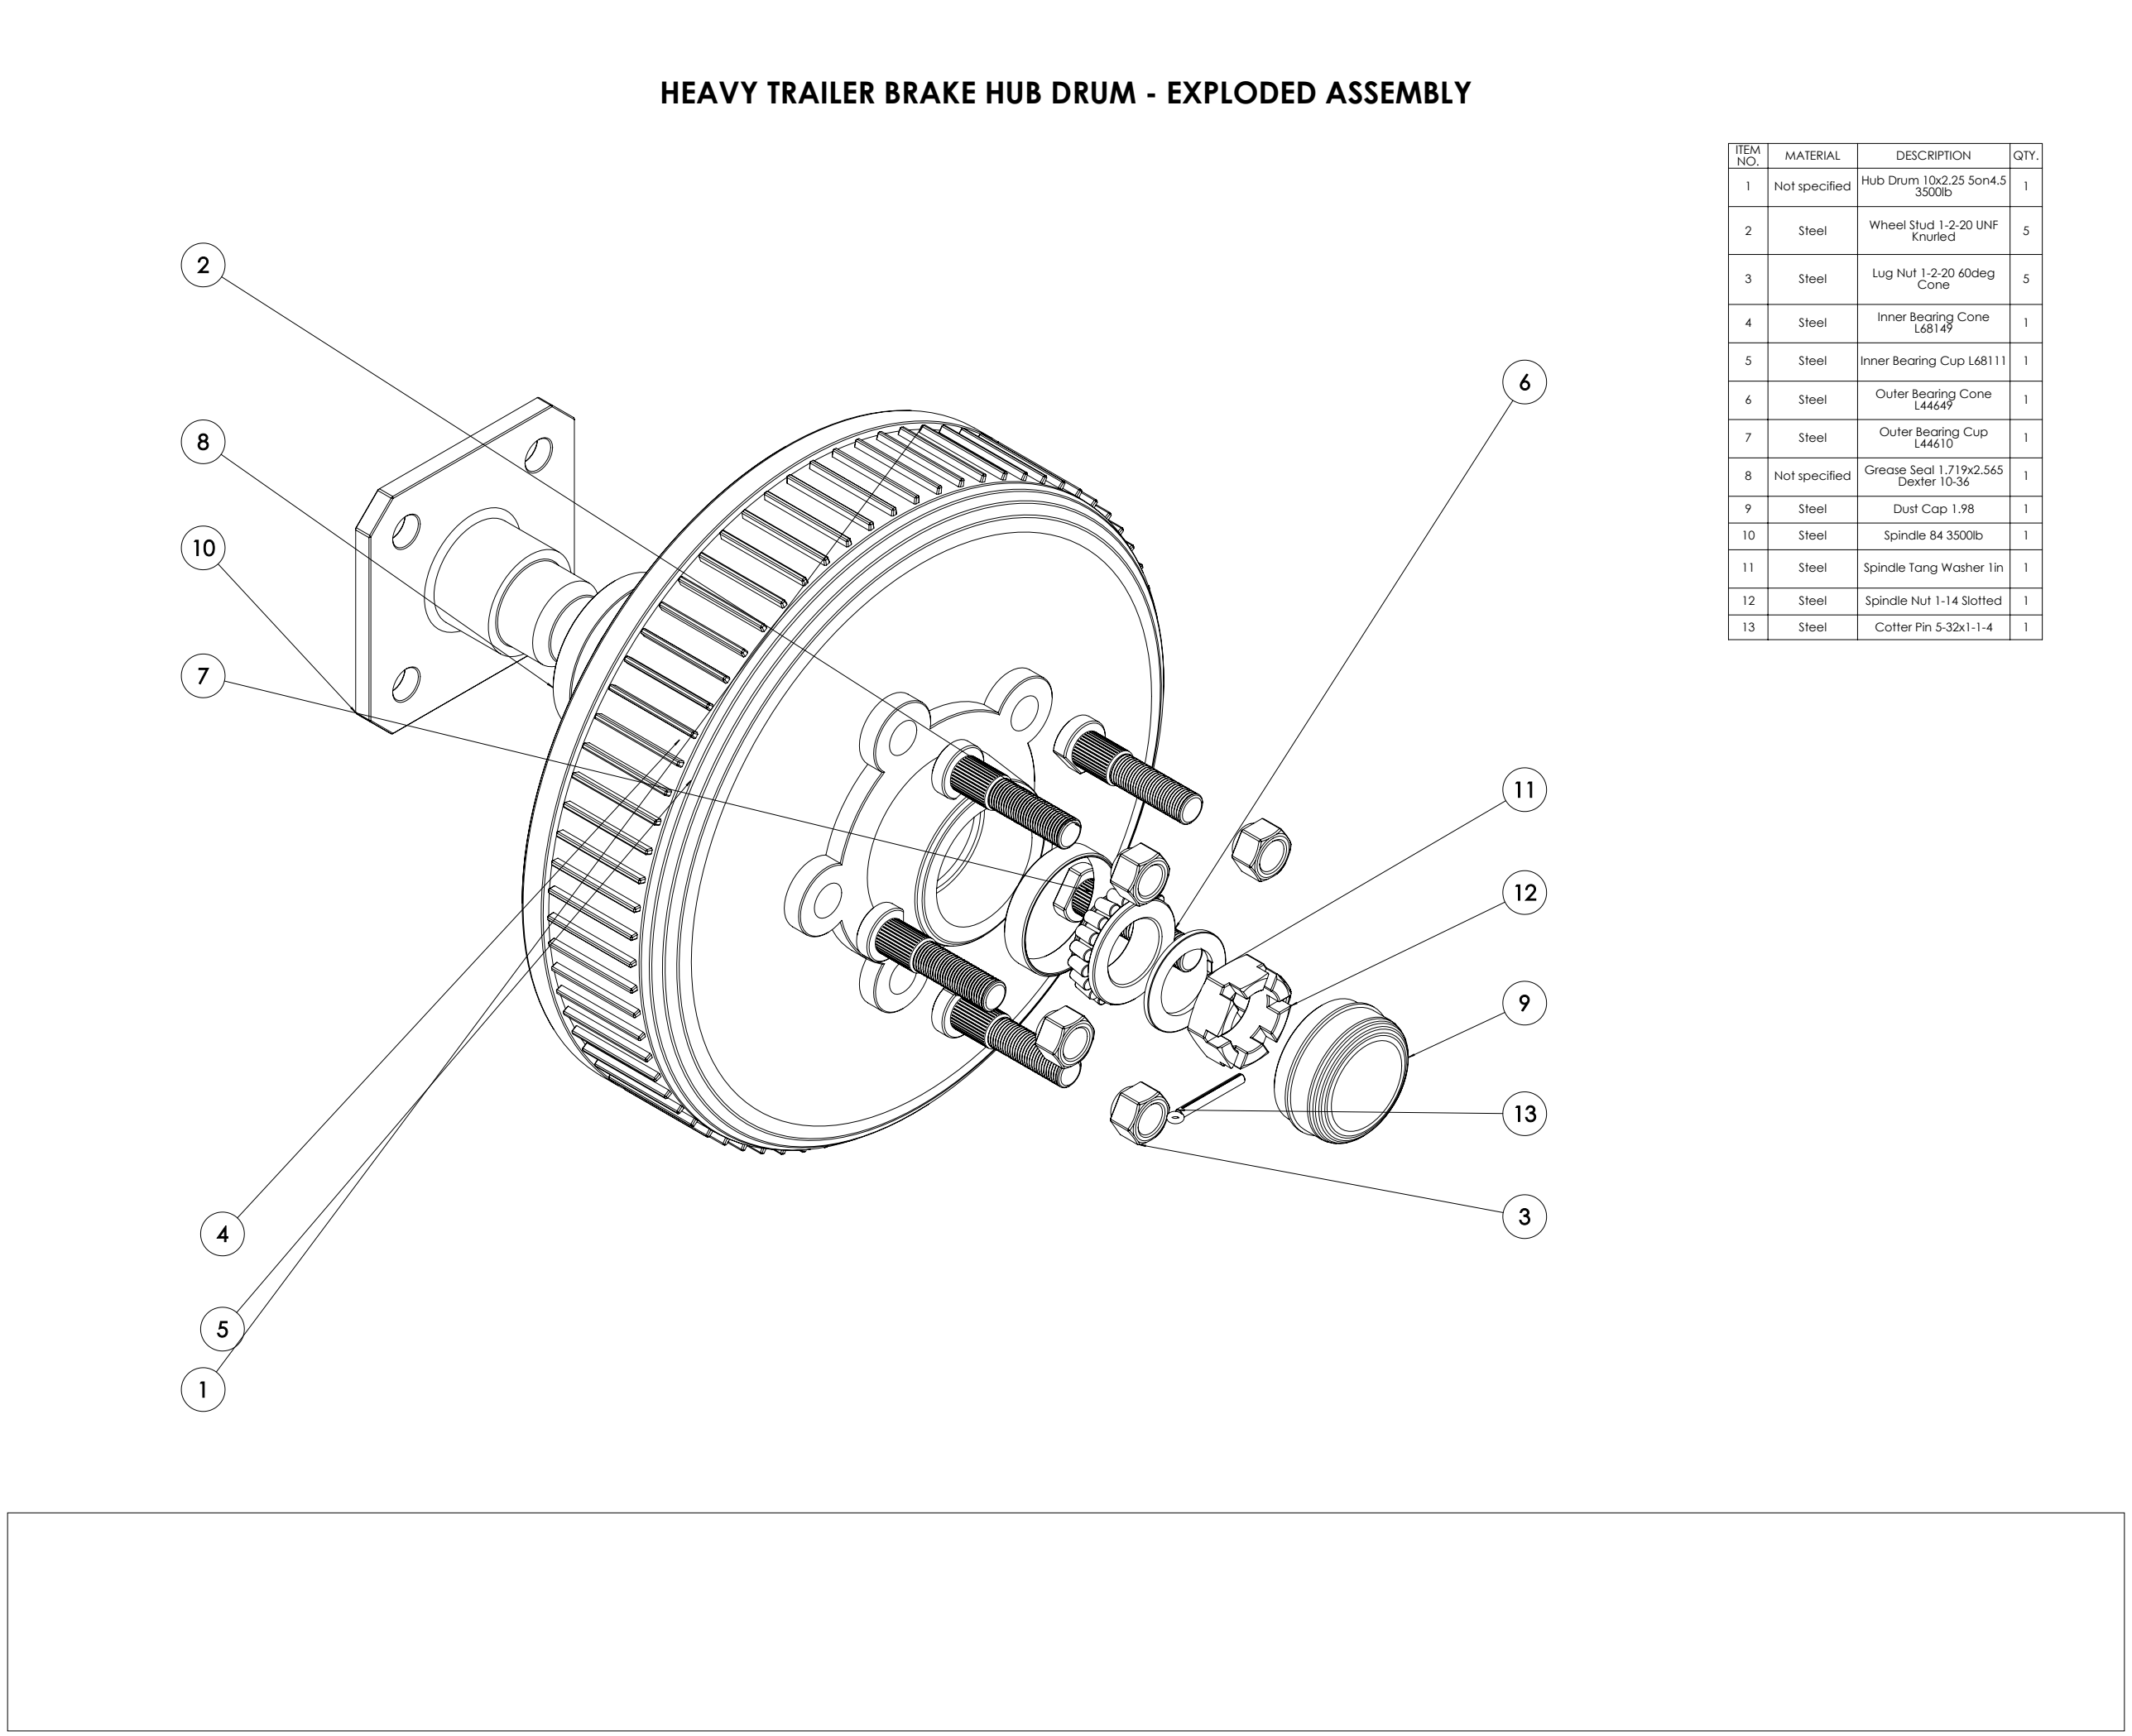
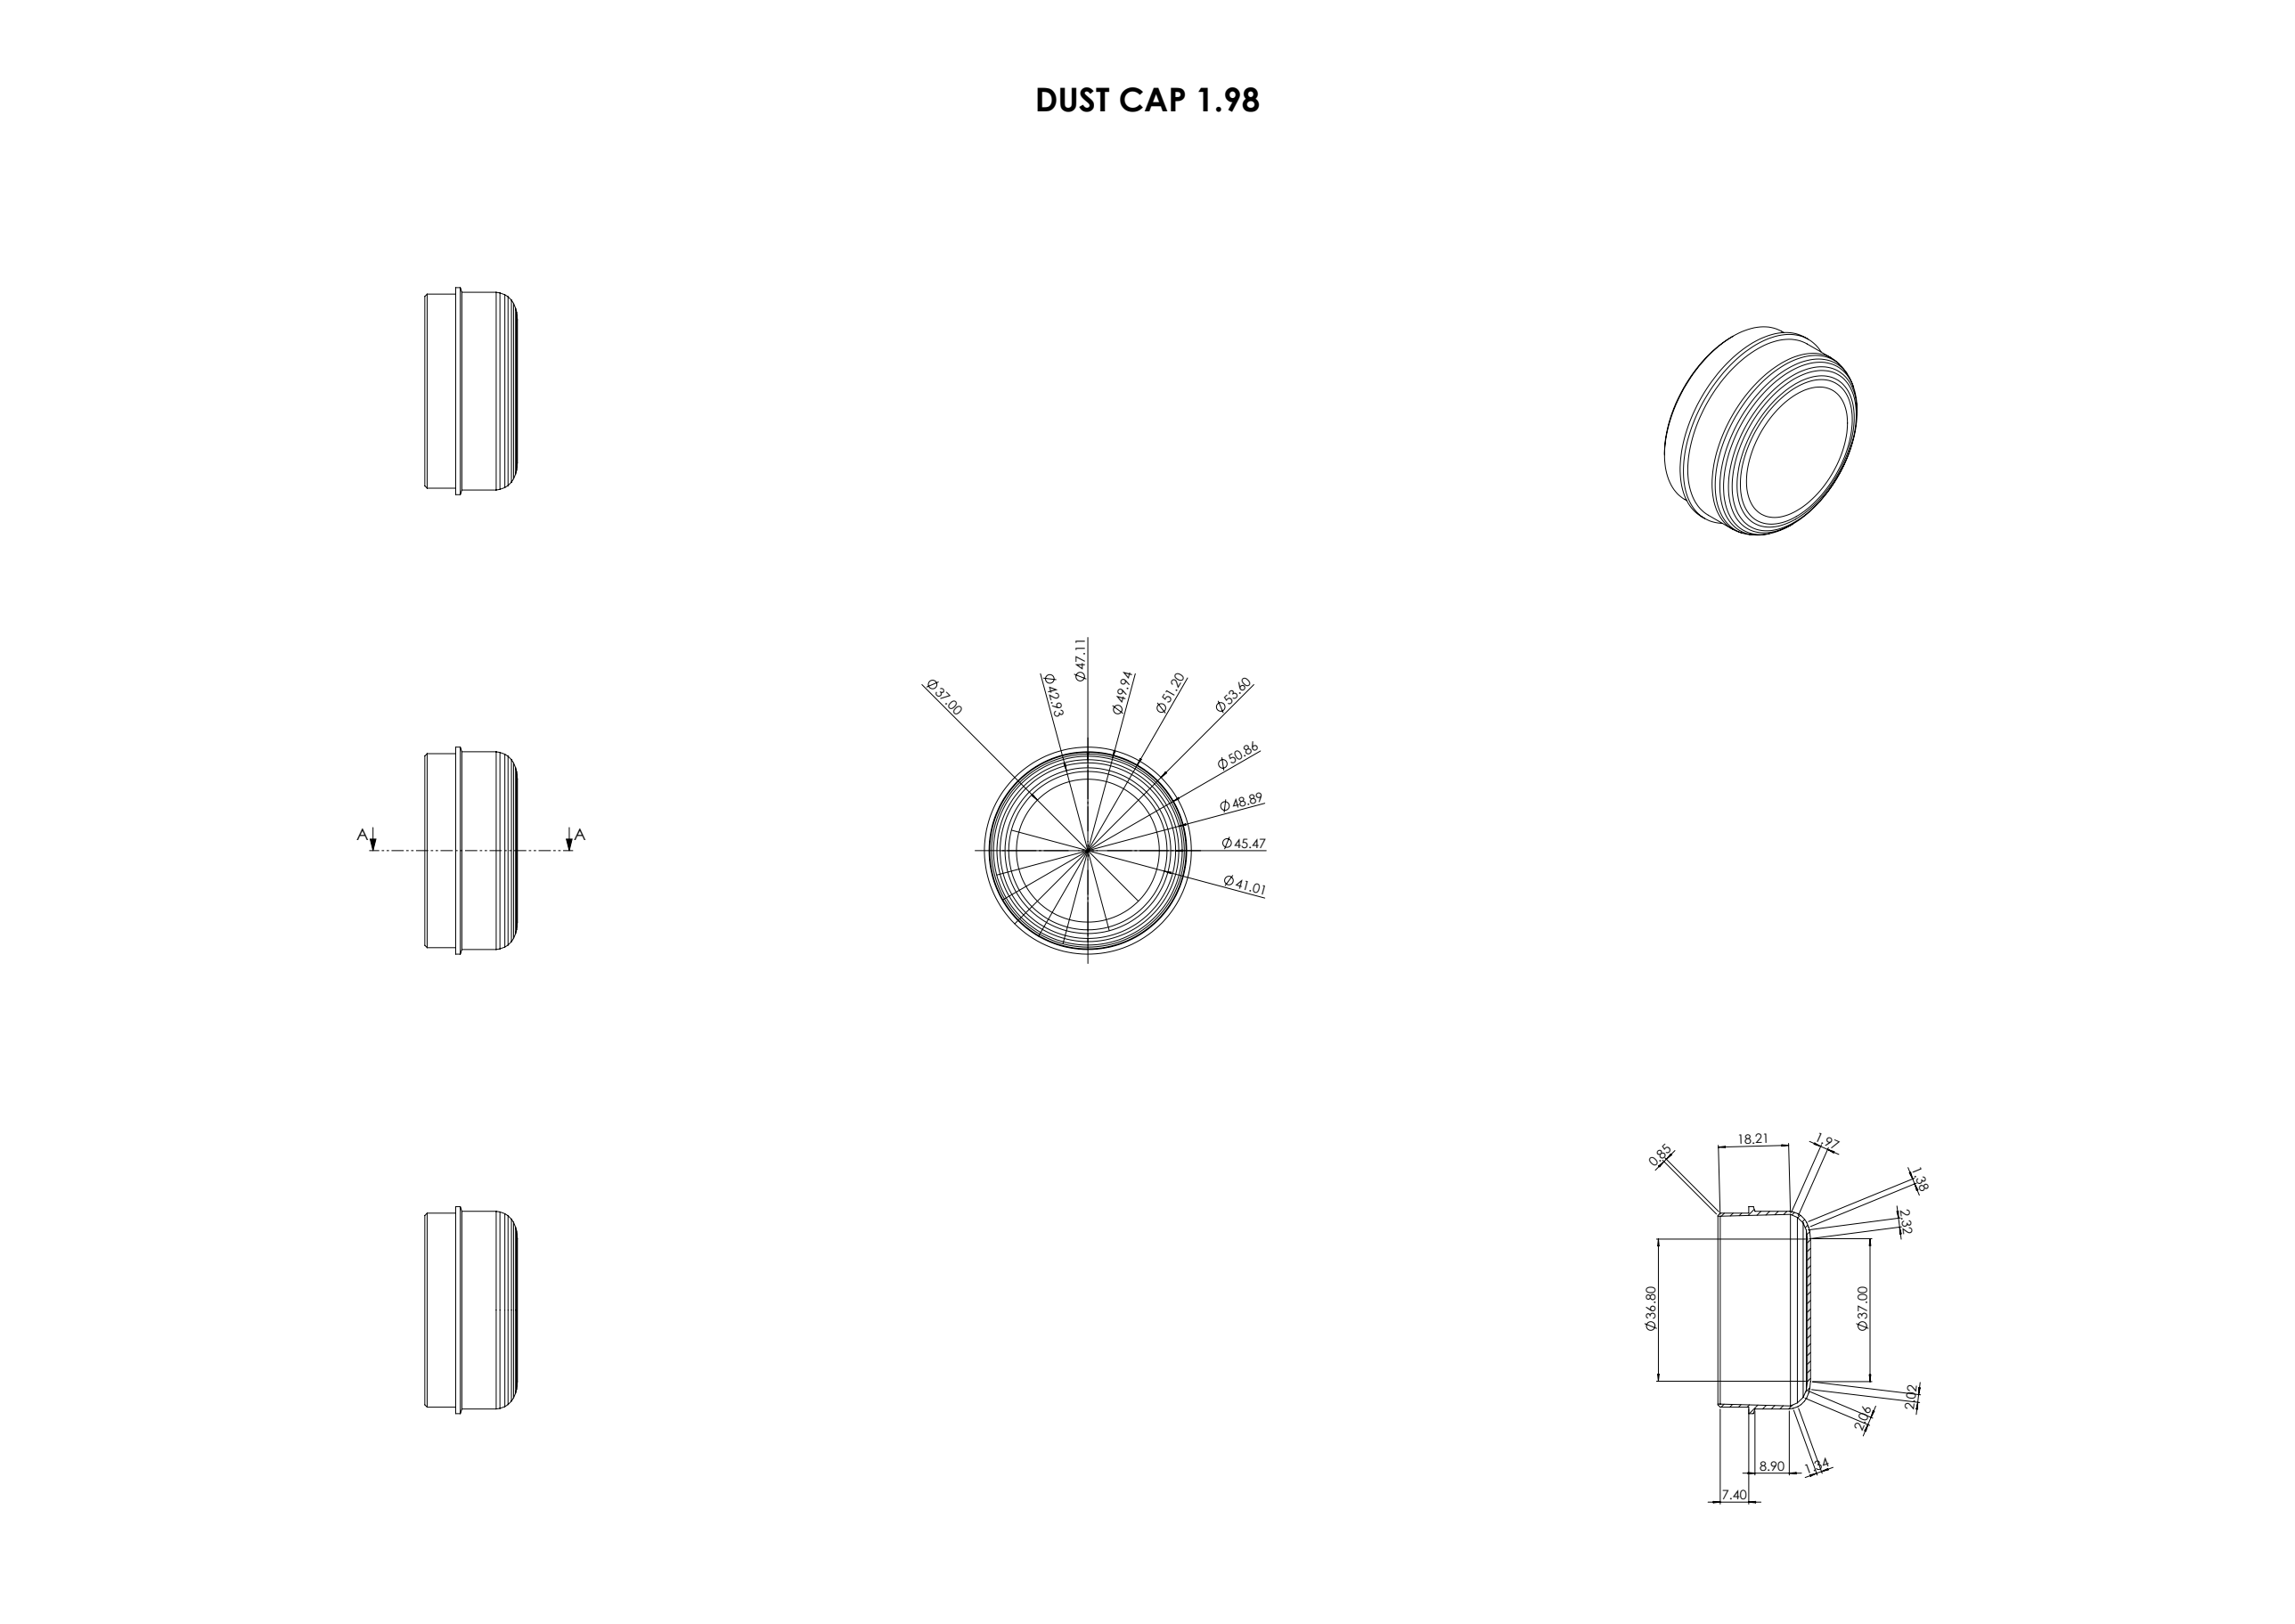
ISO-10303-21;
HEADER;
/* Generated by software containing ST-Developer
 * from STEP Tools, Inc. (www.steptools.com) 
 */

FILE_DESCRIPTION(
/* description */ (''),
/* implementation_level */ '2;1');

FILE_NAME(
/* name */ 'MAS-498',
/* time_stamp */ '2026-10-25T01:26:34-07:00',
/* author */ (''),
/* organization */ (''),
/* preprocessor_version */ 'ST-DEVELOPER v20.2',
/* originating_system */ 'Autodesk Translation Framework v15.15.0.0',
/* authorisation */ '');

FILE_SCHEMA (('AUTOMOTIVE_DESIGN { 1 0 10303 214 3 1 1 }'));
ENDSEC;

DATA;
#10=MECHANICAL_DESIGN_GEOMETRIC_PRESENTATION_REPRESENTATION('',(#321,#322,
#323,#324,#325,#326,#327,#328,#329,#330,#331,#332,#333),#71628);
#11=ITEM_DEFINED_TRANSFORMATION($,$,#34366,#37640);
#12=ITEM_DEFINED_TRANSFORMATION($,$,#36166,#37641);
#13=ITEM_DEFINED_TRANSFORMATION($,$,#36341,#37642);
#14=ITEM_DEFINED_TRANSFORMATION($,$,#36377,#37643);
#15=ITEM_DEFINED_TRANSFORMATION($,$,#36394,#37644);
#16=ITEM_DEFINED_TRANSFORMATION($,$,#36711,#37645);
#17=ITEM_DEFINED_TRANSFORMATION($,$,#36728,#37646);
#18=ITEM_DEFINED_TRANSFORMATION($,$,#37019,#37647);
#19=ITEM_DEFINED_TRANSFORMATION($,$,#37037,#37648);
#20=ITEM_DEFINED_TRANSFORMATION($,$,#37185,#37649);
#21=ITEM_DEFINED_TRANSFORMATION($,$,#37215,#37650);
#22=ITEM_DEFINED_TRANSFORMATION($,$,#37269,#37651);
#23=ITEM_DEFINED_TRANSFORMATION($,$,#37583,#37652);
#24=ITEM_DEFINED_TRANSFORMATION($,$,#37269,#37653);
#25=ITEM_DEFINED_TRANSFORMATION($,$,#37583,#37654);
#26=ITEM_DEFINED_TRANSFORMATION($,$,#37269,#37655);
#27=ITEM_DEFINED_TRANSFORMATION($,$,#37583,#37656);
#28=ITEM_DEFINED_TRANSFORMATION($,$,#37269,#37657);
#29=ITEM_DEFINED_TRANSFORMATION($,$,#37583,#37658);
#30=ITEM_DEFINED_TRANSFORMATION($,$,#37269,#37659);
#31=ITEM_DEFINED_TRANSFORMATION($,$,#37583,#37660);
#32=(
REPRESENTATION_RELATIONSHIP($,$,#71683,#71682)
REPRESENTATION_RELATIONSHIP_WITH_TRANSFORMATION(#11)
SHAPE_REPRESENTATION_RELATIONSHIP()
);
#33=(
REPRESENTATION_RELATIONSHIP($,$,#71684,#71682)
REPRESENTATION_RELATIONSHIP_WITH_TRANSFORMATION(#12)
SHAPE_REPRESENTATION_RELATIONSHIP()
);
#34=(
REPRESENTATION_RELATIONSHIP($,$,#71685,#71682)
REPRESENTATION_RELATIONSHIP_WITH_TRANSFORMATION(#13)
SHAPE_REPRESENTATION_RELATIONSHIP()
);
#35=(
REPRESENTATION_RELATIONSHIP($,$,#71686,#71682)
REPRESENTATION_RELATIONSHIP_WITH_TRANSFORMATION(#14)
SHAPE_REPRESENTATION_RELATIONSHIP()
);
#36=(
REPRESENTATION_RELATIONSHIP($,$,#71687,#71682)
REPRESENTATION_RELATIONSHIP_WITH_TRANSFORMATION(#15)
SHAPE_REPRESENTATION_RELATIONSHIP()
);
#37=(
REPRESENTATION_RELATIONSHIP($,$,#71688,#71682)
REPRESENTATION_RELATIONSHIP_WITH_TRANSFORMATION(#16)
SHAPE_REPRESENTATION_RELATIONSHIP()
);
#38=(
REPRESENTATION_RELATIONSHIP($,$,#71689,#71682)
REPRESENTATION_RELATIONSHIP_WITH_TRANSFORMATION(#17)
SHAPE_REPRESENTATION_RELATIONSHIP()
);
#39=(
REPRESENTATION_RELATIONSHIP($,$,#71690,#71682)
REPRESENTATION_RELATIONSHIP_WITH_TRANSFORMATION(#18)
SHAPE_REPRESENTATION_RELATIONSHIP()
);
#40=(
REPRESENTATION_RELATIONSHIP($,$,#71691,#71682)
REPRESENTATION_RELATIONSHIP_WITH_TRANSFORMATION(#19)
SHAPE_REPRESENTATION_RELATIONSHIP()
);
#41=(
REPRESENTATION_RELATIONSHIP($,$,#71692,#71682)
REPRESENTATION_RELATIONSHIP_WITH_TRANSFORMATION(#20)
SHAPE_REPRESENTATION_RELATIONSHIP()
);
#42=(
REPRESENTATION_RELATIONSHIP($,$,#71693,#71682)
REPRESENTATION_RELATIONSHIP_WITH_TRANSFORMATION(#21)
SHAPE_REPRESENTATION_RELATIONSHIP()
);
#43=(
REPRESENTATION_RELATIONSHIP($,$,#71694,#71682)
REPRESENTATION_RELATIONSHIP_WITH_TRANSFORMATION(#22)
SHAPE_REPRESENTATION_RELATIONSHIP()
);
#44=(
REPRESENTATION_RELATIONSHIP($,$,#71695,#71682)
REPRESENTATION_RELATIONSHIP_WITH_TRANSFORMATION(#23)
SHAPE_REPRESENTATION_RELATIONSHIP()
);
#45=(
REPRESENTATION_RELATIONSHIP($,$,#71694,#71682)
REPRESENTATION_RELATIONSHIP_WITH_TRANSFORMATION(#24)
SHAPE_REPRESENTATION_RELATIONSHIP()
);
#46=(
REPRESENTATION_RELATIONSHIP($,$,#71695,#71682)
REPRESENTATION_RELATIONSHIP_WITH_TRANSFORMATION(#25)
SHAPE_REPRESENTATION_RELATIONSHIP()
);
#47=(
REPRESENTATION_RELATIONSHIP($,$,#71694,#71682)
REPRESENTATION_RELATIONSHIP_WITH_TRANSFORMATION(#26)
SHAPE_REPRESENTATION_RELATIONSHIP()
);
#48=(
REPRESENTATION_RELATIONSHIP($,$,#71695,#71682)
REPRESENTATION_RELATIONSHIP_WITH_TRANSFORMATION(#27)
SHAPE_REPRESENTATION_RELATIONSHIP()
);
#49=(
REPRESENTATION_RELATIONSHIP($,$,#71694,#71682)
REPRESENTATION_RELATIONSHIP_WITH_TRANSFORMATION(#28)
SHAPE_REPRESENTATION_RELATIONSHIP()
);
#50=(
REPRESENTATION_RELATIONSHIP($,$,#71695,#71682)
REPRESENTATION_RELATIONSHIP_WITH_TRANSFORMATION(#29)
SHAPE_REPRESENTATION_RELATIONSHIP()
);
#51=(
REPRESENTATION_RELATIONSHIP($,$,#71694,#71682)
REPRESENTATION_RELATIONSHIP_WITH_TRANSFORMATION(#30)
SHAPE_REPRESENTATION_RELATIONSHIP()
);
#52=(
REPRESENTATION_RELATIONSHIP($,$,#71695,#71682)
REPRESENTATION_RELATIONSHIP_WITH_TRANSFORMATION(#31)
SHAPE_REPRESENTATION_RELATIONSHIP()
);
#53=CONTEXT_DEPENDENT_SHAPE_REPRESENTATION(#32,#71661);
#54=CONTEXT_DEPENDENT_SHAPE_REPRESENTATION(#33,#71662);
#55=CONTEXT_DEPENDENT_SHAPE_REPRESENTATION(#34,#71663);
#56=CONTEXT_DEPENDENT_SHAPE_REPRESENTATION(#35,#71664);
#57=CONTEXT_DEPENDENT_SHAPE_REPRESENTATION(#36,#71665);
#58=CONTEXT_DEPENDENT_SHAPE_REPRESENTATION(#37,#71666);
#59=CONTEXT_DEPENDENT_SHAPE_REPRESENTATION(#38,#71667);
#60=CONTEXT_DEPENDENT_SHAPE_REPRESENTATION(#39,#71668);
#61=CONTEXT_DEPENDENT_SHAPE_REPRESENTATION(#40,#71669);
#62=CONTEXT_DEPENDENT_SHAPE_REPRESENTATION(#41,#71670);
#63=CONTEXT_DEPENDENT_SHAPE_REPRESENTATION(#42,#71671);
#64=CONTEXT_DEPENDENT_SHAPE_REPRESENTATION(#43,#71672);
#65=CONTEXT_DEPENDENT_SHAPE_REPRESENTATION(#44,#71673);
#66=CONTEXT_DEPENDENT_SHAPE_REPRESENTATION(#45,#71674);
#67=CONTEXT_DEPENDENT_SHAPE_REPRESENTATION(#46,#71675);
#68=CONTEXT_DEPENDENT_SHAPE_REPRESENTATION(#47,#71676);
#69=CONTEXT_DEPENDENT_SHAPE_REPRESENTATION(#48,#71677);
#70=CONTEXT_DEPENDENT_SHAPE_REPRESENTATION(#49,#71678);
#71=CONTEXT_DEPENDENT_SHAPE_REPRESENTATION(#50,#71679);
#72=CONTEXT_DEPENDENT_SHAPE_REPRESENTATION(#51,#71680);
#73=CONTEXT_DEPENDENT_SHAPE_REPRESENTATION(#52,#71681);
#74=NEXT_ASSEMBLY_USAGE_OCCURRENCE(
'01_Hub_Drum_10x2.25_5on4.5_3500lb:2',
'01_Hub_Drum_10x2.25_5on4.5_3500lb:2',
'01_Hub_Drum_10x2.25_5on4.5_3500lb:2',#71697,#71698,
'01_Hub_Drum_10x2.25_5on4.5_3500lb:2');
#75=NEXT_ASSEMBLY_USAGE_OCCURRENCE('10_Spindle_84_3500lb:2',
'10_Spindle_84_3500lb:2','10_Spindle_84_3500lb:2',#71697,#71699,
'10_Spindle_84_3500lb:2');
#76=NEXT_ASSEMBLY_USAGE_OCCURRENCE(
'08_Grease_Seal_1.719x2.565_Dexter_10-36:2',
'08_Grease_Seal_1.719x2.565_Dexter_10-36:2',
'08_Grease_Seal_1.719x2.565_Dexter_10-36:2',#71697,#71700,
'08_Grease_Seal_1.719x2.565_Dexter_10-36:2');
#77=NEXT_ASSEMBLY_USAGE_OCCURRENCE('05_Inner_Bearing_Cup_L68111:2',
'05_Inner_Bearing_Cup_L68111:2','05_Inner_Bearing_Cup_L68111:2',#71697,
#71701,'05_Inner_Bearing_Cup_L68111:2');
#78=NEXT_ASSEMBLY_USAGE_OCCURRENCE('04_Inner_Bearing_Cone_L68149:2',
'04_Inner_Bearing_Cone_L68149:2','04_Inner_Bearing_Cone_L68149:2',#71697,
#71702,'04_Inner_Bearing_Cone_L68149:2');
#79=NEXT_ASSEMBLY_USAGE_OCCURRENCE('07_Outer_Bearing_Cup_L44610:2',
'07_Outer_Bearing_Cup_L44610:2','07_Outer_Bearing_Cup_L44610:2',#71697,
#71703,'07_Outer_Bearing_Cup_L44610:2');
#80=NEXT_ASSEMBLY_USAGE_OCCURRENCE('06_Outer_Bearing_Cone_L44649:2',
'06_Outer_Bearing_Cone_L44649:2','06_Outer_Bearing_Cone_L44649:2',#71697,
#71704,'06_Outer_Bearing_Cone_L44649:2');
#81=NEXT_ASSEMBLY_USAGE_OCCURRENCE('11_Spindle_Tang_Washer_1in:2',
'11_Spindle_Tang_Washer_1in:2','11_Spindle_Tang_Washer_1in:2',#71697,#71705,
'11_Spindle_Tang_Washer_1in:2');
#82=NEXT_ASSEMBLY_USAGE_OCCURRENCE('12_Spindle_Nut_1-14_Slotted:2',
'12_Spindle_Nut_1-14_Slotted:2','12_Spindle_Nut_1-14_Slotted:2',#71697,
#71706,'12_Spindle_Nut_1-14_Slotted:2');
#83=NEXT_ASSEMBLY_USAGE_OCCURRENCE('13_Cotter_Pin_5-32x1-1-4:2',
'13_Cotter_Pin_5-32x1-1-4:2','13_Cotter_Pin_5-32x1-1-4:2',#71697,#71707,
'13_Cotter_Pin_5-32x1-1-4:2');
#84=NEXT_ASSEMBLY_USAGE_OCCURRENCE('09_Dust_Cap_1.98:2',
'09_Dust_Cap_1.98:2','09_Dust_Cap_1.98:2',#71697,#71708,
'09_Dust_Cap_1.98:2');
#85=NEXT_ASSEMBLY_USAGE_OCCURRENCE('02_Wheel_Stud_1-2-20_UNF_Knurled:2',
'02_Wheel_Stud_1-2-20_UNF_Knurled:2',
'02_Wheel_Stud_1-2-20_UNF_Knurled:2',#71697,#71709,
'02_Wheel_Stud_1-2-20_UNF_Knurled:2');
#86=NEXT_ASSEMBLY_USAGE_OCCURRENCE('03_Lug_Nut_1-2-20_60deg_Cone:2',
'03_Lug_Nut_1-2-20_60deg_Cone:2','03_Lug_Nut_1-2-20_60deg_Cone:2',#71697,
#71710,'03_Lug_Nut_1-2-20_60deg_Cone:2');
#87=NEXT_ASSEMBLY_USAGE_OCCURRENCE('02_Wheel_Stud_1-2-20_UNF_Knurled:3',
'02_Wheel_Stud_1-2-20_UNF_Knurled:3',
'02_Wheel_Stud_1-2-20_UNF_Knurled:3',#71697,#71709,
'02_Wheel_Stud_1-2-20_UNF_Knurled:3');
#88=NEXT_ASSEMBLY_USAGE_OCCURRENCE('03_Lug_Nut_1-2-20_60deg_Cone:3',
'03_Lug_Nut_1-2-20_60deg_Cone:3','03_Lug_Nut_1-2-20_60deg_Cone:3',#71697,
#71710,'03_Lug_Nut_1-2-20_60deg_Cone:3');
#89=NEXT_ASSEMBLY_USAGE_OCCURRENCE('02_Wheel_Stud_1-2-20_UNF_Knurled:4',
'02_Wheel_Stud_1-2-20_UNF_Knurled:4',
'02_Wheel_Stud_1-2-20_UNF_Knurled:4',#71697,#71709,
'02_Wheel_Stud_1-2-20_UNF_Knurled:4');
#90=NEXT_ASSEMBLY_USAGE_OCCURRENCE('03_Lug_Nut_1-2-20_60deg_Cone:4',
'03_Lug_Nut_1-2-20_60deg_Cone:4','03_Lug_Nut_1-2-20_60deg_Cone:4',#71697,
#71710,'03_Lug_Nut_1-2-20_60deg_Cone:4');
#91=NEXT_ASSEMBLY_USAGE_OCCURRENCE('02_Wheel_Stud_1-2-20_UNF_Knurled:5',
'02_Wheel_Stud_1-2-20_UNF_Knurled:5',
'02_Wheel_Stud_1-2-20_UNF_Knurled:5',#71697,#71709,
'02_Wheel_Stud_1-2-20_UNF_Knurled:5');
#92=NEXT_ASSEMBLY_USAGE_OCCURRENCE('03_Lug_Nut_1-2-20_60deg_Cone:5',
'03_Lug_Nut_1-2-20_60deg_Cone:5','03_Lug_Nut_1-2-20_60deg_Cone:5',#71697,
#71710,'03_Lug_Nut_1-2-20_60deg_Cone:5');
#93=NEXT_ASSEMBLY_USAGE_OCCURRENCE('02_Wheel_Stud_1-2-20_UNF_Knurled:6',
'02_Wheel_Stud_1-2-20_UNF_Knurled:6',
'02_Wheel_Stud_1-2-20_UNF_Knurled:6',#71697,#71709,
'02_Wheel_Stud_1-2-20_UNF_Knurled:6');
#94=NEXT_ASSEMBLY_USAGE_OCCURRENCE('03_Lug_Nut_1-2-20_60deg_Cone:6',
'03_Lug_Nut_1-2-20_60deg_Cone:6','03_Lug_Nut_1-2-20_60deg_Cone:6',#71697,
#71710,'03_Lug_Nut_1-2-20_60deg_Cone:6');
#95=TOROIDAL_SURFACE('',#36358,25.4,0.8);
#96=TOROIDAL_SURFACE('',#36411,2.22978791005503,0.3);
#97=TOROIDAL_SURFACE('',#36419,2.56984636336567,0.3);
#98=TOROIDAL_SURFACE('',#36424,2.22978791005503,0.3);
#99=TOROIDAL_SURFACE('',#36432,2.56984636336567,0.3);
#100=TOROIDAL_SURFACE('',#36437,2.22978791005503,0.3);
#101=TOROIDAL_SURFACE('',#36445,2.56984636336567,0.3);
#102=TOROIDAL_SURFACE('',#36450,2.22978791005503,0.3);
#103=TOROIDAL_SURFACE('',#36458,2.56984636336567,0.3);
#104=TOROIDAL_SURFACE('',#36463,2.22978791005503,0.3);
#105=TOROIDAL_SURFACE('',#36471,2.56984636336567,0.3);
#106=TOROIDAL_SURFACE('',#36476,2.22978791005503,0.3);
#107=TOROIDAL_SURFACE('',#36484,2.56984636336567,0.3);
#108=TOROIDAL_SURFACE('',#36489,2.22978791005503,0.3);
#109=TOROIDAL_SURFACE('',#36497,2.56984636336567,0.3);
#110=TOROIDAL_SURFACE('',#36502,2.22978791005503,0.3);
#111=TOROIDAL_SURFACE('',#36510,2.56984636336567,0.3);
#112=TOROIDAL_SURFACE('',#36515,2.22978791005503,0.3);
#113=TOROIDAL_SURFACE('',#36523,2.56984636336567,0.3);
#114=TOROIDAL_SURFACE('',#36528,2.22978791005503,0.3);
#115=TOROIDAL_SURFACE('',#36536,2.56984636336567,0.3);
#116=TOROIDAL_SURFACE('',#36541,2.22978791005503,0.3);
#117=TOROIDAL_SURFACE('',#36549,2.56984636336567,0.3);
#118=TOROIDAL_SURFACE('',#36554,2.22978791005503,0.3);
#119=TOROIDAL_SURFACE('',#36562,2.56984636336567,0.3);
#120=TOROIDAL_SURFACE('',#36567,2.22978791005503,0.3);
#121=TOROIDAL_SURFACE('',#36575,2.56984636336567,0.3);
#122=TOROIDAL_SURFACE('',#36580,2.22978791005503,0.3);
#123=TOROIDAL_SURFACE('',#36588,2.56984636336567,0.3);
#124=TOROIDAL_SURFACE('',#36593,2.22978791005503,0.3);
#125=TOROIDAL_SURFACE('',#36601,2.56984636336567,0.3);
#126=TOROIDAL_SURFACE('',#36606,2.22978791005503,0.3);
#127=TOROIDAL_SURFACE('',#36614,2.56984636336567,0.3);
#128=TOROIDAL_SURFACE('',#36619,2.22978791005503,0.3);
#129=TOROIDAL_SURFACE('',#36627,2.56984636336567,0.3);
#130=TOROIDAL_SURFACE('',#36632,2.22978791005503,0.3);
#131=TOROIDAL_SURFACE('',#36640,2.56984636336567,0.3);
#132=TOROIDAL_SURFACE('',#36645,2.22978791005503,0.3);
#133=TOROIDAL_SURFACE('',#36653,2.56984636336567,0.3);
#134=TOROIDAL_SURFACE('',#36658,2.22978791005503,0.3);
#135=TOROIDAL_SURFACE('',#36666,2.56984636336567,0.3);
#136=TOROIDAL_SURFACE('',#36671,2.22978791005503,0.3);
#137=TOROIDAL_SURFACE('',#36679,2.56984636336567,0.3);
#138=TOROIDAL_SURFACE('',#36684,2.22978791005503,0.3);
#139=TOROIDAL_SURFACE('',#36692,2.56984636336567,0.3);
#140=TOROIDAL_SURFACE('',#36745,2.05196259868229,0.3);
#141=TOROIDAL_SURFACE('',#36753,2.34767167473842,0.3);
#142=TOROIDAL_SURFACE('',#36758,2.05196259868229,0.3);
#143=TOROIDAL_SURFACE('',#36766,2.34767167473842,0.3);
#144=TOROIDAL_SURFACE('',#36771,2.05196259868229,0.3);
#145=TOROIDAL_SURFACE('',#36779,2.34767167473842,0.3);
#146=TOROIDAL_SURFACE('',#36784,2.05196259868229,0.3);
#147=TOROIDAL_SURFACE('',#36792,2.34767167473842,0.3);
#148=TOROIDAL_SURFACE('',#36797,2.05196259868229,0.3);
#149=TOROIDAL_SURFACE('',#36805,2.34767167473842,0.3);
#150=TOROIDAL_SURFACE('',#36810,2.05196259868229,0.3);
#151=TOROIDAL_SURFACE('',#36818,2.34767167473842,0.3);
#152=TOROIDAL_SURFACE('',#36823,2.05196259868229,0.3);
#153=TOROIDAL_SURFACE('',#36831,2.34767167473842,0.3);
#154=TOROIDAL_SURFACE('',#36836,2.05196259868229,0.3);
#155=TOROIDAL_SURFACE('',#36844,2.34767167473842,0.3);
#156=TOROIDAL_SURFACE('',#36849,2.05196259868229,0.3);
#157=TOROIDAL_SURFACE('',#36857,2.34767167473842,0.3);
#158=TOROIDAL_SURFACE('',#36862,2.05196259868229,0.3);
#159=TOROIDAL_SURFACE('',#36870,2.34767167473842,0.3);
#160=TOROIDAL_SURFACE('',#36875,2.05196259868229,0.3);
#161=TOROIDAL_SURFACE('',#36883,2.34767167473842,0.3);
#162=TOROIDAL_SURFACE('',#36888,2.05196259868229,0.3);
#163=TOROIDAL_SURFACE('',#36896,2.34767167473842,0.3);
#164=TOROIDAL_SURFACE('',#36901,2.05196259868229,0.3);
#165=TOROIDAL_SURFACE('',#36909,2.34767167473842,0.3);
#166=TOROIDAL_SURFACE('',#36914,2.05196259868229,0.3);
#167=TOROIDAL_SURFACE('',#36922,2.34767167473842,0.3);
#168=TOROIDAL_SURFACE('',#36927,2.05196259868229,0.3);
#169=TOROIDAL_SURFACE('',#36935,2.34767167473842,0.3);
#170=TOROIDAL_SURFACE('',#36940,2.05196259868229,0.3);
#171=TOROIDAL_SURFACE('',#36948,2.34767167473842,0.3);
#172=TOROIDAL_SURFACE('',#36953,2.05196259868229,0.3);
#173=TOROIDAL_SURFACE('',#36961,2.34767167473842,0.3);
#174=TOROIDAL_SURFACE('',#36966,2.05196259868229,0.3);
#175=TOROIDAL_SURFACE('',#36974,2.34767167473842,0.3);
#176=TOROIDAL_SURFACE('',#36979,2.05196259868229,0.3);
#177=TOROIDAL_SURFACE('',#36987,2.34767167473842,0.3);
#178=TOROIDAL_SURFACE('',#36992,2.05196259868229,0.3);
#179=TOROIDAL_SURFACE('',#37000,2.34767167473842,0.3);
#180=TOROIDAL_SURFACE('',#37211,2.29999999999999,0.999999999999996);
#181=(
BOUNDED_CURVE()
B_SPLINE_CURVE(2,(#57816,#57817,#57818),.UNSPECIFIED.,.F.,.F.)
B_SPLINE_CURVE_WITH_KNOTS((3,3),(0.0552009552934231,0.395576151489963),
 .UNSPECIFIED.)
CURVE()
GEOMETRIC_REPRESENTATION_ITEM()
RATIONAL_B_SPLINE_CURVE((1.00343876873283,1.01256123126711,1.00343876873283))
REPRESENTATION_ITEM('')
);
#182=(
BOUNDED_CURVE()
B_SPLINE_CURVE(2,(#57942,#57943,#57944),.UNSPECIFIED.,.F.,.F.)
B_SPLINE_CURVE_WITH_KNOTS((3,3),(0.0550683626555145,0.394625977980432),
 .UNSPECIFIED.)
CURVE()
GEOMETRIC_REPRESENTATION_ITEM()
RATIONAL_B_SPLINE_CURVE((1.00343876873282,1.01256123126706,1.00343876873282))
REPRESENTATION_ITEM('')
);
#183=(
BOUNDED_CURVE()
B_SPLINE_CURVE(2,(#61982,#61983,#61984),.UNSPECIFIED.,.F.,.F.)
B_SPLINE_CURVE_WITH_KNOTS((3,3),(0.0551833308085786,0.208603356030854),
 .UNSPECIFIED.)
CURVE()
GEOMETRIC_REPRESENTATION_ITEM()
RATIONAL_B_SPLINE_CURVE((1.00066796366419,1.00140515246647,1.00107839993824))
REPRESENTATION_ITEM('')
);
#184=(
BOUNDED_CURVE()
B_SPLINE_CURVE(2,(#61988,#61989,#61990),.UNSPECIFIED.,.F.,.F.)
B_SPLINE_CURVE_WITH_KNOTS((3,3),(0.,0.0415381994417814),.UNSPECIFIED.)
CURVE()
GEOMETRIC_REPRESENTATION_ITEM()
RATIONAL_B_SPLINE_CURVE((1.,1.,1.))
REPRESENTATION_ITEM('')
);
#185=(
BOUNDED_CURVE()
B_SPLINE_CURVE(2,(#62002,#62003,#62004),.UNSPECIFIED.,.F.,.F.)
B_SPLINE_CURVE_WITH_KNOTS((3,3),(0.146737168363919,0.166814895713845),
 .UNSPECIFIED.)
CURVE()
GEOMETRIC_REPRESENTATION_ITEM()
RATIONAL_B_SPLINE_CURVE((1.00169850871231,1.00172953563108,1.00173725401054))
REPRESENTATION_ITEM('')
);
#186=(
BOUNDED_CURVE()
B_SPLINE_CURVE(2,(#62006,#62007,#62008),.UNSPECIFIED.,.F.,.F.)
B_SPLINE_CURVE_WITH_KNOTS((3,3),(0.0286170700108403,0.0762123799831723),
 .UNSPECIFIED.)
CURVE()
GEOMETRIC_REPRESENTATION_ITEM()
RATIONAL_B_SPLINE_CURVE((1.00112886559711,1.00201824869615,1.00274341056429))
REPRESENTATION_ITEM('')
);
#187=(
BOUNDED_CURVE()
B_SPLINE_CURVE(2,(#62010,#62011,#62012),.UNSPECIFIED.,.F.,.F.)
B_SPLINE_CURVE_WITH_KNOTS((3,3),(0.460004626021665,2.01415548066414),
 .UNSPECIFIED.)
CURVE()
GEOMETRIC_REPRESENTATION_ITEM()
RATIONAL_B_SPLINE_CURVE((1.06220108868579,1.14327836336947,1.06220108868485))
REPRESENTATION_ITEM('')
);
#188=(
BOUNDED_CURVE()
B_SPLINE_CURVE(2,(#62014,#62015,#62016),.UNSPECIFIED.,.F.,.F.)
B_SPLINE_CURVE_WITH_KNOTS((3,3),(0.517898922485183,0.565329042615563),
 .UNSPECIFIED.)
CURVE()
GEOMETRIC_REPRESENTATION_ITEM()
RATIONAL_B_SPLINE_CURVE((1.00287035745076,1.00210549051843,1.00117645345012))
REPRESENTATION_ITEM('')
);
#189=(
BOUNDED_CURVE()
B_SPLINE_CURVE(2,(#62018,#62019,#62020),.UNSPECIFIED.,.F.,.F.)
B_SPLINE_CURVE_WITH_KNOTS((3,3),(0.180111955302705,0.200189682652632),
 .UNSPECIFIED.)
CURVE()
GEOMETRIC_REPRESENTATION_ITEM()
RATIONAL_B_SPLINE_CURVE((1.00173725403577,1.00172953565623,1.00169850873703))
REPRESENTATION_ITEM('')
);
#190=(
BOUNDED_CURVE()
B_SPLINE_CURVE(2,(#62021,#62022,#62023),.UNSPECIFIED.,.F.,.F.)
B_SPLINE_CURVE_WITH_KNOTS((3,3),(0.135718481594952,0.289180967053373),
 .UNSPECIFIED.)
CURVE()
GEOMETRIC_REPRESENTATION_ITEM()
RATIONAL_B_SPLINE_CURVE((1.00140882606001,1.0017347183849,1.00099631962994))
REPRESENTATION_ITEM('')
);
#191=(
BOUNDED_CURVE()
B_SPLINE_CURVE(2,(#62028,#62029,#62030),.UNSPECIFIED.,.F.,.F.)
B_SPLINE_CURVE_WITH_KNOTS((3,3),(-2.1703979840528,-2.16974314947152),
 .UNSPECIFIED.)
CURVE()
GEOMETRIC_REPRESENTATION_ITEM()
RATIONAL_B_SPLINE_CURVE((1.2052492603669,1.20540347259793,1.20555757308983))
REPRESENTATION_ITEM('')
);
#192=(
BOUNDED_CURVE()
B_SPLINE_CURVE(2,(#62060,#62061,#62062),.UNSPECIFIED.,.F.,.F.)
B_SPLINE_CURVE_WITH_KNOTS((3,3),(-0.363565876377553,-0.362911041796276),
 .UNSPECIFIED.)
CURVE()
GEOMETRIC_REPRESENTATION_ITEM()
RATIONAL_B_SPLINE_CURVE((1.20555757308983,1.20540347259792,1.20524926036689))
REPRESENTATION_ITEM('')
);
#193=(
BOUNDED_CURVE()
B_SPLINE_CURVE(2,(#62082,#62083,#62084),.UNSPECIFIED.,.F.,.F.)
B_SPLINE_CURVE_WITH_KNOTS((3,3),(0.0400329798995012,0.0815711793412347),
 .UNSPECIFIED.)
CURVE()
GEOMETRIC_REPRESENTATION_ITEM()
RATIONAL_B_SPLINE_CURVE((1.,1.,1.))
REPRESENTATION_ITEM('')
);
#194=(
BOUNDED_CURVE()
B_SPLINE_CURVE(2,(#62105,#62106,#62107),.UNSPECIFIED.,.F.,.F.)
B_SPLINE_CURVE_WITH_KNOTS((3,3),(0.280206015619899,0.367357794870773),
 .UNSPECIFIED.)
CURVE()
GEOMETRIC_REPRESENTATION_ITEM()
RATIONAL_B_SPLINE_CURVE((1.0058941656769,1.00611162505668,1.0058941656769))
REPRESENTATION_ITEM('')
);
#195=(
BOUNDED_CURVE()
B_SPLINE_CURVE(2,(#62117,#62118,#62119),.UNSPECIFIED.,.F.,.F.)
B_SPLINE_CURVE_WITH_KNOTS((3,3),(0.460004626021663,2.01415548066414),
 .UNSPECIFIED.)
CURVE()
GEOMETRIC_REPRESENTATION_ITEM()
RATIONAL_B_SPLINE_CURVE((1.06220108868579,1.14327836336948,1.06220108868485))
REPRESENTATION_ITEM('')
);
#196=(
BOUNDED_CURVE()
B_SPLINE_CURVE(2,(#62126,#62127,#62128),.UNSPECIFIED.,.F.,.F.)
B_SPLINE_CURVE_WITH_KNOTS((3,3),(0.196145060700811,2.27801504598277),
 .UNSPECIFIED.)
CURVE()
GEOMETRIC_REPRESENTATION_ITEM()
RATIONAL_B_SPLINE_CURVE((1.02999692649796,1.17548252555731,1.02999692649702))
REPRESENTATION_ITEM('')
);
#197=(
BOUNDED_CURVE()
B_SPLINE_CURVE(2,(#62143,#62144,#62145),.UNSPECIFIED.,.F.,.F.)
B_SPLINE_CURVE_WITH_KNOTS((3,3),(0.0551833308085729,0.208603356030911),
 .UNSPECIFIED.)
CURVE()
GEOMETRIC_REPRESENTATION_ITEM()
RATIONAL_B_SPLINE_CURVE((1.00066796366438,1.00140515246685,1.00107839993854))
REPRESENTATION_ITEM('')
);
#198=(
BOUNDED_CURVE()
B_SPLINE_CURVE(2,(#62149,#62150,#62151),.UNSPECIFIED.,.F.,.F.)
B_SPLINE_CURVE_WITH_KNOTS((3,3),(0.,0.0415381994417707),.UNSPECIFIED.)
CURVE()
GEOMETRIC_REPRESENTATION_ITEM()
RATIONAL_B_SPLINE_CURVE((1.,1.,1.))
REPRESENTATION_ITEM('')
);
#199=(
BOUNDED_CURVE()
B_SPLINE_CURVE(2,(#62159,#62160,#62161),.UNSPECIFIED.,.F.,.F.)
B_SPLINE_CURVE_WITH_KNOTS((3,3),(0.0400329798994619,0.0815711793412169),
 .UNSPECIFIED.)
CURVE()
GEOMETRIC_REPRESENTATION_ITEM()
RATIONAL_B_SPLINE_CURVE((1.,1.,1.))
REPRESENTATION_ITEM('')
);
#200=(
BOUNDED_CURVE()
B_SPLINE_CURVE(2,(#62179,#62180,#62181),.UNSPECIFIED.,.F.,.F.)
B_SPLINE_CURVE_WITH_KNOTS((3,3),(0.146737168392566,0.16681489574343),
 .UNSPECIFIED.)
CURVE()
GEOMETRIC_REPRESENTATION_ITEM()
RATIONAL_B_SPLINE_CURVE((1.00169850874089,1.00172953566016,1.00173725403971))
REPRESENTATION_ITEM('')
);
#201=(
BOUNDED_CURVE()
B_SPLINE_CURVE(2,(#62183,#62184,#62185),.UNSPECIFIED.,.F.,.F.)
B_SPLINE_CURVE_WITH_KNOTS((3,3),(0.0286170700108407,0.0762123799831754),
 .UNSPECIFIED.)
CURVE()
GEOMETRIC_REPRESENTATION_ITEM()
RATIONAL_B_SPLINE_CURVE((1.0011288655971,1.00201824869615,1.00274341056429))
REPRESENTATION_ITEM('')
);
#202=(
BOUNDED_CURVE()
B_SPLINE_CURVE(2,(#62187,#62188,#62189),.UNSPECIFIED.,.F.,.F.)
B_SPLINE_CURVE_WITH_KNOTS((3,3),(0.460004626021664,2.01415548066414),
 .UNSPECIFIED.)
CURVE()
GEOMETRIC_REPRESENTATION_ITEM()
RATIONAL_B_SPLINE_CURVE((1.06220108868579,1.14327836336947,1.06220108868485))
REPRESENTATION_ITEM('')
);
#203=(
BOUNDED_CURVE()
B_SPLINE_CURVE(2,(#62191,#62192,#62193),.UNSPECIFIED.,.F.,.F.)
B_SPLINE_CURVE_WITH_KNOTS((3,3),(0.517898922485173,0.565329042615554),
 .UNSPECIFIED.)
CURVE()
GEOMETRIC_REPRESENTATION_ITEM()
RATIONAL_B_SPLINE_CURVE((1.00287035745075,1.00210549051842,1.00117645345012))
REPRESENTATION_ITEM('')
);
#204=(
BOUNDED_CURVE()
B_SPLINE_CURVE(2,(#62195,#62196,#62197),.UNSPECIFIED.,.F.,.F.)
B_SPLINE_CURVE_WITH_KNOTS((3,3),(0.180111955322094,0.200189682671483),
 .UNSPECIFIED.)
CURVE()
GEOMETRIC_REPRESENTATION_ITEM()
RATIONAL_B_SPLINE_CURVE((1.00173725402072,1.00172953564122,1.00169850872227))
REPRESENTATION_ITEM('')
);
#205=(
BOUNDED_CURVE()
B_SPLINE_CURVE(2,(#62198,#62199,#62200),.UNSPECIFIED.,.F.,.F.)
B_SPLINE_CURVE_WITH_KNOTS((3,3),(0.13571848159495,0.289180967053359),
 .UNSPECIFIED.)
CURVE()
GEOMETRIC_REPRESENTATION_ITEM()
RATIONAL_B_SPLINE_CURVE((1.00140882605995,1.00173471838483,1.0009963196299))
REPRESENTATION_ITEM('')
);
#206=(
BOUNDED_CURVE()
B_SPLINE_CURVE(2,(#62208,#62209,#62210),.UNSPECIFIED.,.F.,.F.)
B_SPLINE_CURVE_WITH_KNOTS((3,3),(0.280206015619895,0.367357794870771),
 .UNSPECIFIED.)
CURVE()
GEOMETRIC_REPRESENTATION_ITEM()
RATIONAL_B_SPLINE_CURVE((1.00589416567692,1.0061116250567,1.00589416567692))
REPRESENTATION_ITEM('')
);
#207=(
BOUNDED_CURVE()
B_SPLINE_CURVE(2,(#62214,#62215,#62216),.UNSPECIFIED.,.F.,.F.)
B_SPLINE_CURVE_WITH_KNOTS((3,3),(0.196145060700812,2.27801504598277),
 .UNSPECIFIED.)
CURVE()
GEOMETRIC_REPRESENTATION_ITEM()
RATIONAL_B_SPLINE_CURVE((1.02999692649796,1.1754825255573,1.02999692649702))
REPRESENTATION_ITEM('')
);
#208=(
BOUNDED_CURVE()
B_SPLINE_CURVE(2,(#62227,#62228,#62229),.UNSPECIFIED.,.F.,.F.)
B_SPLINE_CURVE_WITH_KNOTS((3,3),(0.196145060700811,1.23708005334447),
 .UNSPECIFIED.)
CURVE()
GEOMETRIC_REPRESENTATION_ITEM()
RATIONAL_B_SPLINE_CURVE((1.02999692649796,1.10273972602782,1.1027397260274))
REPRESENTATION_ITEM('')
);
#209=(
BOUNDED_CURVE()
B_SPLINE_CURVE(2,(#62231,#62232,#62233),.UNSPECIFIED.,.F.,.F.)
B_SPLINE_CURVE_WITH_KNOTS((3,3),(0.280206015619894,0.367357794870769),
 .UNSPECIFIED.)
CURVE()
GEOMETRIC_REPRESENTATION_ITEM()
RATIONAL_B_SPLINE_CURVE((1.00589416567691,1.00611162505669,1.00589416567691))
REPRESENTATION_ITEM('')
);
#210=(
BOUNDED_CURVE()
B_SPLINE_CURVE(2,(#62235,#62236,#62237),.UNSPECIFIED.,.F.,.F.)
B_SPLINE_CURVE_WITH_KNOTS((3,3),(0.196145060700811,2.27801504598277),
 .UNSPECIFIED.)
CURVE()
GEOMETRIC_REPRESENTATION_ITEM()
RATIONAL_B_SPLINE_CURVE((1.02999692649796,1.17548252555731,1.02999692649702))
REPRESENTATION_ITEM('')
);
#211=(
BOUNDED_CURVE()
B_SPLINE_CURVE(2,(#62239,#62240,#62241),.UNSPECIFIED.,.F.,.F.)
B_SPLINE_CURVE_WITH_KNOTS((3,3),(0.280206015619887,0.367357794870763),
 .UNSPECIFIED.)
CURVE()
GEOMETRIC_REPRESENTATION_ITEM()
RATIONAL_B_SPLINE_CURVE((1.00589416567691,1.00611162505669,1.00589416567691))
REPRESENTATION_ITEM('')
);
#212=(
BOUNDED_CURVE()
B_SPLINE_CURVE(2,(#62243,#62244,#62245),.UNSPECIFIED.,.F.,.F.)
B_SPLINE_CURVE_WITH_KNOTS((3,3),(0.196145060700811,2.27801504598277),
 .UNSPECIFIED.)
CURVE()
GEOMETRIC_REPRESENTATION_ITEM()
RATIONAL_B_SPLINE_CURVE((1.02999692649796,1.1754825255573,1.02999692649702))
REPRESENTATION_ITEM('')
);
#213=(
BOUNDED_CURVE()
B_SPLINE_CURVE(2,(#62247,#62248,#62249),.UNSPECIFIED.,.F.,.F.)
B_SPLINE_CURVE_WITH_KNOTS((3,3),(0.280206015619889,0.367357794870765),
 .UNSPECIFIED.)
CURVE()
GEOMETRIC_REPRESENTATION_ITEM()
RATIONAL_B_SPLINE_CURVE((1.00589416567691,1.00611162505669,1.00589416567691))
REPRESENTATION_ITEM('')
);
#214=(
BOUNDED_CURVE()
B_SPLINE_CURVE(2,(#62251,#62252,#62253),.UNSPECIFIED.,.F.,.F.)
B_SPLINE_CURVE_WITH_KNOTS((3,3),(0.196145060700811,2.27801504598277),
 .UNSPECIFIED.)
CURVE()
GEOMETRIC_REPRESENTATION_ITEM()
RATIONAL_B_SPLINE_CURVE((1.02999692649796,1.17548252555731,1.02999692649702))
REPRESENTATION_ITEM('')
);
#215=(
BOUNDED_CURVE()
B_SPLINE_CURVE(2,(#62254,#62255,#62256),.UNSPECIFIED.,.F.,.F.)
B_SPLINE_CURVE_WITH_KNOTS((3,3),(0.280206015619893,0.367357794870768),
 .UNSPECIFIED.)
CURVE()
GEOMETRIC_REPRESENTATION_ITEM()
RATIONAL_B_SPLINE_CURVE((1.00589416567691,1.00611162505669,1.00589416567691))
REPRESENTATION_ITEM('')
);
#216=(
BOUNDED_CURVE()
B_SPLINE_CURVE(2,(#62257,#62258,#62259),.UNSPECIFIED.,.F.,.F.)
B_SPLINE_CURVE_WITH_KNOTS((3,3),(1.23708005334447,2.27801504598277),
 .UNSPECIFIED.)
CURVE()
GEOMETRIC_REPRESENTATION_ITEM()
RATIONAL_B_SPLINE_CURVE((1.1027397260274,1.10273972602697,1.02999692649702))
REPRESENTATION_ITEM('')
);
#217=(
BOUNDED_CURVE()
B_SPLINE_CURVE(2,(#62263,#62264,#62265),.UNSPECIFIED.,.F.,.F.)
B_SPLINE_CURVE_WITH_KNOTS((3,3),(0.0551833308085754,0.208603356030846),
 .UNSPECIFIED.)
CURVE()
GEOMETRIC_REPRESENTATION_ITEM()
RATIONAL_B_SPLINE_CURVE((1.00066796366419,1.00140515246646,1.00107839993824))
REPRESENTATION_ITEM('')
);
#218=(
BOUNDED_CURVE()
B_SPLINE_CURVE(2,(#62269,#62270,#62271),.UNSPECIFIED.,.F.,.F.)
B_SPLINE_CURVE_WITH_KNOTS((3,3),(0.,0.0415381994417462),.UNSPECIFIED.)
CURVE()
GEOMETRIC_REPRESENTATION_ITEM()
RATIONAL_B_SPLINE_CURVE((1.,1.,1.))
REPRESENTATION_ITEM('')
);
#219=(
BOUNDED_CURVE()
B_SPLINE_CURVE(2,(#62283,#62284,#62285),.UNSPECIFIED.,.F.,.F.)
B_SPLINE_CURVE_WITH_KNOTS((3,3),(0.146737168364576,0.166814895714678),
 .UNSPECIFIED.)
CURVE()
GEOMETRIC_REPRESENTATION_ITEM()
RATIONAL_B_SPLINE_CURVE((1.00169850872058,1.00172953563951,1.001737254019))
REPRESENTATION_ITEM('')
);
#220=(
BOUNDED_CURVE()
B_SPLINE_CURVE(2,(#62287,#62288,#62289),.UNSPECIFIED.,.F.,.F.)
B_SPLINE_CURVE_WITH_KNOTS((3,3),(0.0286170700108412,0.076212379983174),
 .UNSPECIFIED.)
CURVE()
GEOMETRIC_REPRESENTATION_ITEM()
RATIONAL_B_SPLINE_CURVE((1.00112886559711,1.00201824869615,1.0027434105643))
REPRESENTATION_ITEM('')
);
#221=(
BOUNDED_CURVE()
B_SPLINE_CURVE(2,(#62291,#62292,#62293),.UNSPECIFIED.,.F.,.F.)
B_SPLINE_CURVE_WITH_KNOTS((3,3),(0.460004626021661,2.01415548066414),
 .UNSPECIFIED.)
CURVE()
GEOMETRIC_REPRESENTATION_ITEM()
RATIONAL_B_SPLINE_CURVE((1.06220108868579,1.14327836336948,1.06220108868485))
REPRESENTATION_ITEM('')
);
#222=(
BOUNDED_CURVE()
B_SPLINE_CURVE(2,(#62295,#62296,#62297),.UNSPECIFIED.,.F.,.F.)
B_SPLINE_CURVE_WITH_KNOTS((3,3),(0.517898922485178,0.565329042615561),
 .UNSPECIFIED.)
CURVE()
GEOMETRIC_REPRESENTATION_ITEM()
RATIONAL_B_SPLINE_CURVE((1.00287035745075,1.00210549051842,1.00117645345012))
REPRESENTATION_ITEM('')
);
#223=(
BOUNDED_CURVE()
B_SPLINE_CURVE(2,(#62299,#62300,#62301),.UNSPECIFIED.,.F.,.F.)
B_SPLINE_CURVE_WITH_KNOTS((3,3),(0.180111955289092,0.200189682639419),
 .UNSPECIFIED.)
CURVE()
GEOMETRIC_REPRESENTATION_ITEM()
RATIONAL_B_SPLINE_CURVE((1.00173725404747,1.00172953566789,1.0016985087485))
REPRESENTATION_ITEM('')
);
#224=(
BOUNDED_CURVE()
B_SPLINE_CURVE(2,(#62302,#62303,#62304),.UNSPECIFIED.,.F.,.F.)
B_SPLINE_CURVE_WITH_KNOTS((3,3),(0.13571848159483,0.289180967053278),
 .UNSPECIFIED.)
CURVE()
GEOMETRIC_REPRESENTATION_ITEM()
RATIONAL_B_SPLINE_CURVE((1.00140882605982,1.00173471838467,1.00099631962981))
REPRESENTATION_ITEM('')
);
#225=(
BOUNDED_CURVE()
B_SPLINE_CURVE(2,(#62309,#62310,#62311),.UNSPECIFIED.,.F.,.F.)
B_SPLINE_CURVE_WITH_KNOTS((3,3),(-2.1703979840528,-2.16974314947153),
 .UNSPECIFIED.)
CURVE()
GEOMETRIC_REPRESENTATION_ITEM()
RATIONAL_B_SPLINE_CURVE((1.2052492603669,1.20540347259793,1.20555757308984))
REPRESENTATION_ITEM('')
);
#226=(
BOUNDED_CURVE()
B_SPLINE_CURVE(2,(#62366,#62367,#62368),.UNSPECIFIED.,.F.,.F.)
B_SPLINE_CURVE_WITH_KNOTS((3,3),(-0.363565876377545,-0.362911041796268),
 .UNSPECIFIED.)
CURVE()
GEOMETRIC_REPRESENTATION_ITEM()
RATIONAL_B_SPLINE_CURVE((1.20555757308984,1.20540347259793,1.2052492603669))
REPRESENTATION_ITEM('')
);
#227=(
BOUNDED_CURVE()
B_SPLINE_CURVE(2,(#62388,#62389,#62390),.UNSPECIFIED.,.F.,.F.)
B_SPLINE_CURVE_WITH_KNOTS((3,3),(0.0400329798994461,0.0815711793412183),
 .UNSPECIFIED.)
CURVE()
GEOMETRIC_REPRESENTATION_ITEM()
RATIONAL_B_SPLINE_CURVE((1.,1.,1.))
REPRESENTATION_ITEM('')
);
#228=(
BOUNDED_CURVE()
B_SPLINE_CURVE(2,(#62421,#62422,#62423),.UNSPECIFIED.,.F.,.F.)
B_SPLINE_CURVE_WITH_KNOTS((3,3),(0.496551500635133,0.54414681060686),
 .UNSPECIFIED.)
CURVE()
GEOMETRIC_REPRESENTATION_ITEM()
RATIONAL_B_SPLINE_CURVE((1.00274341056425,1.00201824869611,1.00112886559708))
REPRESENTATION_ITEM('')
);
#229=(
BOUNDED_CURVE()
B_SPLINE_CURVE(2,(#62426,#62427,#62428),.UNSPECIFIED.,.F.,.F.)
B_SPLINE_CURVE_WITH_KNOTS((3,3),(0.180111955327547,0.200189682676742),
 .UNSPECIFIED.)
CURVE()
GEOMETRIC_REPRESENTATION_ITEM()
RATIONAL_B_SPLINE_CURVE((1.00173725401411,1.00172953563463,1.00169850871579))
REPRESENTATION_ITEM('')
);
#230=(
BOUNDED_CURVE()
B_SPLINE_CURVE(2,(#62430,#62431,#62432),.UNSPECIFIED.,.F.,.F.)
B_SPLINE_CURVE_WITH_KNOTS((3,3),(0.135718481594802,0.28918096705326),
 .UNSPECIFIED.)
CURVE()
GEOMETRIC_REPRESENTATION_ITEM()
RATIONAL_B_SPLINE_CURVE((1.00140882605999,1.00173471838487,1.00099631962993))
REPRESENTATION_ITEM('')
);
#231=(
BOUNDED_CURVE()
B_SPLINE_CURVE(2,(#62436,#62437,#62438),.UNSPECIFIED.,.F.,.F.)
B_SPLINE_CURVE_WITH_KNOTS((3,3),(0.0762382668082746,0.229700752266092),
 .UNSPECIFIED.)
CURVE()
GEOMETRIC_REPRESENTATION_ITEM()
RATIONAL_B_SPLINE_CURVE((1.00099631962987,1.00173471838476,1.0014088260599))
REPRESENTATION_ITEM('')
);
#232=(
BOUNDED_CURVE()
B_SPLINE_CURVE(2,(#62440,#62441,#62442),.UNSPECIFIED.,.F.,.F.)
B_SPLINE_CURVE_WITH_KNOTS((3,3),(0.146737168364582,0.166814895714678),
 .UNSPECIFIED.)
CURVE()
GEOMETRIC_REPRESENTATION_ITEM()
RATIONAL_B_SPLINE_CURVE((1.00169850872035,1.00172953563927,1.00173725401877))
REPRESENTATION_ITEM('')
);
#233=(
BOUNDED_CURVE()
B_SPLINE_CURVE(2,(#62443,#62444,#62445),.UNSPECIFIED.,.F.,.F.)
B_SPLINE_CURVE_WITH_KNOTS((3,3),(0.0285159432695787,0.075946063400608),
 .UNSPECIFIED.)
CURVE()
GEOMETRIC_REPRESENTATION_ITEM()
RATIONAL_B_SPLINE_CURVE((1.00117645345009,1.00210549051841,1.00287035745075))
REPRESENTATION_ITEM('')
);
#234=(
BOUNDED_CURVE()
B_SPLINE_CURVE(2,(#62450,#62451,#62452),.UNSPECIFIED.,.F.,.F.)
B_SPLINE_CURVE_WITH_KNOTS((3,3),(-0.363565876377541,-0.362911041796264),
 .UNSPECIFIED.)
CURVE()
GEOMETRIC_REPRESENTATION_ITEM()
RATIONAL_B_SPLINE_CURVE((1.20555757308984,1.20540347259794,1.2052492603669))
REPRESENTATION_ITEM('')
);
#235=(
BOUNDED_CURVE()
B_SPLINE_CURVE(2,(#62464,#62465,#62466),.UNSPECIFIED.,.F.,.F.)
B_SPLINE_CURVE_WITH_KNOTS((3,3),(0.460004626021663,2.01415548066414),
 .UNSPECIFIED.)
CURVE()
GEOMETRIC_REPRESENTATION_ITEM()
RATIONAL_B_SPLINE_CURVE((1.06220108868579,1.14327836336948,1.06220108868485))
REPRESENTATION_ITEM('')
);
#236=(
BOUNDED_CURVE()
B_SPLINE_CURVE(2,(#62480,#62481,#62482),.UNSPECIFIED.,.F.,.F.)
B_SPLINE_CURVE_WITH_KNOTS((3,3),(0.496551500635129,0.544146810606855),
 .UNSPECIFIED.)
CURVE()
GEOMETRIC_REPRESENTATION_ITEM()
RATIONAL_B_SPLINE_CURVE((1.00274341056426,1.00201824869612,1.00112886559708))
REPRESENTATION_ITEM('')
);
#237=(
BOUNDED_CURVE()
B_SPLINE_CURVE(2,(#62488,#62489,#62490),.UNSPECIFIED.,.F.,.F.)
B_SPLINE_CURVE_WITH_KNOTS((3,3),(-0.363565876377545,-0.362911041796268),
 .UNSPECIFIED.)
CURVE()
GEOMETRIC_REPRESENTATION_ITEM()
RATIONAL_B_SPLINE_CURVE((1.20555757308984,1.20540347259793,1.2052492603669))
REPRESENTATION_ITEM('')
);
#238=(
BOUNDED_CURVE()
B_SPLINE_CURVE(2,(#62495,#62496,#62497),.UNSPECIFIED.,.F.,.F.)
B_SPLINE_CURVE_WITH_KNOTS((3,3),(0.180111955326739,0.200189682676032),
 .UNSPECIFIED.)
CURVE()
GEOMETRIC_REPRESENTATION_ITEM()
RATIONAL_B_SPLINE_CURVE((1.00173725401877,1.00172953563927,1.00169850872035))
REPRESENTATION_ITEM('')
);
#239=(
BOUNDED_CURVE()
B_SPLINE_CURVE(2,(#62506,#62507,#62508),.UNSPECIFIED.,.F.,.F.)
B_SPLINE_CURVE_WITH_KNOTS((3,3),(-2.1703979840528,-2.16974314947152),
 .UNSPECIFIED.)
CURVE()
GEOMETRIC_REPRESENTATION_ITEM()
RATIONAL_B_SPLINE_CURVE((1.2052492603669,1.20540347259793,1.20555757308983))
REPRESENTATION_ITEM('')
);
#240=(
BOUNDED_CURVE()
B_SPLINE_CURVE(2,(#62514,#62515,#62516),.UNSPECIFIED.,.F.,.F.)
B_SPLINE_CURVE_WITH_KNOTS((3,3),(0.,0.0415381989501033),.UNSPECIFIED.)
CURVE()
GEOMETRIC_REPRESENTATION_ITEM()
RATIONAL_B_SPLINE_CURVE((1.,1.,1.))
REPRESENTATION_ITEM('')
);
#241=(
BOUNDED_CURVE()
B_SPLINE_CURVE(2,(#62522,#62523,#62524),.UNSPECIFIED.,.F.,.F.)
B_SPLINE_CURVE_WITH_KNOTS((3,3),(2.58081477858363,2.59739059715085),
 .UNSPECIFIED.)
CURVE()
GEOMETRIC_REPRESENTATION_ITEM()
RATIONAL_B_SPLINE_CURVE((1.03637289268669,1.01830325256961,1.))
REPRESENTATION_ITEM('')
);
#242=(
BOUNDED_CURVE()
B_SPLINE_CURVE(2,(#62527,#62528,#62529),.UNSPECIFIED.,.F.,.F.)
B_SPLINE_CURVE_WITH_KNOTS((3,3),(1.77226571272999,1.80534191248319),
 .UNSPECIFIED.)
CURVE()
GEOMETRIC_REPRESENTATION_ITEM()
RATIONAL_B_SPLINE_CURVE((1.0219180827151,1.01662663545196,1.01113004279036))
REPRESENTATION_ITEM('')
);
#243=(
BOUNDED_CURVE()
B_SPLINE_CURVE(2,(#62587,#62588,#62589),.UNSPECIFIED.,.F.,.F.)
B_SPLINE_CURVE_WITH_KNOTS((3,3),(0.0468703348388751,0.0935146604975977),
 .UNSPECIFIED.)
CURVE()
GEOMETRIC_REPRESENTATION_ITEM()
RATIONAL_B_SPLINE_CURVE((1.00023109890562,1.00023054172511,1.))
REPRESENTATION_ITEM('')
);
#244=(
BOUNDED_CURVE()
B_SPLINE_CURVE(2,(#62597,#62598,#62599),.UNSPECIFIED.,.F.,.F.)
B_SPLINE_CURVE_WITH_KNOTS((3,3),(-2.1703979840528,-2.16974314947153),
 .UNSPECIFIED.)
CURVE()
GEOMETRIC_REPRESENTATION_ITEM()
RATIONAL_B_SPLINE_CURVE((1.2052492603669,1.20540347259793,1.20555757308984))
REPRESENTATION_ITEM('')
);
#245=(
BOUNDED_CURVE()
B_SPLINE_CURVE(2,(#62605,#62606,#62607),.UNSPECIFIED.,.F.,.F.)
B_SPLINE_CURVE_WITH_KNOTS((3,3),(-0.363565876377547,-0.36291104179627),
 .UNSPECIFIED.)
CURVE()
GEOMETRIC_REPRESENTATION_ITEM()
RATIONAL_B_SPLINE_CURVE((1.20555757308984,1.20540347259793,1.2052492603669))
REPRESENTATION_ITEM('')
);
#246=(
BOUNDED_CURVE()
B_SPLINE_CURVE(2,(#62618,#62619,#62620),.UNSPECIFIED.,.F.,.F.)
B_SPLINE_CURVE_WITH_KNOTS((3,3),(-2.17039798405279,-2.16974314947152),
 .UNSPECIFIED.)
CURVE()
GEOMETRIC_REPRESENTATION_ITEM()
RATIONAL_B_SPLINE_CURVE((1.20524926036689,1.20540347259792,1.20555757308983))
REPRESENTATION_ITEM('')
);
#247=(
BOUNDED_CURVE()
B_SPLINE_CURVE(2,(#62660,#62661,#62662),.UNSPECIFIED.,.F.,.F.)
B_SPLINE_CURVE_WITH_KNOTS((3,3),(2.58081477858368,2.5973905971509),
 .UNSPECIFIED.)
CURVE()
GEOMETRIC_REPRESENTATION_ITEM()
RATIONAL_B_SPLINE_CURVE((1.03637289268669,1.01830325256961,1.))
REPRESENTATION_ITEM('')
);
#248=(
BOUNDED_CURVE()
B_SPLINE_CURVE(2,(#62667,#62668,#62669),.UNSPECIFIED.,.F.,.F.)
B_SPLINE_CURVE_WITH_KNOTS((3,3),(0.0764015610922613,0.230183975191949),
 .UNSPECIFIED.)
CURVE()
GEOMETRIC_REPRESENTATION_ITEM()
RATIONAL_B_SPLINE_CURVE((1.00095841961808,1.00165861973304,1.001294595355))
REPRESENTATION_ITEM('')
);
#249=(
BOUNDED_CURVE()
B_SPLINE_CURVE(2,(#62675,#62676,#62677),.UNSPECIFIED.,.F.,.F.)
B_SPLINE_CURVE_WITH_KNOTS((3,3),(0.0286170700108397,0.0762123799831708),
 .UNSPECIFIED.)
CURVE()
GEOMETRIC_REPRESENTATION_ITEM()
RATIONAL_B_SPLINE_CURVE((1.00112886559711,1.00201824869616,1.00274341056431))
REPRESENTATION_ITEM('')
);
#250=(
BOUNDED_CURVE()
B_SPLINE_CURVE(2,(#62683,#62684,#62685),.UNSPECIFIED.,.F.,.F.)
B_SPLINE_CURVE_WITH_KNOTS((3,3),(0.460004626021665,2.01415548066414),
 .UNSPECIFIED.)
CURVE()
GEOMETRIC_REPRESENTATION_ITEM()
RATIONAL_B_SPLINE_CURVE((1.06220108868579,1.14327836336947,1.06220108868485))
REPRESENTATION_ITEM('')
);
#251=(
BOUNDED_CURVE()
B_SPLINE_CURVE(2,(#62687,#62688,#62689),.UNSPECIFIED.,.F.,.F.)
B_SPLINE_CURVE_WITH_KNOTS((3,3),(0.517898922485166,0.565329042615548),
 .UNSPECIFIED.)
CURVE()
GEOMETRIC_REPRESENTATION_ITEM()
RATIONAL_B_SPLINE_CURVE((1.00287035745074,1.00210549051841,1.00117645345011))
REPRESENTATION_ITEM('')
);
#252=(
BOUNDED_CURVE()
B_SPLINE_CURVE(2,(#62691,#62692,#62693),.UNSPECIFIED.,.F.,.F.)
B_SPLINE_CURVE_WITH_KNOTS((3,3),(0.180111955322879,0.20018968267217),
 .UNSPECIFIED.)
CURVE()
GEOMETRIC_REPRESENTATION_ITEM()
RATIONAL_B_SPLINE_CURVE((1.00173725401601,1.00172953563653,1.00169850871767))
REPRESENTATION_ITEM('')
);
#253=(
BOUNDED_CURVE()
B_SPLINE_CURVE(2,(#62695,#62696,#62697),.UNSPECIFIED.,.F.,.F.)
B_SPLINE_CURVE_WITH_KNOTS((3,3),(0.12497957891104,0.278761993011364),
 .UNSPECIFIED.)
CURVE()
GEOMETRIC_REPRESENTATION_ITEM()
RATIONAL_B_SPLINE_CURVE((1.00129459535509,1.00165861973317,1.00095841961815))
REPRESENTATION_ITEM('')
);
#254=(
BOUNDED_CURVE()
B_SPLINE_CURVE(2,(#62699,#62700,#62701),.UNSPECIFIED.,.F.,.F.)
B_SPLINE_CURVE_WITH_KNOTS((3,3),(0.146737168401206,0.166814895752325),
 .UNSPECIFIED.)
CURVE()
GEOMETRIC_REPRESENTATION_ITEM()
RATIONAL_B_SPLINE_CURVE((1.00169850874789,1.00172953566728,1.00173725404685))
REPRESENTATION_ITEM('')
);
#255=(
BOUNDED_CURVE()
B_SPLINE_CURVE(2,(#62711,#62712,#62713),.UNSPECIFIED.,.F.,.F.)
B_SPLINE_CURVE_WITH_KNOTS((3,3),(2.58081477858364,2.59739059715087),
 .UNSPECIFIED.)
CURVE()
GEOMETRIC_REPRESENTATION_ITEM()
RATIONAL_B_SPLINE_CURVE((1.03637289268669,1.01830325256961,1.))
REPRESENTATION_ITEM('')
);
#256=(
BOUNDED_CURVE()
B_SPLINE_CURVE(2,(#62717,#62718,#62719),.UNSPECIFIED.,.F.,.F.)
B_SPLINE_CURVE_WITH_KNOTS((3,3),(0.,0.0165758185672203),.UNSPECIFIED.)
CURVE()
GEOMETRIC_REPRESENTATION_ITEM()
RATIONAL_B_SPLINE_CURVE((1.,1.01830325256961,1.03637289268669))
REPRESENTATION_ITEM('')
);
#257=(
BOUNDED_CURVE()
B_SPLINE_CURVE(2,(#62746,#62747,#62748),.UNSPECIFIED.,.F.,.F.)
B_SPLINE_CURVE_WITH_KNOTS((3,3),(-0.363565876377549,-0.362911041796272),
 .UNSPECIFIED.)
CURVE()
GEOMETRIC_REPRESENTATION_ITEM()
RATIONAL_B_SPLINE_CURVE((1.20555757308984,1.20540347259793,1.2052492603669))
REPRESENTATION_ITEM('')
);
#258=(
BOUNDED_CURVE()
B_SPLINE_CURVE(2,(#62751,#62752,#62753),.UNSPECIFIED.,.F.,.F.)
B_SPLINE_CURVE_WITH_KNOTS((3,3),(-2.17039798405279,-2.16974314947152),
 .UNSPECIFIED.)
CURVE()
GEOMETRIC_REPRESENTATION_ITEM()
RATIONAL_B_SPLINE_CURVE((1.20524926036689,1.20540347259792,1.20555757308982))
REPRESENTATION_ITEM('')
);
#259=(
BOUNDED_CURVE()
B_SPLINE_CURVE(2,(#62757,#62758,#62759),.UNSPECIFIED.,.F.,.F.)
B_SPLINE_CURVE_WITH_KNOTS((3,3),(0.0764015610913054,0.230183975191003),
 .UNSPECIFIED.)
CURVE()
GEOMETRIC_REPRESENTATION_ITEM()
RATIONAL_B_SPLINE_CURVE((1.00095841961842,1.00165861973365,1.00129459535547))
REPRESENTATION_ITEM('')
);
#260=(
BOUNDED_CURVE()
B_SPLINE_CURVE(2,(#62766,#62767,#62768),.UNSPECIFIED.,.F.,.F.)
B_SPLINE_CURVE_WITH_KNOTS((3,3),(0.1249795789111,0.278761993011415),
 .UNSPECIFIED.)
CURVE()
GEOMETRIC_REPRESENTATION_ITEM()
RATIONAL_B_SPLINE_CURVE((1.00129459535522,1.00165861973333,1.00095841961823))
REPRESENTATION_ITEM('')
);
#261=(
BOUNDED_CURVE()
B_SPLINE_CURVE(2,(#62781,#62782,#62783),.UNSPECIFIED.,.F.,.F.)
B_SPLINE_CURVE_WITH_KNOTS((3,3),(0.0285159432695794,0.0759460634006091),
 .UNSPECIFIED.)
CURVE()
GEOMETRIC_REPRESENTATION_ITEM()
RATIONAL_B_SPLINE_CURVE((1.00117645345008,1.00210549051839,1.00287035745073))
REPRESENTATION_ITEM('')
);
#262=(
BOUNDED_CURVE()
B_SPLINE_CURVE(2,(#62807,#62808,#62809),.UNSPECIFIED.,.F.,.F.)
B_SPLINE_CURVE_WITH_KNOTS((3,3),(0.146737168363879,0.166814895713834),
 .UNSPECIFIED.)
CURVE()
GEOMETRIC_REPRESENTATION_ITEM()
RATIONAL_B_SPLINE_CURVE((1.00169850871386,1.00172953563266,1.00173725401213))
REPRESENTATION_ITEM('')
);
#263=(
BOUNDED_CURVE()
B_SPLINE_CURVE(2,(#62887,#62888,#62889),.UNSPECIFIED.,.F.,.F.)
B_SPLINE_CURVE_WITH_KNOTS((3,3),(0.0543046845342199,0.0689123358693617),
 .UNSPECIFIED.)
CURVE()
GEOMETRIC_REPRESENTATION_ITEM()
RATIONAL_B_SPLINE_CURVE((1.00437382539668,1.00277520786002,1.00000007127116))
REPRESENTATION_ITEM('')
);
#264=(
BOUNDED_CURVE()
B_SPLINE_CURVE(2,(#62908,#62909,#62910),.UNSPECIFIED.,.F.,.F.)
B_SPLINE_CURVE_WITH_KNOTS((3,3),(1.87576610016924E-7,0.0146078389114927),
 .UNSPECIFIED.)
CURVE()
GEOMETRIC_REPRESENTATION_ITEM()
RATIONAL_B_SPLINE_CURVE((1.00000007127116,1.00277520785907,1.00437382539519))
REPRESENTATION_ITEM('')
);
#265=(
BOUNDED_CURVE()
B_SPLINE_CURVE(2,(#62927,#62928,#62929),.UNSPECIFIED.,.F.,.F.)
B_SPLINE_CURVE_WITH_KNOTS((3,3),(1.87576606599038E-7,0.0146078389114552),
 .UNSPECIFIED.)
CURVE()
GEOMETRIC_REPRESENTATION_ITEM()
RATIONAL_B_SPLINE_CURVE((1.00000007127116,1.00277520785998,1.00437382539664))
REPRESENTATION_ITEM('')
);
#266=(
BOUNDED_CURVE()
B_SPLINE_CURVE(2,(#62951,#62952,#62953),.UNSPECIFIED.,.F.,.F.)
B_SPLINE_CURVE_WITH_KNOTS((3,3),(0.0543046845342203,0.0689123358693609),
 .UNSPECIFIED.)
CURVE()
GEOMETRIC_REPRESENTATION_ITEM()
RATIONAL_B_SPLINE_CURVE((1.0043738253967,1.00277520786004,1.00000007127116))
REPRESENTATION_ITEM('')
);
#267=(
BOUNDED_CURVE()
B_SPLINE_CURVE(2,(#66650,#66651,#66652),.UNSPECIFIED.,.F.,.F.)
B_SPLINE_CURVE_WITH_KNOTS((3,3),(0.0318913416068047,0.0878632526191407),
 .UNSPECIFIED.)
CURVE()
GEOMETRIC_REPRESENTATION_ITEM()
RATIONAL_B_SPLINE_CURVE((1.,1.,1.))
REPRESENTATION_ITEM('')
);
#268=(
BOUNDED_CURVE()
B_SPLINE_CURVE(2,(#66656,#66657,#66658),.UNSPECIFIED.,.F.,.F.)
B_SPLINE_CURVE_WITH_KNOTS((3,3),(0.,0.0559719110123359),.UNSPECIFIED.)
CURVE()
GEOMETRIC_REPRESENTATION_ITEM()
RATIONAL_B_SPLINE_CURVE((1.,1.,1.))
REPRESENTATION_ITEM('')
);
#269=(
BOUNDED_CURVE()
B_SPLINE_CURVE(2,(#66674,#66675,#66676),.UNSPECIFIED.,.F.,.F.)
B_SPLINE_CURVE_WITH_KNOTS((3,3),(0.149824701143017,0.201007744174973),
 .UNSPECIFIED.)
CURVE()
GEOMETRIC_REPRESENTATION_ITEM()
RATIONAL_B_SPLINE_CURVE((1.0015789381359,1.00105916711486,1.))
REPRESENTATION_ITEM('')
);
#270=(
BOUNDED_CURVE()
B_SPLINE_CURVE(2,(#66679,#66680,#66681),.UNSPECIFIED.,.F.,.F.)
B_SPLINE_CURVE_WITH_KNOTS((3,3),(0.,0.0619069470426676),.UNSPECIFIED.)
CURVE()
GEOMETRIC_REPRESENTATION_ITEM()
RATIONAL_B_SPLINE_CURVE((1.,1.00126373727763,1.00175959622219))
REPRESENTATION_ITEM('')
);
#271=(
BOUNDED_CURVE()
B_SPLINE_CURVE(2,(#66690,#66691,#66692),.UNSPECIFIED.,.F.,.F.)
B_SPLINE_CURVE_WITH_KNOTS((3,3),(0.,0.0544904914367116),.UNSPECIFIED.)
CURVE()
GEOMETRIC_REPRESENTATION_ITEM()
RATIONAL_B_SPLINE_CURVE((1.,1.00018612804858,1.00011392668297))
REPRESENTATION_ITEM('')
);
#272=(
BOUNDED_CURVE()
B_SPLINE_CURVE(2,(#66696,#66697,#66698),.UNSPECIFIED.,.F.,.F.)
B_SPLINE_CURVE_WITH_KNOTS((3,3),(0.024031026287471,0.0785215177241609),
 .UNSPECIFIED.)
CURVE()
GEOMETRIC_REPRESENTATION_ITEM()
RATIONAL_B_SPLINE_CURVE((1.00011392668297,1.00018612804858,1.))
REPRESENTATION_ITEM('')
);
#273=(
BOUNDED_CURVE()
B_SPLINE_CURVE(2,(#66699,#66700,#66701),.UNSPECIFIED.,.F.,.F.)
B_SPLINE_CURVE_WITH_KNOTS((3,3),(0.,0.051183043031955),.UNSPECIFIED.)
CURVE()
GEOMETRIC_REPRESENTATION_ITEM()
RATIONAL_B_SPLINE_CURVE((1.,1.00105916711486,1.0015789381359))
REPRESENTATION_ITEM('')
);
#274=(
BOUNDED_CURVE()
B_SPLINE_CURVE(2,(#66711,#66712,#66713),.UNSPECIFIED.,.F.,.F.)
B_SPLINE_CURVE_WITH_KNOTS((3,3),(0.141860012781432,0.2037669598241),
 .UNSPECIFIED.)
CURVE()
GEOMETRIC_REPRESENTATION_ITEM()
RATIONAL_B_SPLINE_CURVE((1.00175959622219,1.00126373727763,1.))
REPRESENTATION_ITEM('')
);
#275=B_SPLINE_SURFACE_WITH_KNOTS('',3,3,((#53607,#53608,#53609,#53610,#53611,
#53612,#53613,#53614,#53615),(#53616,#53617,#53618,#53619,#53620,#53621,
#53622,#53623,#53624),(#53625,#53626,#53627,#53628,#53629,#53630,#53631,
#53632,#53633),(#53634,#53635,#53636,#53637,#53638,#53639,#53640,#53641,
#53642)),.UNSPECIFIED.,.F.,.F.,.F.,(4,4),(4,1,1,1,1,1,4),(0.,0.117317574699332),
(58.2563833255769,58.586820436873,59.2476946594652,59.5781317707613,60.2390059933534,
60.8998802159456,61.2303173272417),.UNSPECIFIED.);
#276=B_SPLINE_SURFACE_WITH_KNOTS('',3,3,((#53715,#53716,#53717,#53718,#53719,
#53720,#53721,#53722,#53723,#53724,#53725,#53726,#53727,#53728,#53729,#53730,
#53731,#53732,#53733,#53734,#53735,#53736,#53737,#53738,#53739,#53740,#53741,
#53742,#53743,#53744,#53745,#53746,#53747,#53748,#53749,#53750,#53751,#53752,
#53753,#53754,#53755,#53756,#53757,#53758,#53759,#53760,#53761),(#53762,
#53763,#53764,#53765,#53766,#53767,#53768,#53769,#53770,#53771,#53772,#53773,
#53774,#53775,#53776,#53777,#53778,#53779,#53780,#53781,#53782,#53783,#53784,
#53785,#53786,#53787,#53788,#53789,#53790,#53791,#53792,#53793,#53794,#53795,
#53796,#53797,#53798,#53799,#53800,#53801,#53802,#53803,#53804,#53805,#53806,
#53807,#53808),(#53809,#53810,#53811,#53812,#53813,#53814,#53815,#53816,
#53817,#53818,#53819,#53820,#53821,#53822,#53823,#53824,#53825,#53826,#53827,
#53828,#53829,#53830,#53831,#53832,#53833,#53834,#53835,#53836,#53837,#53838,
#53839,#53840,#53841,#53842,#53843,#53844,#53845,#53846,#53847,#53848,#53849,
#53850,#53851,#53852,#53853,#53854,#53855),(#53856,#53857,#53858,#53859,
#53860,#53861,#53862,#53863,#53864,#53865,#53866,#53867,#53868,#53869,#53870,
#53871,#53872,#53873,#53874,#53875,#53876,#53877,#53878,#53879,#53880,#53881,
#53882,#53883,#53884,#53885,#53886,#53887,#53888,#53889,#53890,#53891,#53892,
#53893,#53894,#53895,#53896,#53897,#53898,#53899,#53900,#53901,#53902)),
 .UNSPECIFIED.,.F.,.F.,.F.,(4,4),(4,1,1,1,1,1,1,1,1,1,1,1,1,1,1,1,1,1,1,
1,1,1,1,1,1,1,1,1,1,1,1,1,1,1,1,1,1,1,1,1,1,1,1,1,4),(0.,0.117317574699332),
(61.2845034392321,61.7747737335008,62.2650440277695,62.7553143220381,63.2455846163068,
63.7358549105755,64.2261252048442,64.7163954991129,65.2066657933815,65.6969360876502,
66.1872063819189,66.6774766761876,67.1677469704563,67.6580172647249,68.1482875589936,
68.6385578532623,69.128828147531,69.6190984417997,70.1093687360683,70.599639030337,
71.0899093246057,71.5801796188744,72.0704499131431,72.5607202074117,73.0509905016804,
73.5412607959491,74.0315310902178,74.5218013844865,75.0120716787551,75.5023419730238,
75.9926122672925,76.4828825615612,76.9731528558299,77.4634231500985,77.9536934443672,
78.4439637386359,78.9342340329046,79.4245043271733,79.9147746214419,80.4050449157106,
80.8953152099793,81.385585504248,81.8758557985167,82.3661260927854,82.856396387054),
 .UNSPECIFIED.);
#277=B_SPLINE_SURFACE_WITH_KNOTS('',3,3,((#54341,#54342,#54343,#54344,#54345,
#54346,#54347,#54348,#54349,#54350,#54351,#54352,#54353,#54354,#54355,#54356,
#54357,#54358,#54359,#54360,#54361,#54362,#54363,#54364,#54365,#54366,#54367,
#54368,#54369,#54370,#54371,#54372,#54373,#54374,#54375,#54376,#54377,#54378,
#54379,#54380,#54381,#54382,#54383,#54384,#54385,#54386,#54387,#54388,#54389,
#54390,#54391,#54392,#54393,#54394,#54395,#54396,#54397,#54398,#54399,#54400,
#54401,#54402,#54403,#54404,#54405,#54406,#54407,#54408,#54409,#54410,#54411,
#54412,#54413,#54414,#54415,#54416,#54417,#54418,#54419,#54420,#54421,#54422,
#54423,#54424,#54425),(#54426,#54427,#54428,#54429,#54430,#54431,#54432,
#54433,#54434,#54435,#54436,#54437,#54438,#54439,#54440,#54441,#54442,#54443,
#54444,#54445,#54446,#54447,#54448,#54449,#54450,#54451,#54452,#54453,#54454,
#54455,#54456,#54457,#54458,#54459,#54460,#54461,#54462,#54463,#54464,#54465,
#54466,#54467,#54468,#54469,#54470,#54471,#54472,#54473,#54474,#54475,#54476,
#54477,#54478,#54479,#54480,#54481,#54482,#54483,#54484,#54485,#54486,#54487,
#54488,#54489,#54490,#54491,#54492,#54493,#54494,#54495,#54496,#54497,#54498,
#54499,#54500,#54501,#54502,#54503,#54504,#54505,#54506,#54507,#54508,#54509,
#54510),(#54511,#54512,#54513,#54514,#54515,#54516,#54517,#54518,#54519,
#54520,#54521,#54522,#54523,#54524,#54525,#54526,#54527,#54528,#54529,#54530,
#54531,#54532,#54533,#54534,#54535,#54536,#54537,#54538,#54539,#54540,#54541,
#54542,#54543,#54544,#54545,#54546,#54547,#54548,#54549,#54550,#54551,#54552,
#54553,#54554,#54555,#54556,#54557,#54558,#54559,#54560,#54561,#54562,#54563,
#54564,#54565,#54566,#54567,#54568,#54569,#54570,#54571,#54572,#54573,#54574,
#54575,#54576,#54577,#54578,#54579,#54580,#54581,#54582,#54583,#54584,#54585,
#54586,#54587,#54588,#54589,#54590,#54591,#54592,#54593,#54594,#54595),
(#54596,#54597,#54598,#54599,#54600,#54601,#54602,#54603,#54604,#54605,
#54606,#54607,#54608,#54609,#54610,#54611,#54612,#54613,#54614,#54615,#54616,
#54617,#54618,#54619,#54620,#54621,#54622,#54623,#54624,#54625,#54626,#54627,
#54628,#54629,#54630,#54631,#54632,#54633,#54634,#54635,#54636,#54637,#54638,
#54639,#54640,#54641,#54642,#54643,#54644,#54645,#54646,#54647,#54648,#54649,
#54650,#54651,#54652,#54653,#54654,#54655,#54656,#54657,#54658,#54659,#54660,
#54661,#54662,#54663,#54664,#54665,#54666,#54667,#54668,#54669,#54670,#54671,
#54672,#54673,#54674,#54675,#54676,#54677,#54678,#54679,#54680)),
 .UNSPECIFIED.,.F.,.F.,.F.,(4,4),(4,1,1,1,1,1,1,1,1,1,1,1,1,1,1,1,1,1,1,
1,1,1,1,1,1,1,1,1,1,1,1,1,1,1,1,1,1,1,1,1,1,1,1,1,1,1,1,1,1,1,1,1,1,1,1,
1,1,1,1,1,1,1,1,1,1,1,1,1,1,1,1,1,1,1,1,1,1,1,1,1,1,1,4),(0.,0.117317574699332),
(8.304938233291,8.79653306474967,9.28812789620834,9.77972272766701,10.2713175591257,
10.7629123905843,11.254507222043,11.7461020535017,12.2376968849604,12.729291716419,
13.2208865478777,13.7124813793364,14.204076210795,14.6956710422537,15.1872658737124,
15.678860705171,16.1704555366297,16.6620503680884,17.153645199547,17.6452400310057,
18.1368348624644,18.628429693923,19.1200245253817,19.6116193568404,20.103214188299,
20.5948090197577,21.0864038512164,21.5779986826751,22.0695935141337,22.5611883455924,
23.0527831770511,23.5443780085097,24.0359728399684,24.5275676714271,25.0191625028857,
25.5107573343444,26.0023521658031,26.4939469972617,26.9855418287204,27.4771366601791,
27.9687314916377,28.4603263230964,28.9519211545551,29.4435159860138,29.9351108174724,
30.4267056489311,30.9183004803898,31.4098953118484,31.9014901433071,32.3930849747658,
32.8846798062244,33.3762746376831,33.8678694691418,34.3594643006004,34.8510591320591,
35.3426539635178,35.8342487949764,36.3258436264351,36.8174384578938,37.3090332893524,
37.8006281208111,38.2922229522698,38.7838177837285,39.2754126151871,39.7670074466458,
40.2586022781045,40.7501971095631,41.2417919410218,41.7333867724805,42.2249816039391,
42.7165764353978,43.2081712668565,43.6997660983151,44.1913609297738,44.6829557612325,
45.1745505926911,45.6661454241498,46.1577402556085,46.6493350870672,47.1409299185258,
47.6325247499845,48.1241195814432,48.6157144129018),.UNSPECIFIED.);
#278=B_SPLINE_SURFACE_WITH_KNOTS('',3,3,((#55387,#55388,#55389,#55390,#55391,
#55392,#55393,#55394,#55395),(#55396,#55397,#55398,#55399,#55400,#55401,
#55402,#55403,#55404),(#55405,#55406,#55407,#55408,#55409,#55410,#55411,
#55412,#55413),(#55414,#55415,#55416,#55417,#55418,#55419,#55420,#55421,
#55422)),.UNSPECIFIED.,.F.,.F.,.F.,(4,4),(4,1,1,1,1,1,4),(0.,0.117317574699332),
(48.7821842940486,49.4244050727166,49.7455154620506,50.0666258513846,50.7088466300525,
51.0299570193865,51.6721777980545),.UNSPECIFIED.);
#279=B_SPLINE_SURFACE_WITH_KNOTS('',3,3,((#55476,#55477,#55478,#55479,#55480,
#55481,#55482,#55483,#55484),(#55485,#55486,#55487,#55488,#55489,#55490,
#55491,#55492,#55493),(#55494,#55495,#55496,#55497,#55498,#55499,#55500,
#55501,#55502),(#55503,#55504,#55505,#55506,#55507,#55508,#55509,#55510,
#55511)),.UNSPECIFIED.,.F.,.F.,.F.,(4,4),(4,1,1,1,1,1,4),(0.,0.117317574699332),
(52.0050602882015,52.6272969542447,52.9384152872664,53.249533620288,53.8717702863312,
54.4940069523745,54.8051252853961),.UNSPECIFIED.);
#280=B_SPLINE_SURFACE_WITH_KNOTS('',3,3,((#55573,#55574,#55575,#55576,#55577,
#55578,#55579,#55580,#55581),(#55582,#55583,#55584,#55585,#55586,#55587,
#55588,#55589,#55590),(#55591,#55592,#55593,#55594,#55595,#55596,#55597,
#55598,#55599),(#55600,#55601,#55602,#55603,#55604,#55605,#55606,#55607,
#55608)),.UNSPECIFIED.,.F.,.F.,.F.,(4,4),(4,1,1,1,1,1,4),(0.,0.117317574699332),
(55.1490525302778,55.4633418551201,56.0919205048047,56.7204991544894,57.0347884793317,
57.349077804174,57.9776564538586),.UNSPECIFIED.);
#281=B_SPLINE_SURFACE_WITH_KNOTS('',3,3,((#55670,#55671,#55672,#55673,#55674,
#55675,#55676,#55677,#55678,#55679,#55680,#55681,#55682,#55683,#55684,#55685,
#55686,#55687,#55688,#55689,#55690,#55691,#55692,#55693,#55694,#55695,#55696,
#55697,#55698,#55699,#55700,#55701,#55702,#55703,#55704,#55705,#55706,#55707,
#55708,#55709,#55710,#55711,#55712,#55713,#55714,#55715,#55716),(#55717,
#55718,#55719,#55720,#55721,#55722,#55723,#55724,#55725,#55726,#55727,#55728,
#55729,#55730,#55731,#55732,#55733,#55734,#55735,#55736,#55737,#55738,#55739,
#55740,#55741,#55742,#55743,#55744,#55745,#55746,#55747,#55748,#55749,#55750,
#55751,#55752,#55753,#55754,#55755,#55756,#55757,#55758,#55759,#55760,#55761,
#55762,#55763),(#55764,#55765,#55766,#55767,#55768,#55769,#55770,#55771,
#55772,#55773,#55774,#55775,#55776,#55777,#55778,#55779,#55780,#55781,#55782,
#55783,#55784,#55785,#55786,#55787,#55788,#55789,#55790,#55791,#55792,#55793,
#55794,#55795,#55796,#55797,#55798,#55799,#55800,#55801,#55802,#55803,#55804,
#55805,#55806,#55807,#55808,#55809,#55810),(#55811,#55812,#55813,#55814,
#55815,#55816,#55817,#55818,#55819,#55820,#55821,#55822,#55823,#55824,#55825,
#55826,#55827,#55828,#55829,#55830,#55831,#55832,#55833,#55834,#55835,#55836,
#55837,#55838,#55839,#55840,#55841,#55842,#55843,#55844,#55845,#55846,#55847,
#55848,#55849,#55850,#55851,#55852,#55853,#55854,#55855,#55856,#55857)),
 .UNSPECIFIED.,.F.,.F.,.F.,(4,4),(4,1,1,1,1,1,1,1,1,1,1,1,1,1,1,1,1,1,1,
1,1,1,1,1,1,1,1,1,1,1,1,1,1,1,1,1,1,1,1,1,1,1,1,1,4),(0.,0.117317574699332),
(64.4256593907634,64.920671977511,65.4156845642586,65.9106971510062,66.4057097377538,
66.9007223245014,67.3957349112491,67.8907474979967,68.3857600847443,68.8807726714919,
69.3757852582395,69.8707978449871,70.3658104317347,70.8608230184823,71.3558356052299,
71.8508481919775,72.3458607787251,72.8408733654727,73.3358859522203,73.8308985389679,
74.3259111257155,74.8209237124631,75.3159362992107,75.8109488859583,76.3059614727059,
76.8009740594535,77.2959866462011,77.7909992329487,78.2860118196963,78.7810244064439,
79.2760369931915,79.7710495799391,80.2660621666867,80.7610747534343,81.2560873401819,
81.7510999269296,82.2461125136772,82.7411251004248,83.2361376871724,83.73115027392,
84.2261628606676,84.7211754474152,85.2161880341628,85.7112006209104,86.206213207658),
 .UNSPECIFIED.);
#282=B_SPLINE_SURFACE_WITH_KNOTS('',3,3,((#56291,#56292,#56293,#56294,#56295,
#56296,#56297,#56298,#56299),(#56300,#56301,#56302,#56303,#56304,#56305,
#56306,#56307,#56308),(#56309,#56310,#56311,#56312,#56313,#56314,#56315,
#56316,#56317),(#56318,#56319,#56320,#56321,#56322,#56323,#56324,#56325,
#56326)),.UNSPECIFIED.,.F.,.F.,.F.,(4,4),(4,1,1,1,1,1,4),(0.,0.117317574699332),
(61.413786866147,61.742287519182,62.399288825252,62.727789478287,63.384790784357,
64.041792090427,64.370292743462),.UNSPECIFIED.);
#283=B_SPLINE_SURFACE_WITH_KNOTS('',3,3,((#56383,#56384,#56385,#56386,#56387,
#56388,#56389,#56390,#56391),(#56392,#56393,#56394,#56395,#56396,#56397,
#56398,#56399,#56400),(#56401,#56402,#56403,#56404,#56405,#56406,#56407,
#56408,#56409),(#56410,#56411,#56412,#56413,#56414,#56415,#56416,#56417,
#56418)),.UNSPECIFIED.,.F.,.F.,.F.,(4,4),(4,1,1,1,1,1,4),(0.,0.117317574699332),
(58.294224706896,58.9183499948197,59.2304126387815,59.5424752827434,60.166600570667,
60.7907258585907,61.1027885025526),.UNSPECIFIED.);
#284=B_SPLINE_SURFACE_WITH_KNOTS('',3,3,((#56480,#56481,#56482,#56483,#56484,
#56485,#56486,#56487,#56488,#56489,#56490,#56491,#56492,#56493,#56494,#56495,
#56496,#56497,#56498,#56499,#56500,#56501,#56502,#56503,#56504,#56505,#56506,
#56507,#56508,#56509,#56510,#56511,#56512,#56513,#56514,#56515,#56516,#56517,
#56518,#56519,#56520,#56521,#56522,#56523,#56524,#56525,#56526,#56527,#56528,
#56529,#56530,#56531,#56532,#56533,#56534,#56535,#56536,#56537,#56538,#56539,
#56540,#56541,#56542,#56543,#56544,#56545,#56546,#56547,#56548,#56549,#56550,
#56551,#56552,#56553,#56554,#56555,#56556,#56557,#56558,#56559,#56560,#56561,
#56562,#56563,#56564),(#56565,#56566,#56567,#56568,#56569,#56570,#56571,
#56572,#56573,#56574,#56575,#56576,#56577,#56578,#56579,#56580,#56581,#56582,
#56583,#56584,#56585,#56586,#56587,#56588,#56589,#56590,#56591,#56592,#56593,
#56594,#56595,#56596,#56597,#56598,#56599,#56600,#56601,#56602,#56603,#56604,
#56605,#56606,#56607,#56608,#56609,#56610,#56611,#56612,#56613,#56614,#56615,
#56616,#56617,#56618,#56619,#56620,#56621,#56622,#56623,#56624,#56625,#56626,
#56627,#56628,#56629,#56630,#56631,#56632,#56633,#56634,#56635,#56636,#56637,
#56638,#56639,#56640,#56641,#56642,#56643,#56644,#56645,#56646,#56647,#56648,
#56649),(#56650,#56651,#56652,#56653,#56654,#56655,#56656,#56657,#56658,
#56659,#56660,#56661,#56662,#56663,#56664,#56665,#56666,#56667,#56668,#56669,
#56670,#56671,#56672,#56673,#56674,#56675,#56676,#56677,#56678,#56679,#56680,
#56681,#56682,#56683,#56684,#56685,#56686,#56687,#56688,#56689,#56690,#56691,
#56692,#56693,#56694,#56695,#56696,#56697,#56698,#56699,#56700,#56701,#56702,
#56703,#56704,#56705,#56706,#56707,#56708,#56709,#56710,#56711,#56712,#56713,
#56714,#56715,#56716,#56717,#56718,#56719,#56720,#56721,#56722,#56723,#56724,
#56725,#56726,#56727,#56728,#56729,#56730,#56731,#56732,#56733,#56734),
(#56735,#56736,#56737,#56738,#56739,#56740,#56741,#56742,#56743,#56744,
#56745,#56746,#56747,#56748,#56749,#56750,#56751,#56752,#56753,#56754,#56755,
#56756,#56757,#56758,#56759,#56760,#56761,#56762,#56763,#56764,#56765,#56766,
#56767,#56768,#56769,#56770,#56771,#56772,#56773,#56774,#56775,#56776,#56777,
#56778,#56779,#56780,#56781,#56782,#56783,#56784,#56785,#56786,#56787,#56788,
#56789,#56790,#56791,#56792,#56793,#56794,#56795,#56796,#56797,#56798,#56799,
#56800,#56801,#56802,#56803,#56804,#56805,#56806,#56807,#56808,#56809,#56810,
#56811,#56812,#56813,#56814,#56815,#56816,#56817,#56818,#56819)),
 .UNSPECIFIED.,.F.,.F.,.F.,(4,4),(4,1,1,1,1,1,1,1,1,1,1,1,1,1,1,1,1,1,1,
1,1,1,1,1,1,1,1,1,1,1,1,1,1,1,1,1,1,1,1,1,1,1,1,1,1,1,1,1,1,1,1,1,1,1,1,
1,1,1,1,1,1,1,1,1,1,1,1,1,1,1,1,1,1,1,1,1,1,1,1,1,1,1,4),(0.,0.117317574699332),
(11.654755053895,12.1440162165507,12.6332773792065,13.1225385418623,13.611799704518,
14.1010608671738,14.5903220298296,15.0795831924853,15.5688443551411,16.0581055177969,
16.5473666804527,17.0366278431084,17.5258890057642,18.01515016842,18.5044113310757,
18.9936724937315,19.4829336563873,19.972194819043,20.4614559816988,20.9507171443546,
21.4399783070103,21.9292394696661,22.4185006323219,22.9077617949777,23.3970229576334,
23.8862841202892,24.375545282945,24.8648064456007,25.3540676082565,25.8433287709123,
26.332589933568,26.8218510962238,27.3111122588796,27.8003734215353,28.2896345841911,
28.7788957468469,29.2681569095027,29.7574180721584,30.2466792348142,30.73594039747,
31.2252015601257,31.7144627227815,32.2037238854373,32.692985048093,33.1822462107488,
33.6715073734046,34.1607685360603,34.6500296987161,35.1392908613719,35.6285520240277,
36.1178131866834,36.6070743493392,37.096335511995,37.5855966746507,38.0748578373065,
38.5641189999623,39.053380162618,39.5426413252738,40.0319024879296,40.5211636505854,
41.0104248132411,41.4996859758969,41.9889471385527,42.4782083012084,42.9674694638642,
43.45673062652,43.9459917891757,44.4352529518315,44.9245141144873,45.413775277143,
45.9030364397988,46.3922976024546,46.8815587651103,47.3708199277661,47.8600810904219,
48.3493422530777,48.8386034157334,49.3278645783892,49.817125741045,50.3063869037007,
50.7956480663565,51.2849092290123,51.774170391668),.UNSPECIFIED.);
#285=B_SPLINE_SURFACE_WITH_KNOTS('',3,3,((#57528,#57529,#57530,#57531,#57532,
#57533,#57534,#57535,#57536),(#57537,#57538,#57539,#57540,#57541,#57542,
#57543,#57544,#57545),(#57546,#57547,#57548,#57549,#57550,#57551,#57552,
#57553,#57554),(#57555,#57556,#57557,#57558,#57559,#57560,#57561,#57562,
#57563)),.UNSPECIFIED.,.F.,.F.,.F.,(4,4),(4,1,1,1,1,1,4),(0.,0.117317574699332),
(51.9058023205642,52.230691972308,52.8804712757956,53.2053609275394,53.855140231027,
54.1800298827708,54.8298091862584),.UNSPECIFIED.);
#286=B_SPLINE_SURFACE_WITH_KNOTS('',3,3,((#57698,#57699,#57700,#57701,#57702,
#57703,#57704,#57705,#57706),(#57707,#57708,#57709,#57710,#57711,#57712,
#57713,#57714,#57715),(#57716,#57717,#57718,#57719,#57720,#57721,#57722,
#57723,#57724),(#57725,#57726,#57727,#57728,#57729,#57730,#57731,#57732,
#57733)),.UNSPECIFIED.,.F.,.F.,.F.,(4,4),(4,1,1,1,1,1,4),(0.,0.117317574699332),
(55.1300987113493,55.4429246232081,56.0685764469255,56.3814023587843,57.0070541825018,
57.3198800943605,57.945531918078),.UNSPECIFIED.);
#287=B_SPLINE_SURFACE_WITH_KNOTS('',3,3,((#66937,#66938,#66939,#66940,#66941,
#66942,#66943,#66944,#66945,#66946,#66947,#66948,#66949,#66950,#66951,#66952,
#66953,#66954,#66955,#66956,#66957,#66958,#66959,#66960,#66961,#66962,#66963,
#66964,#66965,#66966,#66967,#66968,#66969,#66970,#66971,#66972,#66973,#66974,
#66975,#66976,#66977,#66978,#66979,#66980,#66981,#66982,#66983,#66984,#66985,
#66986,#66987,#66988,#66989,#66990,#66991,#66992,#66993,#66994,#66995,#66996,
#66997,#66998,#66999,#67000,#67001,#67002,#67003,#67004,#67005,#67006,#67007,
#67008,#67009,#67010,#67011,#67012,#67013,#67014,#67015,#67016,#67017,#67018,
#67019,#67020,#67021,#67022,#67023,#67024,#67025,#67026,#67027,#67028,#67029,
#67030,#67031,#67032,#67033,#67034,#67035,#67036,#67037,#67038,#67039,#67040,
#67041,#67042,#67043,#67044,#67045,#67046,#67047,#67048,#67049,#67050,#67051,
#67052,#67053,#67054,#67055,#67056,#67057,#67058,#67059,#67060,#67061,#67062,
#67063,#67064,#67065,#67066,#67067,#67068,#67069,#67070,#67071,#67072,#67073,
#67074,#67075,#67076,#67077,#67078,#67079,#67080,#67081,#67082,#67083,#67084,
#67085,#67086,#67087,#67088,#67089,#67090,#67091,#67092,#67093,#67094,#67095,
#67096,#67097,#67098,#67099,#67100,#67101,#67102,#67103,#67104,#67105,#67106,
#67107,#67108,#67109,#67110,#67111,#67112,#67113,#67114,#67115,#67116,#67117,
#67118,#67119,#67120,#67121,#67122,#67123,#67124,#67125,#67126,#67127,#67128,
#67129,#67130,#67131,#67132,#67133,#67134,#67135,#67136,#67137,#67138,#67139,
#67140,#67141,#67142,#67143,#67144,#67145,#67146,#67147,#67148,#67149,#67150,
#67151,#67152,#67153,#67154,#67155,#67156,#67157,#67158,#67159,#67160,#67161,
#67162,#67163,#67164,#67165,#67166,#67167,#67168,#67169,#67170,#67171,#67172,
#67173,#67174,#67175,#67176,#67177,#67178,#67179,#67180,#67181,#67182,#67183,
#67184,#67185,#67186,#67187,#67188,#67189,#67190,#67191,#67192,#67193,#67194,
#67195,#67196,#67197,#67198,#67199,#67200,#67201,#67202,#67203,#67204,#67205,
#67206,#67207,#67208,#67209,#67210,#67211,#67212,#67213,#67214,#67215,#67216,
#67217,#67218,#67219,#67220,#67221,#67222,#67223,#67224,#67225,#67226,#67227,
#67228,#67229,#67230,#67231,#67232,#67233,#67234,#67235,#67236,#67237,#67238,
#67239,#67240,#67241,#67242,#67243,#67244,#67245,#67246,#67247,#67248,#67249,
#67250,#67251,#67252,#67253,#67254,#67255,#67256,#67257,#67258,#67259,#67260,
#67261,#67262,#67263,#67264,#67265,#67266,#67267,#67268,#67269,#67270,#67271,
#67272,#67273,#67274,#67275,#67276,#67277,#67278,#67279,#67280,#67281,#67282,
#67283,#67284,#67285,#67286,#67287,#67288,#67289,#67290,#67291,#67292,#67293,
#67294,#67295,#67296,#67297,#67298,#67299,#67300,#67301,#67302,#67303,#67304,
#67305),(#67306,#67307,#67308,#67309,#67310,#67311,#67312,#67313,#67314,
#67315,#67316,#67317,#67318,#67319,#67320,#67321,#67322,#67323,#67324,#67325,
#67326,#67327,#67328,#67329,#67330,#67331,#67332,#67333,#67334,#67335,#67336,
#67337,#67338,#67339,#67340,#67341,#67342,#67343,#67344,#67345,#67346,#67347,
#67348,#67349,#67350,#67351,#67352,#67353,#67354,#67355,#67356,#67357,#67358,
#67359,#67360,#67361,#67362,#67363,#67364,#67365,#67366,#67367,#67368,#67369,
#67370,#67371,#67372,#67373,#67374,#67375,#67376,#67377,#67378,#67379,#67380,
#67381,#67382,#67383,#67384,#67385,#67386,#67387,#67388,#67389,#67390,#67391,
#67392,#67393,#67394,#67395,#67396,#67397,#67398,#67399,#67400,#67401,#67402,
#67403,#67404,#67405,#67406,#67407,#67408,#67409,#67410,#67411,#67412,#67413,
#67414,#67415,#67416,#67417,#67418,#67419,#67420,#67421,#67422,#67423,#67424,
#67425,#67426,#67427,#67428,#67429,#67430,#67431,#67432,#67433,#67434,#67435,
#67436,#67437,#67438,#67439,#67440,#67441,#67442,#67443,#67444,#67445,#67446,
#67447,#67448,#67449,#67450,#67451,#67452,#67453,#67454,#67455,#67456,#67457,
#67458,#67459,#67460,#67461,#67462,#67463,#67464,#67465,#67466,#67467,#67468,
#67469,#67470,#67471,#67472,#67473,#67474,#67475,#67476,#67477,#67478,#67479,
#67480,#67481,#67482,#67483,#67484,#67485,#67486,#67487,#67488,#67489,#67490,
#67491,#67492,#67493,#67494,#67495,#67496,#67497,#67498,#67499,#67500,#67501,
#67502,#67503,#67504,#67505,#67506,#67507,#67508,#67509,#67510,#67511,#67512,
#67513,#67514,#67515,#67516,#67517,#67518,#67519,#67520,#67521,#67522,#67523,
#67524,#67525,#67526,#67527,#67528,#67529,#67530,#67531,#67532,#67533,#67534,
#67535,#67536,#67537,#67538,#67539,#67540,#67541,#67542,#67543,#67544,#67545,
#67546,#67547,#67548,#67549,#67550,#67551,#67552,#67553,#67554,#67555,#67556,
#67557,#67558,#67559,#67560,#67561,#67562,#67563,#67564,#67565,#67566,#67567,
#67568,#67569,#67570,#67571,#67572,#67573,#67574,#67575,#67576,#67577,#67578,
#67579,#67580,#67581,#67582,#67583,#67584,#67585,#67586,#67587,#67588,#67589,
#67590,#67591,#67592,#67593,#67594,#67595,#67596,#67597,#67598,#67599,#67600,
#67601,#67602,#67603,#67604,#67605,#67606,#67607,#67608,#67609,#67610,#67611,
#67612,#67613,#67614,#67615,#67616,#67617,#67618,#67619,#67620,#67621,#67622,
#67623,#67624,#67625,#67626,#67627,#67628,#67629,#67630,#67631,#67632,#67633,
#67634,#67635,#67636,#67637,#67638,#67639,#67640,#67641,#67642,#67643,#67644,
#67645,#67646,#67647,#67648,#67649,#67650,#67651,#67652,#67653,#67654,#67655,
#67656,#67657,#67658,#67659,#67660,#67661,#67662,#67663,#67664,#67665,#67666,
#67667,#67668,#67669,#67670,#67671,#67672,#67673,#67674),(#67675,#67676,
#67677,#67678,#67679,#67680,#67681,#67682,#67683,#67684,#67685,#67686,#67687,
#67688,#67689,#67690,#67691,#67692,#67693,#67694,#67695,#67696,#67697,#67698,
#67699,#67700,#67701,#67702,#67703,#67704,#67705,#67706,#67707,#67708,#67709,
#67710,#67711,#67712,#67713,#67714,#67715,#67716,#67717,#67718,#67719,#67720,
#67721,#67722,#67723,#67724,#67725,#67726,#67727,#67728,#67729,#67730,#67731,
#67732,#67733,#67734,#67735,#67736,#67737,#67738,#67739,#67740,#67741,#67742,
#67743,#67744,#67745,#67746,#67747,#67748,#67749,#67750,#67751,#67752,#67753,
#67754,#67755,#67756,#67757,#67758,#67759,#67760,#67761,#67762,#67763,#67764,
#67765,#67766,#67767,#67768,#67769,#67770,#67771,#67772,#67773,#67774,#67775,
#67776,#67777,#67778,#67779,#67780,#67781,#67782,#67783,#67784,#67785,#67786,
#67787,#67788,#67789,#67790,#67791,#67792,#67793,#67794,#67795,#67796,#67797,
#67798,#67799,#67800,#67801,#67802,#67803,#67804,#67805,#67806,#67807,#67808,
#67809,#67810,#67811,#67812,#67813,#67814,#67815,#67816,#67817,#67818,#67819,
#67820,#67821,#67822,#67823,#67824,#67825,#67826,#67827,#67828,#67829,#67830,
#67831,#67832,#67833,#67834,#67835,#67836,#67837,#67838,#67839,#67840,#67841,
#67842,#67843,#67844,#67845,#67846,#67847,#67848,#67849,#67850,#67851,#67852,
#67853,#67854,#67855,#67856,#67857,#67858,#67859,#67860,#67861,#67862,#67863,
#67864,#67865,#67866,#67867,#67868,#67869,#67870,#67871,#67872,#67873,#67874,
#67875,#67876,#67877,#67878,#67879,#67880,#67881,#67882,#67883,#67884,#67885,
#67886,#67887,#67888,#67889,#67890,#67891,#67892,#67893,#67894,#67895,#67896,
#67897,#67898,#67899,#67900,#67901,#67902,#67903,#67904,#67905,#67906,#67907,
#67908,#67909,#67910,#67911,#67912,#67913,#67914,#67915,#67916,#67917,#67918,
#67919,#67920,#67921,#67922,#67923,#67924,#67925,#67926,#67927,#67928,#67929,
#67930,#67931,#67932,#67933,#67934,#67935,#67936,#67937,#67938,#67939,#67940,
#67941,#67942,#67943,#67944,#67945,#67946,#67947,#67948,#67949,#67950,#67951,
#67952,#67953,#67954,#67955,#67956,#67957,#67958,#67959,#67960,#67961,#67962,
#67963,#67964,#67965,#67966,#67967,#67968,#67969,#67970,#67971,#67972,#67973,
#67974,#67975,#67976,#67977,#67978,#67979,#67980,#67981,#67982,#67983,#67984,
#67985,#67986,#67987,#67988,#67989,#67990,#67991,#67992,#67993,#67994,#67995,
#67996,#67997,#67998,#67999,#68000,#68001,#68002,#68003,#68004,#68005,#68006,
#68007,#68008,#68009,#68010,#68011,#68012,#68013,#68014,#68015,#68016,#68017,
#68018,#68019,#68020,#68021,#68022,#68023,#68024,#68025,#68026,#68027,#68028,
#68029,#68030,#68031,#68032,#68033,#68034,#68035,#68036,#68037,#68038,#68039,
#68040,#68041,#68042,#68043),(#68044,#68045,#68046,#68047,#68048,#68049,
#68050,#68051,#68052,#68053,#68054,#68055,#68056,#68057,#68058,#68059,#68060,
#68061,#68062,#68063,#68064,#68065,#68066,#68067,#68068,#68069,#68070,#68071,
#68072,#68073,#68074,#68075,#68076,#68077,#68078,#68079,#68080,#68081,#68082,
#68083,#68084,#68085,#68086,#68087,#68088,#68089,#68090,#68091,#68092,#68093,
#68094,#68095,#68096,#68097,#68098,#68099,#68100,#68101,#68102,#68103,#68104,
#68105,#68106,#68107,#68108,#68109,#68110,#68111,#68112,#68113,#68114,#68115,
#68116,#68117,#68118,#68119,#68120,#68121,#68122,#68123,#68124,#68125,#68126,
#68127,#68128,#68129,#68130,#68131,#68132,#68133,#68134,#68135,#68136,#68137,
#68138,#68139,#68140,#68141,#68142,#68143,#68144,#68145,#68146,#68147,#68148,
#68149,#68150,#68151,#68152,#68153,#68154,#68155,#68156,#68157,#68158,#68159,
#68160,#68161,#68162,#68163,#68164,#68165,#68166,#68167,#68168,#68169,#68170,
#68171,#68172,#68173,#68174,#68175,#68176,#68177,#68178,#68179,#68180,#68181,
#68182,#68183,#68184,#68185,#68186,#68187,#68188,#68189,#68190,#68191,#68192,
#68193,#68194,#68195,#68196,#68197,#68198,#68199,#68200,#68201,#68202,#68203,
#68204,#68205,#68206,#68207,#68208,#68209,#68210,#68211,#68212,#68213,#68214,
#68215,#68216,#68217,#68218,#68219,#68220,#68221,#68222,#68223,#68224,#68225,
#68226,#68227,#68228,#68229,#68230,#68231,#68232,#68233,#68234,#68235,#68236,
#68237,#68238,#68239,#68240,#68241,#68242,#68243,#68244,#68245,#68246,#68247,
#68248,#68249,#68250,#68251,#68252,#68253,#68254,#68255,#68256,#68257,#68258,
#68259,#68260,#68261,#68262,#68263,#68264,#68265,#68266,#68267,#68268,#68269,
#68270,#68271,#68272,#68273,#68274,#68275,#68276,#68277,#68278,#68279,#68280,
#68281,#68282,#68283,#68284,#68285,#68286,#68287,#68288,#68289,#68290,#68291,
#68292,#68293,#68294,#68295,#68296,#68297,#68298,#68299,#68300,#68301,#68302,
#68303,#68304,#68305,#68306,#68307,#68308,#68309,#68310,#68311,#68312,#68313,
#68314,#68315,#68316,#68317,#68318,#68319,#68320,#68321,#68322,#68323,#68324,
#68325,#68326,#68327,#68328,#68329,#68330,#68331,#68332,#68333,#68334,#68335,
#68336,#68337,#68338,#68339,#68340,#68341,#68342,#68343,#68344,#68345,#68346,
#68347,#68348,#68349,#68350,#68351,#68352,#68353,#68354,#68355,#68356,#68357,
#68358,#68359,#68360,#68361,#68362,#68363,#68364,#68365,#68366,#68367,#68368,
#68369,#68370,#68371,#68372,#68373,#68374,#68375,#68376,#68377,#68378,#68379,
#68380,#68381,#68382,#68383,#68384,#68385,#68386,#68387,#68388,#68389,#68390,
#68391,#68392,#68393,#68394,#68395,#68396,#68397,#68398,#68399,#68400,#68401,
#68402,#68403,#68404,#68405,#68406,#68407,#68408,#68409,#68410,#68411,#68412)),
 .UNSPECIFIED.,.F.,.F.,.F.,(4,4),(4,1,1,1,1,1,1,1,1,1,1,1,1,1,1,1,1,1,1,
1,1,1,1,1,1,1,1,1,1,1,1,1,1,1,1,1,1,1,1,1,1,1,1,1,1,1,1,1,1,1,1,1,1,1,1,
1,1,1,1,1,1,1,1,1,1,1,1,1,1,1,1,1,1,1,1,1,1,1,1,1,1,1,1,1,1,1,1,1,1,1,1,
1,1,1,1,1,1,1,1,1,1,1,1,1,1,1,1,1,1,1,1,1,1,1,1,1,1,1,1,1,1,1,1,1,1,1,1,
1,1,1,1,1,1,1,1,1,1,1,1,1,1,1,1,1,1,1,1,1,1,1,1,1,1,1,1,1,1,1,1,1,1,1,1,
1,1,1,1,1,1,1,1,1,1,1,1,1,1,1,1,1,1,1,1,1,1,1,1,1,1,1,1,1,1,1,1,1,1,1,1,
1,1,1,1,1,1,1,1,1,1,1,1,1,1,1,1,1,1,1,1,1,1,1,1,1,1,1,1,1,1,1,1,1,1,1,1,
1,1,1,1,1,1,1,1,1,1,1,1,1,1,1,1,1,1,1,1,1,1,1,1,1,1,1,1,1,1,1,1,1,1,1,1,
1,1,1,1,1,1,1,1,1,1,1,1,1,1,1,1,1,1,1,1,1,1,1,1,1,1,1,1,1,1,1,1,1,1,1,1,
1,1,1,1,1,1,1,1,1,1,1,1,1,1,1,1,1,1,1,1,1,1,1,1,1,1,1,1,1,1,1,1,1,1,1,1,
1,1,1,1,1,1,1,1,1,1,1,1,1,1,1,1,1,1,1,1,1,1,1,4),(0.,0.0813890674476615),
(8.31473274985811,8.81229131725278,9.30984988464746,9.80740845204213,10.3049670194368,
10.8025255868315,11.3000841542261,11.7976427216208,12.2952012890155,12.7927598564102,
13.2903184238048,13.7878769911995,14.2854355585942,14.7829941259888,15.2805526933835,
15.7781112607782,16.2756698281729,16.7732283955675,17.2707869629622,17.7683455303569,
18.2659040977515,18.7634626651462,19.2610212325409,19.7585797999356,20.2561383673302,
20.7536969347249,21.2512555021196,21.7488140695142,22.2463726369089,22.7439312043036,
23.2414897716983,23.7390483390929,24.2366069064876,24.7341654738823,25.231724041277,
25.7292826086716,26.2268411760663,26.724399743461,27.2219583108556,27.7195168782503,
28.217075445645,28.7146340130397,29.2121925804343,29.709751147829,30.2073097152237,
30.7048682826183,31.202426850013,31.6999854174077,32.1975439848024,32.695102552197,
33.1926611195917,33.6902196869864,34.187778254381,34.6853368217757,35.1828953891704,
35.6804539565651,36.1780125239597,36.6755710913544,37.1731296587491,37.6706882261438,
38.1682467935384,38.6658053609331,39.1633639283278,39.6609224957224,40.1584810631171,
40.6560396305118,41.1535981979065,41.6511567653011,42.1487153326958,42.6462739000905,
43.1438324674851,43.6413910348798,44.1389496022745,44.6365081696692,45.1340667370638,
45.6316253044585,46.1291838718532,46.6267424392478,47.1243010066425,47.6218595740372,
48.1194181414319,48.6169767088265,49.1145352762212,49.6120938436159,50.1096524110105,
50.6072109784052,51.1047695457999,51.6023281131946,52.0998866805892,52.5974452479839,
53.0950038153786,53.5925623827733,54.0901209501679,54.5876795175626,55.0852380849573,
55.5827966523519,56.0803552197466,56.5779137871413,57.075472354536,57.5730309219306,
58.0705894893253,58.56814805672,59.0657066241146,59.5632651915093,60.060823758904,
60.5583823262987,61.0559408936933,61.553499461088,62.0510580284827,62.5486165958773,
63.046175163272,63.5437337306667,64.0412922980614,64.538850865456,65.0364094328507,
65.5339680002454,66.03152656764,66.5290851350347,67.0266437024294,67.5242022698241,
68.0217608372187,68.5193194046134,69.0168779720081,69.5144365394028,70.0119951067974,
70.5095536741921,71.0071122415868,71.5046708089814,72.0022293763761,72.4997879437708,
72.9973465111654,73.4949050785601,73.9924636459548,74.4900222133495,74.9875807807441,
75.4851393481388,75.9826979155335,76.4802564829282,76.9778150503228,77.4753736177175,
77.9729321851122,78.4704907525068,78.9680493199015,79.4656078872962,79.9631664546908,
80.4607250220855,80.9582835894802,81.4558421568749,81.9534007242695,82.4509592916642,
82.9485178590589,83.4460764264536,83.9436349938482,84.4411935612429,84.9387521286376,
85.4363106960323,85.9338692634269,86.4314278308216,86.9289863982163,87.4265449656109,
87.9241035330056,88.4216621004003,88.9192206677949,89.4167792351896,89.9143378025843,
90.411896369979,90.9094549373736,91.4070135047683,91.904572072163,92.4021306395577,
92.8996892069523,93.397247774347,93.8948063417417,94.3923649091363,94.889923476531,
95.3874820439257,95.8850406113204,96.382599178715,96.8801577461097,97.3777163135044,
97.875274880899,98.3728334482937,98.8703920156884,99.3679505830831,99.8655091504777,
100.363067717872,100.860626285267,101.358184852662,101.855743420056,102.353301987451,
102.850860554846,103.34841912224,103.845977689635,104.34353625703,104.841094824424,
105.338653391819,105.836211959214,106.333770526608,106.831329094003,107.328887661398,
107.826446228792,108.324004796187,108.821563363582,109.319121930977,109.816680498371,
110.314239065766,110.811797633161,111.309356200555,111.80691476795,112.304473335345,
112.802031902739,113.299590470134,113.797149037529,114.294707604923,114.792266172318,
115.289824739713,115.787383307107,116.284941874502,116.782500441897,117.280059009291,
117.777617576686,118.275176144081,118.772734711475,119.27029327887,119.767851846265,
120.265410413659,120.762968981054,121.260527548449,121.758086115843,122.255644683238,
122.753203250633,123.250761818027,123.748320385422,124.245878952817,124.743437520211,
125.240996087606,125.738554655001,126.236113222395,126.73367178979,127.231230357185,
127.728788924579,128.226347491974,128.723906059369,129.221464626763,129.719023194158,
130.216581761553,130.714140328947,131.211698896342,131.709257463737,132.206816031131,
132.704374598526,133.201933165921,133.699491733315,134.19705030071,134.694608868105,
135.192167435499,135.689726002894,136.187284570289,136.684843137683,137.182401705078,
137.679960272473,138.177518839867,138.675077407262,139.172635974657,139.670194542051,
140.167753109446,140.665311676841,141.162870244235,141.66042881163,142.157987379025,
142.65554594642,143.153104513814,143.650663081209,144.148221648604,144.645780215998,
145.143338783393,145.640897350788,146.138455918182,146.636014485577,147.133573052972,
147.631131620366,148.128690187761,148.626248755156,149.12380732255,149.621365889945,
150.11892445734,150.616483024734,151.114041592129,151.611600159524,152.109158726918,
152.606717294313,153.104275861708,153.601834429102,154.099392996497,154.596951563892,
155.094510131286,155.592068698681,156.089627266076,156.58718583347,157.084744400865,
157.58230296826,158.079861535654,158.577420103049,159.074978670444,159.572537237838,
160.070095805233,160.567654372628,161.065212940022,161.562771507417,162.060330074812,
162.557888642206,163.055447209601,163.553005776996,164.05056434439,164.548122911785,
165.04568147918,165.543240046574,166.040798613969,166.538357181364,167.035915748758,
167.533474316153,168.031032883548,168.528591450942,169.026150018337,169.523708585732,
170.021267153126,170.518825720521,171.016384287916,171.51394285531,172.011501422705,
172.5090599901,173.006618557495,173.504177124889,174.001735692284,174.499294259679,
174.996852827073,175.494411394468,175.991969961863,176.489528529257,176.987087096652,
177.484645664047,177.982204231441,178.479762798836,178.977321366231,179.474879933625,
179.97243850102,180.469997068415,180.967555635809,181.465114203204,181.962672770599,
182.460231337993,182.957789905388,183.455348472783,183.952907040177,184.450465607572,
184.948024174967,185.445582742361,185.943141309756,186.440699877151,186.938258444545,
187.43581701194,187.933375579335,188.430934146729,188.928492714124,189.426051281519,
189.923609848913,190.421168416308),.UNSPECIFIED.);
#288=B_SPLINE_SURFACE_WITH_KNOTS('',3,3,((#68690,#68691,#68692,#68693,#68694,
#68695,#68696,#68697,#68698,#68699,#68700,#68701,#68702,#68703,#68704,#68705,
#68706,#68707,#68708,#68709,#68710,#68711,#68712,#68713,#68714,#68715,#68716,
#68717,#68718,#68719,#68720,#68721,#68722,#68723,#68724,#68725,#68726,#68727,
#68728,#68729,#68730,#68731,#68732,#68733,#68734,#68735,#68736,#68737,#68738,
#68739,#68740,#68741,#68742,#68743,#68744,#68745,#68746,#68747,#68748,#68749,
#68750,#68751,#68752,#68753,#68754,#68755,#68756,#68757,#68758,#68759,#68760,
#68761,#68762,#68763,#68764,#68765,#68766,#68767,#68768,#68769,#68770,#68771,
#68772,#68773,#68774,#68775,#68776,#68777,#68778,#68779,#68780,#68781,#68782,
#68783,#68784,#68785,#68786,#68787,#68788,#68789,#68790,#68791,#68792,#68793,
#68794,#68795,#68796,#68797,#68798,#68799,#68800,#68801,#68802,#68803,#68804,
#68805,#68806,#68807,#68808,#68809,#68810,#68811,#68812,#68813,#68814,#68815,
#68816,#68817,#68818,#68819,#68820,#68821,#68822,#68823,#68824,#68825,#68826,
#68827,#68828,#68829,#68830,#68831,#68832,#68833,#68834,#68835,#68836,#68837,
#68838,#68839,#68840,#68841,#68842,#68843,#68844,#68845,#68846,#68847,#68848,
#68849,#68850,#68851,#68852,#68853,#68854,#68855,#68856,#68857,#68858,#68859,
#68860,#68861,#68862,#68863,#68864,#68865,#68866,#68867,#68868,#68869,#68870,
#68871,#68872,#68873,#68874,#68875,#68876,#68877,#68878,#68879,#68880,#68881,
#68882,#68883,#68884,#68885,#68886,#68887,#68888,#68889,#68890,#68891,#68892,
#68893,#68894,#68895,#68896,#68897,#68898,#68899,#68900,#68901,#68902,#68903,
#68904,#68905,#68906,#68907,#68908,#68909,#68910,#68911,#68912,#68913,#68914,
#68915,#68916,#68917,#68918,#68919,#68920,#68921,#68922,#68923,#68924,#68925,
#68926,#68927,#68928,#68929,#68930,#68931,#68932,#68933,#68934,#68935,#68936,
#68937,#68938,#68939,#68940,#68941,#68942,#68943,#68944,#68945,#68946,#68947,
#68948,#68949,#68950,#68951,#68952,#68953,#68954,#68955,#68956,#68957,#68958,
#68959,#68960,#68961,#68962,#68963,#68964,#68965,#68966,#68967,#68968,#68969,
#68970,#68971,#68972,#68973,#68974,#68975,#68976,#68977,#68978,#68979,#68980,
#68981,#68982,#68983,#68984,#68985,#68986,#68987,#68988,#68989,#68990,#68991,
#68992,#68993,#68994,#68995,#68996,#68997,#68998,#68999,#69000,#69001,#69002,
#69003,#69004,#69005,#69006,#69007,#69008,#69009,#69010,#69011,#69012,#69013,
#69014,#69015,#69016,#69017,#69018,#69019,#69020,#69021,#69022,#69023,#69024,
#69025,#69026,#69027,#69028,#69029,#69030,#69031,#69032,#69033,#69034,#69035,
#69036,#69037,#69038,#69039,#69040,#69041,#69042,#69043,#69044,#69045,#69046,
#69047,#69048,#69049,#69050,#69051,#69052,#69053,#69054,#69055,#69056,#69057,
#69058),(#69059,#69060,#69061,#69062,#69063,#69064,#69065,#69066,#69067,
#69068,#69069,#69070,#69071,#69072,#69073,#69074,#69075,#69076,#69077,#69078,
#69079,#69080,#69081,#69082,#69083,#69084,#69085,#69086,#69087,#69088,#69089,
#69090,#69091,#69092,#69093,#69094,#69095,#69096,#69097,#69098,#69099,#69100,
#69101,#69102,#69103,#69104,#69105,#69106,#69107,#69108,#69109,#69110,#69111,
#69112,#69113,#69114,#69115,#69116,#69117,#69118,#69119,#69120,#69121,#69122,
#69123,#69124,#69125,#69126,#69127,#69128,#69129,#69130,#69131,#69132,#69133,
#69134,#69135,#69136,#69137,#69138,#69139,#69140,#69141,#69142,#69143,#69144,
#69145,#69146,#69147,#69148,#69149,#69150,#69151,#69152,#69153,#69154,#69155,
#69156,#69157,#69158,#69159,#69160,#69161,#69162,#69163,#69164,#69165,#69166,
#69167,#69168,#69169,#69170,#69171,#69172,#69173,#69174,#69175,#69176,#69177,
#69178,#69179,#69180,#69181,#69182,#69183,#69184,#69185,#69186,#69187,#69188,
#69189,#69190,#69191,#69192,#69193,#69194,#69195,#69196,#69197,#69198,#69199,
#69200,#69201,#69202,#69203,#69204,#69205,#69206,#69207,#69208,#69209,#69210,
#69211,#69212,#69213,#69214,#69215,#69216,#69217,#69218,#69219,#69220,#69221,
#69222,#69223,#69224,#69225,#69226,#69227,#69228,#69229,#69230,#69231,#69232,
#69233,#69234,#69235,#69236,#69237,#69238,#69239,#69240,#69241,#69242,#69243,
#69244,#69245,#69246,#69247,#69248,#69249,#69250,#69251,#69252,#69253,#69254,
#69255,#69256,#69257,#69258,#69259,#69260,#69261,#69262,#69263,#69264,#69265,
#69266,#69267,#69268,#69269,#69270,#69271,#69272,#69273,#69274,#69275,#69276,
#69277,#69278,#69279,#69280,#69281,#69282,#69283,#69284,#69285,#69286,#69287,
#69288,#69289,#69290,#69291,#69292,#69293,#69294,#69295,#69296,#69297,#69298,
#69299,#69300,#69301,#69302,#69303,#69304,#69305,#69306,#69307,#69308,#69309,
#69310,#69311,#69312,#69313,#69314,#69315,#69316,#69317,#69318,#69319,#69320,
#69321,#69322,#69323,#69324,#69325,#69326,#69327,#69328,#69329,#69330,#69331,
#69332,#69333,#69334,#69335,#69336,#69337,#69338,#69339,#69340,#69341,#69342,
#69343,#69344,#69345,#69346,#69347,#69348,#69349,#69350,#69351,#69352,#69353,
#69354,#69355,#69356,#69357,#69358,#69359,#69360,#69361,#69362,#69363,#69364,
#69365,#69366,#69367,#69368,#69369,#69370,#69371,#69372,#69373,#69374,#69375,
#69376,#69377,#69378,#69379,#69380,#69381,#69382,#69383,#69384,#69385,#69386,
#69387,#69388,#69389,#69390,#69391,#69392,#69393,#69394,#69395,#69396,#69397,
#69398,#69399,#69400,#69401,#69402,#69403,#69404,#69405,#69406,#69407,#69408,
#69409,#69410,#69411,#69412,#69413,#69414,#69415,#69416,#69417,#69418,#69419,
#69420,#69421,#69422,#69423,#69424,#69425,#69426,#69427),(#69428,#69429,
#69430,#69431,#69432,#69433,#69434,#69435,#69436,#69437,#69438,#69439,#69440,
#69441,#69442,#69443,#69444,#69445,#69446,#69447,#69448,#69449,#69450,#69451,
#69452,#69453,#69454,#69455,#69456,#69457,#69458,#69459,#69460,#69461,#69462,
#69463,#69464,#69465,#69466,#69467,#69468,#69469,#69470,#69471,#69472,#69473,
#69474,#69475,#69476,#69477,#69478,#69479,#69480,#69481,#69482,#69483,#69484,
#69485,#69486,#69487,#69488,#69489,#69490,#69491,#69492,#69493,#69494,#69495,
#69496,#69497,#69498,#69499,#69500,#69501,#69502,#69503,#69504,#69505,#69506,
#69507,#69508,#69509,#69510,#69511,#69512,#69513,#69514,#69515,#69516,#69517,
#69518,#69519,#69520,#69521,#69522,#69523,#69524,#69525,#69526,#69527,#69528,
#69529,#69530,#69531,#69532,#69533,#69534,#69535,#69536,#69537,#69538,#69539,
#69540,#69541,#69542,#69543,#69544,#69545,#69546,#69547,#69548,#69549,#69550,
#69551,#69552,#69553,#69554,#69555,#69556,#69557,#69558,#69559,#69560,#69561,
#69562,#69563,#69564,#69565,#69566,#69567,#69568,#69569,#69570,#69571,#69572,
#69573,#69574,#69575,#69576,#69577,#69578,#69579,#69580,#69581,#69582,#69583,
#69584,#69585,#69586,#69587,#69588,#69589,#69590,#69591,#69592,#69593,#69594,
#69595,#69596,#69597,#69598,#69599,#69600,#69601,#69602,#69603,#69604,#69605,
#69606,#69607,#69608,#69609,#69610,#69611,#69612,#69613,#69614,#69615,#69616,
#69617,#69618,#69619,#69620,#69621,#69622,#69623,#69624,#69625,#69626,#69627,
#69628,#69629,#69630,#69631,#69632,#69633,#69634,#69635,#69636,#69637,#69638,
#69639,#69640,#69641,#69642,#69643,#69644,#69645,#69646,#69647,#69648,#69649,
#69650,#69651,#69652,#69653,#69654,#69655,#69656,#69657,#69658,#69659,#69660,
#69661,#69662,#69663,#69664,#69665,#69666,#69667,#69668,#69669,#69670,#69671,
#69672,#69673,#69674,#69675,#69676,#69677,#69678,#69679,#69680,#69681,#69682,
#69683,#69684,#69685,#69686,#69687,#69688,#69689,#69690,#69691,#69692,#69693,
#69694,#69695,#69696,#69697,#69698,#69699,#69700,#69701,#69702,#69703,#69704,
#69705,#69706,#69707,#69708,#69709,#69710,#69711,#69712,#69713,#69714,#69715,
#69716,#69717,#69718,#69719,#69720,#69721,#69722,#69723,#69724,#69725,#69726,
#69727,#69728,#69729,#69730,#69731,#69732,#69733,#69734,#69735,#69736,#69737,
#69738,#69739,#69740,#69741,#69742,#69743,#69744,#69745,#69746,#69747,#69748,
#69749,#69750,#69751,#69752,#69753,#69754,#69755,#69756,#69757,#69758,#69759,
#69760,#69761,#69762,#69763,#69764,#69765,#69766,#69767,#69768,#69769,#69770,
#69771,#69772,#69773,#69774,#69775,#69776,#69777,#69778,#69779,#69780,#69781,
#69782,#69783,#69784,#69785,#69786,#69787,#69788,#69789,#69790,#69791,#69792,
#69793,#69794,#69795,#69796),(#69797,#69798,#69799,#69800,#69801,#69802,
#69803,#69804,#69805,#69806,#69807,#69808,#69809,#69810,#69811,#69812,#69813,
#69814,#69815,#69816,#69817,#69818,#69819,#69820,#69821,#69822,#69823,#69824,
#69825,#69826,#69827,#69828,#69829,#69830,#69831,#69832,#69833,#69834,#69835,
#69836,#69837,#69838,#69839,#69840,#69841,#69842,#69843,#69844,#69845,#69846,
#69847,#69848,#69849,#69850,#69851,#69852,#69853,#69854,#69855,#69856,#69857,
#69858,#69859,#69860,#69861,#69862,#69863,#69864,#69865,#69866,#69867,#69868,
#69869,#69870,#69871,#69872,#69873,#69874,#69875,#69876,#69877,#69878,#69879,
#69880,#69881,#69882,#69883,#69884,#69885,#69886,#69887,#69888,#69889,#69890,
#69891,#69892,#69893,#69894,#69895,#69896,#69897,#69898,#69899,#69900,#69901,
#69902,#69903,#69904,#69905,#69906,#69907,#69908,#69909,#69910,#69911,#69912,
#69913,#69914,#69915,#69916,#69917,#69918,#69919,#69920,#69921,#69922,#69923,
#69924,#69925,#69926,#69927,#69928,#69929,#69930,#69931,#69932,#69933,#69934,
#69935,#69936,#69937,#69938,#69939,#69940,#69941,#69942,#69943,#69944,#69945,
#69946,#69947,#69948,#69949,#69950,#69951,#69952,#69953,#69954,#69955,#69956,
#69957,#69958,#69959,#69960,#69961,#69962,#69963,#69964,#69965,#69966,#69967,
#69968,#69969,#69970,#69971,#69972,#69973,#69974,#69975,#69976,#69977,#69978,
#69979,#69980,#69981,#69982,#69983,#69984,#69985,#69986,#69987,#69988,#69989,
#69990,#69991,#69992,#69993,#69994,#69995,#69996,#69997,#69998,#69999,#70000,
#70001,#70002,#70003,#70004,#70005,#70006,#70007,#70008,#70009,#70010,#70011,
#70012,#70013,#70014,#70015,#70016,#70017,#70018,#70019,#70020,#70021,#70022,
#70023,#70024,#70025,#70026,#70027,#70028,#70029,#70030,#70031,#70032,#70033,
#70034,#70035,#70036,#70037,#70038,#70039,#70040,#70041,#70042,#70043,#70044,
#70045,#70046,#70047,#70048,#70049,#70050,#70051,#70052,#70053,#70054,#70055,
#70056,#70057,#70058,#70059,#70060,#70061,#70062,#70063,#70064,#70065,#70066,
#70067,#70068,#70069,#70070,#70071,#70072,#70073,#70074,#70075,#70076,#70077,
#70078,#70079,#70080,#70081,#70082,#70083,#70084,#70085,#70086,#70087,#70088,
#70089,#70090,#70091,#70092,#70093,#70094,#70095,#70096,#70097,#70098,#70099,
#70100,#70101,#70102,#70103,#70104,#70105,#70106,#70107,#70108,#70109,#70110,
#70111,#70112,#70113,#70114,#70115,#70116,#70117,#70118,#70119,#70120,#70121,
#70122,#70123,#70124,#70125,#70126,#70127,#70128,#70129,#70130,#70131,#70132,
#70133,#70134,#70135,#70136,#70137,#70138,#70139,#70140,#70141,#70142,#70143,
#70144,#70145,#70146,#70147,#70148,#70149,#70150,#70151,#70152,#70153,#70154,
#70155,#70156,#70157,#70158,#70159,#70160,#70161,#70162,#70163,#70164,#70165)),
 .UNSPECIFIED.,.F.,.F.,.F.,(4,4),(4,1,1,1,1,1,1,1,1,1,1,1,1,1,1,1,1,1,1,
1,1,1,1,1,1,1,1,1,1,1,1,1,1,1,1,1,1,1,1,1,1,1,1,1,1,1,1,1,1,1,1,1,1,1,1,
1,1,1,1,1,1,1,1,1,1,1,1,1,1,1,1,1,1,1,1,1,1,1,1,1,1,1,1,1,1,1,1,1,1,1,1,
1,1,1,1,1,1,1,1,1,1,1,1,1,1,1,1,1,1,1,1,1,1,1,1,1,1,1,1,1,1,1,1,1,1,1,1,
1,1,1,1,1,1,1,1,1,1,1,1,1,1,1,1,1,1,1,1,1,1,1,1,1,1,1,1,1,1,1,1,1,1,1,1,
1,1,1,1,1,1,1,1,1,1,1,1,1,1,1,1,1,1,1,1,1,1,1,1,1,1,1,1,1,1,1,1,1,1,1,1,
1,1,1,1,1,1,1,1,1,1,1,1,1,1,1,1,1,1,1,1,1,1,1,1,1,1,1,1,1,1,1,1,1,1,1,1,
1,1,1,1,1,1,1,1,1,1,1,1,1,1,1,1,1,1,1,1,1,1,1,1,1,1,1,1,1,1,1,1,1,1,1,1,
1,1,1,1,1,1,1,1,1,1,1,1,1,1,1,1,1,1,1,1,1,1,1,1,1,1,1,1,1,1,1,1,1,1,1,1,
1,1,1,1,1,1,1,1,1,1,1,1,1,1,1,1,1,1,1,1,1,1,1,1,1,1,1,1,1,1,1,1,1,1,1,1,
1,1,1,1,1,1,1,1,1,1,1,1,1,1,1,1,1,1,1,1,1,1,1,4),(0.,0.0813890674476615),
(11.6630985309706,12.1606570983653,12.65821566576,13.1557742331546,13.6533328005493,
14.150891367944,14.6484499353386,15.1460085027333,15.643567070128,16.1411256375227,
16.6386842049173,17.136242772312,17.6338013397067,18.1313599071013,18.628918474496,
19.1264770418907,19.6240356092854,20.12159417668,20.6191527440747,21.1167113114694,
21.6142698788641,22.1118284462587,22.6093870136534,23.1069455810481,23.6045041484427,
24.1020627158374,24.5996212832321,25.0971798506268,25.5947384180214,26.0922969854161,
26.5898555528108,27.0874141202054,27.5849726876001,28.0825312549948,28.5800898223895,
29.0776483897841,29.5752069571788,30.0727655245735,30.5703240919681,31.0678826593628,
31.5654412267575,32.0629997941522,32.5605583615468,33.0581169289415,33.5556754963362,
34.0532340637308,34.5507926311255,35.0483511985202,35.5459097659149,36.0434683333095,
36.5410269007042,37.0385854680989,37.5361440354935,38.0337026028882,38.5312611702829,
39.0288197376776,39.5263783050722,40.0239368724669,40.5214954398616,41.0190540072562,
41.5166125746509,42.0141711420456,42.5117297094403,43.0092882768349,43.5068468442296,
44.0044054116243,44.501963979019,44.9995225464136,45.4970811138083,45.994639681203,
46.4921982485976,46.9897568159923,47.487315383387,47.9848739507816,48.4824325181763,
48.979991085571,49.4775496529657,49.9751082203603,50.472666787755,50.9702253551497,
51.4677839225444,51.965342489939,52.4629010573337,52.9604596247284,53.458018192123,
53.9555767595177,54.4531353269124,54.9506938943071,55.4482524617017,55.9458110290964,
56.4433695964911,56.9409281638857,57.4384867312804,57.9360452986751,58.4336038660698,
58.9311624334644,59.4287210008591,59.9262795682538,60.4238381356484,60.9213967030431,
61.4189552704378,61.9165138378325,62.4140724052271,62.9116309726218,63.4091895400165,
63.9067481074111,64.4043066748058,64.9018652422005,65.3994238095952,65.8969823769898,
66.3945409443845,66.8920995117792,67.3896580791738,67.8872166465685,68.3847752139632,
68.8823337813579,69.3798923487525,69.8774509161472,70.3750094835419,70.8725680509366,
71.3701266183312,71.8676851857259,72.3652437531206,72.8628023205152,73.3603608879099,
73.8579194553046,74.3554780226992,74.8530365900939,75.3505951574886,75.8481537248833,
76.3457122922779,76.8432708596726,77.3408294270673,77.838387994462,78.3359465618566,
78.8335051292513,79.331063696646,79.8286222640406,80.3261808314353,80.82373939883,
81.3212979662247,81.8188565336193,82.316415101014,82.8139736684087,83.3115322358033,
83.809090803198,84.3066493705927,84.8042079379874,85.301766505382,85.7993250727767,
86.2968836401714,86.794442207566,87.2920007749607,87.7895593423554,88.2871179097501,
88.7846764771447,89.2822350445394,89.7797936119341,90.2773521793287,90.7749107467234,
91.2724693141181,91.7700278815128,92.2675864489074,92.7651450163021,93.2627035836968,
93.7602621510915,94.2578207184861,94.7553792858808,95.2529378532755,95.7504964206701,
96.2480549880648,96.7456135554595,97.2431721228542,97.7407306902488,98.2382892576435,
98.7358478250382,99.2334063924328,99.7309649598275,100.228523527222,100.726082094617,
101.223640662012,101.721199229406,102.218757796801,102.716316364196,103.21387493159,
103.711433498985,104.20899206638,104.706550633774,105.204109201169,105.701667768564,
106.199226335958,106.696784903353,107.194343470748,107.691902038142,108.189460605537,
108.687019172932,109.184577740326,109.682136307721,110.179694875116,110.67725344251,
111.174812009905,111.6723705773,112.169929144694,112.667487712089,113.165046279484,
113.662604846878,114.160163414273,114.657721981668,115.155280549062,115.652839116457,
116.150397683852,116.647956251246,117.145514818641,117.643073386036,118.14063195343,
118.638190520825,119.13574908822,119.633307655614,120.130866223009,120.628424790404,
121.125983357798,121.623541925193,122.121100492588,122.618659059982,123.116217627377,
123.613776194772,124.111334762166,124.608893329561,125.106451896956,125.60401046435,
126.101569031745,126.59912759914,127.096686166534,127.594244733929,128.091803301324,
128.589361868718,129.086920436113,129.584479003508,130.082037570902,130.579596138297,
131.077154705692,131.574713273087,132.072271840481,132.569830407876,133.067388975271,
133.564947542665,134.06250611006,134.560064677455,135.057623244849,135.555181812244,
136.052740379639,136.550298947033,137.047857514428,137.545416081823,138.042974649217,
138.540533216612,139.038091784007,139.535650351401,140.033208918796,140.530767486191,
141.028326053585,141.52588462098,142.023443188375,142.521001755769,143.018560323164,
143.516118890559,144.013677457953,144.511236025348,145.008794592743,145.506353160137,
146.003911727532,146.501470294927,146.999028862321,147.496587429716,147.994145997111,
148.491704564505,148.9892631319,149.486821699295,149.984380266689,150.481938834084,
150.979497401479,151.477055968873,151.974614536268,152.472173103663,152.969731671057,
153.467290238452,153.964848805847,154.462407373241,154.959965940636,155.457524508031,
155.955083075425,156.45264164282,156.950200210215,157.447758777609,157.945317345004,
158.442875912399,158.940434479793,159.437993047188,159.935551614583,160.433110181977,
160.930668749372,161.428227316767,161.925785884161,162.423344451556,162.920903018951,
163.418461586346,163.91602015374,164.413578721135,164.91113728853,165.408695855924,
165.906254423319,166.403812990714,166.901371558108,167.398930125503,167.896488692898,
168.394047260292,168.891605827687,169.389164395082,169.886722962476,170.384281529871,
170.881840097266,171.37939866466,171.876957232055,172.37451579945,172.872074366844,
173.369632934239,173.867191501634,174.364750069028,174.862308636423,175.359867203818,
175.857425771212,176.354984338607,176.852542906002,177.350101473396,177.847660040791,
178.345218608186,178.84277717558,179.340335742975,179.83789431037,180.335452877764,
180.833011445159,181.330570012554,181.828128579948,182.325687147343,182.823245714738,
183.320804282132,183.818362849527,184.315921416922,184.813479984316,185.311038551711,
185.808597119106,186.3061556865,186.803714253895,187.30127282129,187.798831388684,
188.296389956079,188.793948523474,189.291507090868,189.789065658263,190.286624225658,
190.784182793052,191.281741360447,191.779299927842,192.276858495236,192.774417062631,
193.271975630026,193.76953419742),.UNSPECIFIED.);
#289=B_SPLINE_SURFACE_WITH_KNOTS('',3,3,((#71137,#71138,#71139,#71140,#71141,
#71142),(#71143,#71144,#71145,#71146,#71147,#71148),(#71149,#71150,#71151,
#71152,#71153,#71154),(#71155,#71156,#71157,#71158,#71159,#71160)),
 .UNSPECIFIED.,.F.,.F.,.F.,(4,4),(4,1,1,4),(0.,1.),(0.111993552465714,0.578527205932438,
0.889549641576921,1.2005720772214),.UNSPECIFIED.);
#290=B_SPLINE_SURFACE_WITH_KNOTS('',3,3,((#71191,#71192,#71193,#71194,#71195,
#71196),(#71197,#71198,#71199,#71200,#71201,#71202),(#71203,#71204,#71205,
#71206,#71207,#71208),(#71209,#71210,#71211,#71212,#71213,#71214)),
 .UNSPECIFIED.,.F.,.F.,.F.,(4,4),(4,1,1,4),(0.,1.),(0.111993552465714,0.578527205932438,
0.889549641576921,1.2005720772214),.UNSPECIFIED.);
#291=B_SPLINE_SURFACE_WITH_KNOTS('',3,3,((#71285,#71286,#71287,#71288,#71289,
#71290),(#71291,#71292,#71293,#71294,#71295,#71296),(#71297,#71298,#71299,
#71300,#71301,#71302),(#71303,#71304,#71305,#71306,#71307,#71308)),
 .UNSPECIFIED.,.F.,.F.,.F.,(4,4),(4,1,1,4),(0.,1.),(0.111993552465713,0.423015988110196,
0.734038423754679,1.2005720772214),.UNSPECIFIED.);
#292=B_SPLINE_SURFACE_WITH_KNOTS('',3,3,((#71437,#71438,#71439,#71440,#71441,
#71442),(#71443,#71444,#71445,#71446,#71447,#71448),(#71449,#71450,#71451,
#71452,#71453,#71454),(#71455,#71456,#71457,#71458,#71459,#71460)),
 .UNSPECIFIED.,.F.,.F.,.F.,(4,4),(4,1,1,4),(0.,1.),(0.111993552465714,0.423015988110197,
0.73403842375468,1.2005720772214),.UNSPECIFIED.);
#293=B_SPLINE_SURFACE_WITH_KNOTS('',3,3,((#71470,#71471,#71472,#71473,#71474,
#71475),(#71476,#71477,#71478,#71479,#71480,#71481),(#71482,#71483,#71484,
#71485,#71486,#71487),(#71488,#71489,#71490,#71491,#71492,#71493)),
 .UNSPECIFIED.,.F.,.F.,.F.,(4,4),(4,1,1,4),(0.,1.),(0.111993552465714,0.578527205932439,
0.889549641576922,1.20057207722141),.UNSPECIFIED.);
#294=B_SPLINE_SURFACE_WITH_KNOTS('',3,3,((#71506,#71507,#71508,#71509,#71510,
#71511),(#71512,#71513,#71514,#71515,#71516,#71517),(#71518,#71519,#71520,
#71521,#71522,#71523),(#71524,#71525,#71526,#71527,#71528,#71529)),
 .UNSPECIFIED.,.F.,.F.,.F.,(4,4),(4,1,1,4),(0.,1.),(0.111993552465714,0.578527205932438,
0.889549641576921,1.2005720772214),.UNSPECIFIED.);
#295=SHAPE_REPRESENTATION_RELATIONSHIP('SRR','None',#71683,#308);
#296=SHAPE_REPRESENTATION_RELATIONSHIP('SRR','None',#71684,#309);
#297=SHAPE_REPRESENTATION_RELATIONSHIP('SRR','None',#71685,#310);
#298=SHAPE_REPRESENTATION_RELATIONSHIP('SRR','None',#71686,#311);
#299=SHAPE_REPRESENTATION_RELATIONSHIP('SRR','None',#71687,#312);
#300=SHAPE_REPRESENTATION_RELATIONSHIP('SRR','None',#71688,#313);
#301=SHAPE_REPRESENTATION_RELATIONSHIP('SRR','None',#71689,#314);
#302=SHAPE_REPRESENTATION_RELATIONSHIP('SRR','None',#71690,#315);
#303=SHAPE_REPRESENTATION_RELATIONSHIP('SRR','None',#71691,#316);
#304=SHAPE_REPRESENTATION_RELATIONSHIP('SRR','None',#71692,#317);
#305=SHAPE_REPRESENTATION_RELATIONSHIP('SRR','None',#71693,#318);
#306=SHAPE_REPRESENTATION_RELATIONSHIP('SRR','None',#71694,#319);
#307=SHAPE_REPRESENTATION_RELATIONSHIP('SRR','None',#71695,#320);
#308=ADVANCED_BREP_SHAPE_REPRESENTATION('',(#334),#71615);
#309=ADVANCED_BREP_SHAPE_REPRESENTATION('',(#335),#71616);
#310=ADVANCED_BREP_SHAPE_REPRESENTATION('',(#336),#71617);
#311=ADVANCED_BREP_SHAPE_REPRESENTATION('',(#337),#71618);
#312=ADVANCED_BREP_SHAPE_REPRESENTATION('',(#338),#71619);
#313=ADVANCED_BREP_SHAPE_REPRESENTATION('',(#339),#71620);
#314=ADVANCED_BREP_SHAPE_REPRESENTATION('',(#340),#71621);
#315=ADVANCED_BREP_SHAPE_REPRESENTATION('',(#341),#71622);
#316=ADVANCED_BREP_SHAPE_REPRESENTATION('',(#342),#71623);
#317=ADVANCED_BREP_SHAPE_REPRESENTATION('',(#343),#71624);
#318=ADVANCED_BREP_SHAPE_REPRESENTATION('',(#344),#71625);
#319=ADVANCED_BREP_SHAPE_REPRESENTATION('',(#345),#71626);
#320=ADVANCED_BREP_SHAPE_REPRESENTATION('',(#346),#71627);
#321=STYLED_ITEM('',(#71804),#334);
#322=STYLED_ITEM('',(#71804),#335);
#323=STYLED_ITEM('',(#71825),#336);
#324=STYLED_ITEM('',(#71818),#337);
#325=STYLED_ITEM('',(#71818),#338);
#326=STYLED_ITEM('',(#71818),#339);
#327=STYLED_ITEM('',(#71818),#340);
#328=STYLED_ITEM('',(#71825),#341);
#329=STYLED_ITEM('',(#71825),#342);
#330=STYLED_ITEM('',(#71818),#343);
#331=STYLED_ITEM('',(#71832),#344);
#332=STYLED_ITEM('',(#71825),#345);
#333=STYLED_ITEM('',(#71825),#346);
#334=MANIFOLD_SOLID_BREP('Body1',#34208);
#335=MANIFOLD_SOLID_BREP('Body1',#34209);
#336=MANIFOLD_SOLID_BREP('Body1',#34210);
#337=MANIFOLD_SOLID_BREP('Body1',#34211);
#338=MANIFOLD_SOLID_BREP('Body1',#34212);
#339=MANIFOLD_SOLID_BREP('Body1',#34213);
#340=MANIFOLD_SOLID_BREP('Body1',#34214);
#341=MANIFOLD_SOLID_BREP('Body1',#34215);
#342=MANIFOLD_SOLID_BREP('Body1',#34216);
#343=MANIFOLD_SOLID_BREP('Body1',#34217);
#344=MANIFOLD_SOLID_BREP('Body1',#34218);
#345=MANIFOLD_SOLID_BREP('Body1',#34219);
#346=MANIFOLD_SOLID_BREP('Body1',#34220);
#347=B_SPLINE_CURVE_WITH_KNOTS('',3,(#48590,#48591,#48592,#48593),
 .UNSPECIFIED.,.F.,.F.,(4,4),(-0.0954037219784117,0.),.UNSPECIFIED.);
#348=B_SPLINE_CURVE_WITH_KNOTS('',3,(#48596,#48597,#48598,#48599),
 .UNSPECIFIED.,.F.,.F.,(4,4),(-0.0954037219783748,0.),.UNSPECIFIED.);
#349=B_SPLINE_CURVE_WITH_KNOTS('',3,(#48604,#48605,#48606,#48607),
 .UNSPECIFIED.,.F.,.F.,(4,4),(-0.0954037219783863,0.),.UNSPECIFIED.);
#350=B_SPLINE_CURVE_WITH_KNOTS('',3,(#48613,#48614,#48615,#48616),
 .UNSPECIFIED.,.F.,.F.,(4,4),(-0.0954037219782671,0.),.UNSPECIFIED.);
#351=B_SPLINE_CURVE_WITH_KNOTS('',3,(#48622,#48623,#48624,#48625),
 .UNSPECIFIED.,.F.,.F.,(4,4),(-0.0954037219784872,0.),.UNSPECIFIED.);
#352=B_SPLINE_CURVE_WITH_KNOTS('',3,(#48631,#48632,#48633,#48634),
 .UNSPECIFIED.,.F.,.F.,(4,4),(-0.0954037219781768,0.),.UNSPECIFIED.);
#353=B_SPLINE_CURVE_WITH_KNOTS('',3,(#48640,#48641,#48642,#48643),
 .UNSPECIFIED.,.F.,.F.,(4,4),(-0.0954037219782904,0.),.UNSPECIFIED.);
#354=B_SPLINE_CURVE_WITH_KNOTS('',3,(#48650,#48651,#48652,#48653),
 .UNSPECIFIED.,.F.,.F.,(4,4),(-0.0954037219784109,0.),.UNSPECIFIED.);
#355=B_SPLINE_CURVE_WITH_KNOTS('',3,(#48659,#48660,#48661,#48662),
 .UNSPECIFIED.,.F.,.F.,(4,4),(-0.0954037219783438,0.),.UNSPECIFIED.);
#356=B_SPLINE_CURVE_WITH_KNOTS('',3,(#48668,#48669,#48670,#48671),
 .UNSPECIFIED.,.F.,.F.,(4,4),(-0.0954037219783345,0.),.UNSPECIFIED.);
#357=B_SPLINE_CURVE_WITH_KNOTS('',3,(#52958,#52959,#52960,#52961,#52962,
#52963,#52964,#52965,#52966,#52967,#52968,#52969,#52970),.UNSPECIFIED.,
 .F.,.F.,(4,1,1,1,1,1,1,1,1,1,4),(47.1238898038469,47.3708199277661,47.8600810904219,
48.3493422530777,48.8386034157334,49.3278645783892,49.817125741045,50.3063869037007,
50.7956480663565,51.2849092290123,51.6964060964814),.UNSPECIFIED.);
#358=B_SPLINE_CURVE_WITH_KNOTS('',3,(#52972,#52973,#52974,#52975),
 .UNSPECIFIED.,.F.,.F.,(4,4),(0.11224113270863,0.157354351022216),
 .UNSPECIFIED.);
#359=B_SPLINE_CURVE_WITH_KNOTS('',3,(#52977,#52978,#52979,#52980,#52981,
#52982,#52983,#52984,#52985),.UNSPECIFIED.,.F.,.F.,(4,1,1,1,1,1,4),(48.7821842940486,
49.4244050727166,49.7455154620506,50.0666258513846,50.7088466300525,51.0299570193865,
51.6721777980545),.UNSPECIFIED.);
#360=B_SPLINE_CURVE_WITH_KNOTS('',3,(#52987,#52988,#52989,#52990,#52991,
#52992),.UNSPECIFIED.,.F.,.F.,(4,2,4),(0.997055295420078,1.08014136000988,
1.09793883659407),.UNSPECIFIED.);
#361=B_SPLINE_CURVE_WITH_KNOTS('',3,(#52994,#52995,#52996,#52997,#52998,
#52999),.UNSPECIFIED.,.F.,.F.,(4,2,4),(0.906540457062692,0.913969230830279,
0.997055295420078),.UNSPECIFIED.);
#362=B_SPLINE_CURVE_WITH_KNOTS('',3,(#53000,#53001,#53002,#53003,#53004,
#53005,#53006),.UNSPECIFIED.,.F.,.F.,(4,1,1,1,4),(47.1238898038469,47.1409299185258,
47.6325247499845,48.1241195814432,48.6157144129018),.UNSPECIFIED.);
#363=B_SPLINE_CURVE_WITH_KNOTS('',3,(#53011,#53012,#53013,#53014,#53015,
#53016,#53017,#53018,#53019,#53020,#53021,#53022,#53023,#53024,#53025,#53026,
#53027),.UNSPECIFIED.,.F.,.F.,(4,1,1,1,1,1,1,1,1,1,1,1,1,1,4),(40.8407044966673,
41.0104248132411,41.4996859758969,41.9889471385527,42.4782083012084,42.9674694638642,
43.45673062652,43.9459917891757,44.4352529518315,44.9245141144873,45.413775277143,
45.9030364397988,46.3922976024546,46.8815587651103,47.1238898038469),
 .UNSPECIFIED.);
#364=B_SPLINE_CURVE_WITH_KNOTS('',3,(#53028,#53029,#53030,#53031,#53032,
#53033,#53034,#53035,#53036,#53037,#53038,#53039,#53040,#53041,#53042,#53043),
 .UNSPECIFIED.,.F.,.F.,(4,1,1,1,1,1,1,1,1,1,1,1,1,4),(40.8407044966673,
41.2417919410218,41.7333867724805,42.2249816039391,42.7165764353978,43.2081712668565,
43.6997660983151,44.1913609297738,44.6829557612325,45.1745505926911,45.6661454241498,
46.1577402556085,46.6493350870672,47.1238898038469),.UNSPECIFIED.);
#365=B_SPLINE_CURVE_WITH_KNOTS('',3,(#53048,#53049,#53050,#53051,#53052,
#53053,#53054,#53055,#53056,#53057,#53058,#53059,#53060,#53061,#53062,#53063,
#53064),.UNSPECIFIED.,.F.,.F.,(4,1,1,1,1,1,1,1,1,1,1,1,1,1,4),(34.5575191894877,
34.6500296987161,35.1392908613719,35.6285520240277,36.1178131866834,36.6070743493392,
37.096335511995,37.5855966746507,38.0748578373065,38.5641189999623,39.053380162618,
39.5426413252738,40.0319024879296,40.5211636505854,40.8407044966673),
 .UNSPECIFIED.);
#366=B_SPLINE_CURVE_WITH_KNOTS('',3,(#53065,#53066,#53067,#53068,#53069,
#53070,#53071,#53072,#53073,#53074,#53075,#53076,#53077,#53078,#53079,#53080,
#53081),.UNSPECIFIED.,.F.,.F.,(4,1,1,1,1,1,1,1,1,1,1,1,1,1,4),(34.5575191894877,
34.8510591320591,35.3426539635178,35.8342487949764,36.3258436264351,36.8174384578938,
37.3090332893524,37.8006281208111,38.2922229522698,38.7838177837285,39.2754126151871,
39.7670074466458,40.2586022781045,40.7501971095631,40.8407044966673),
 .UNSPECIFIED.);
#367=B_SPLINE_CURVE_WITH_KNOTS('',3,(#53086,#53087,#53088,#53089,#53090,
#53091,#53092,#53093,#53094,#53095,#53096,#53097,#53098,#53099,#53100,#53101,
#53102),.UNSPECIFIED.,.F.,.F.,(4,1,1,1,1,1,1,1,1,1,1,1,1,1,4),(28.2743338823081,
28.2896345841911,28.7788957468469,29.2681569095027,29.7574180721584,30.2466792348142,
30.73594039747,31.2252015601257,31.7144627227815,32.2037238854373,32.692985048093,
33.1822462107488,33.6715073734046,34.1607685360603,34.5575191894877),
 .UNSPECIFIED.);
#368=B_SPLINE_CURVE_WITH_KNOTS('',3,(#53103,#53104,#53105,#53106,#53107,
#53108,#53109,#53110,#53111,#53112,#53113,#53114,#53115,#53116,#53117,#53118,
#53119),.UNSPECIFIED.,.F.,.F.,(4,1,1,1,1,1,1,1,1,1,1,1,1,1,4),(28.2743338823081,
28.4603263230964,28.9519211545551,29.4435159860138,29.9351108174724,30.4267056489311,
30.9183004803898,31.4098953118484,31.9014901433071,32.3930849747658,32.8846798062244,
33.3762746376831,33.8678694691418,34.3594643006004,34.5575191894877),
 .UNSPECIFIED.);
#369=B_SPLINE_CURVE_WITH_KNOTS('',3,(#53124,#53125,#53126,#53127,#53128,
#53129,#53130,#53131,#53132,#53133,#53134,#53135,#53136,#53137,#53138,#53139),
 .UNSPECIFIED.,.F.,.F.,(4,1,1,1,1,1,1,1,1,1,1,1,1,4),(21.9911485751285,
22.4185006323219,22.9077617949777,23.3970229576334,23.8862841202892,24.375545282945,
24.8648064456007,25.3540676082565,25.8433287709123,26.332589933568,26.8218510962238,
27.3111122588796,27.8003734215353,28.2743338823081),.UNSPECIFIED.);
#370=B_SPLINE_CURVE_WITH_KNOTS('',3,(#53140,#53141,#53142,#53143,#53144,
#53145,#53146,#53147,#53148,#53149,#53150,#53151,#53152,#53153,#53154,#53155,
#53156),.UNSPECIFIED.,.F.,.F.,(4,1,1,1,1,1,1,1,1,1,1,1,1,1,4),(21.9911485751285,
22.0695935141337,22.5611883455924,23.0527831770511,23.5443780085097,24.0359728399684,
24.5275676714271,25.0191625028857,25.5107573343444,26.0023521658031,26.4939469972617,
26.9855418287204,27.4771366601791,27.9687314916377,28.2743338823081),
 .UNSPECIFIED.);
#371=B_SPLINE_CURVE_WITH_KNOTS('',3,(#53161,#53162,#53163,#53164,#53165,
#53166,#53167,#53168,#53169,#53170,#53171,#53172,#53173,#53174,#53175,#53176,
#53177),.UNSPECIFIED.,.F.,.F.,(4,1,1,1,1,1,1,1,1,1,1,1,1,1,4),(15.707963267949,
16.0581055177969,16.5473666804527,17.0366278431084,17.5258890057642,18.01515016842,
18.5044113310757,18.9936724937315,19.4829336563873,19.972194819043,20.4614559816988,
20.9507171443546,21.4399783070103,21.9292394696661,21.9911485751285),
 .UNSPECIFIED.);
#372=B_SPLINE_CURVE_WITH_KNOTS('',3,(#53178,#53179,#53180,#53181,#53182,
#53183,#53184,#53185,#53186,#53187,#53188,#53189,#53190,#53191,#53192,#53193),
 .UNSPECIFIED.,.F.,.F.,(4,1,1,1,1,1,1,1,1,1,1,1,1,4),(15.7079632679489,
16.1704555366297,16.6620503680884,17.153645199547,17.6452400310057,18.1368348624644,
18.628429693923,19.1200245253817,19.6116193568404,20.103214188299,20.5948090197577,
21.0864038512164,21.5779986826751,21.9911485751285),.UNSPECIFIED.);
#373=B_SPLINE_CURVE_WITH_KNOTS('',3,(#53199,#53200,#53201,#53202,#53203,
#53204,#53205,#53206,#53207,#53208,#53209,#53210,#53211,#53212,#53213),
 .UNSPECIFIED.,.F.,.F.,(4,1,1,1,1,1,1,1,1,1,1,1,4),(78.5398163397448,78.7810244064439,
79.2760369931915,79.7710495799391,80.2660621666867,80.7610747534343,81.2560873401819,
81.7510999269296,82.2461125136772,82.7411251004248,83.2361376871724,83.73115027392,
84.1747579197157),.UNSPECIFIED.);
#374=B_SPLINE_CURVE_WITH_KNOTS('',3,(#53216,#53217,#53218,#53219,#53220,
#53221,#53222,#53223,#53224,#53225,#53226,#53227),.UNSPECIFIED.,.F.,.F.,
(4,1,1,1,1,1,1,1,1,4),(78.5398163397448,78.9342340329046,79.4245043271733,
79.9147746214419,80.4050449157106,80.8953152099793,81.385585504248,81.8758557985167,
82.3661260927854,82.856396387054),.UNSPECIFIED.);
#375=B_SPLINE_CURVE_WITH_KNOTS('',3,(#53232,#53233,#53234,#53235,#53236,
#53237,#53238,#53239,#53240,#53241,#53242,#53243,#53244,#53245,#53246,#53247,
#53248),.UNSPECIFIED.,.F.,.F.,(4,1,1,1,1,1,1,1,1,1,1,1,1,1,4),(72.2566310325653,
72.3458607787251,72.8408733654727,73.3358859522203,73.8308985389679,74.3259111257155,
74.8209237124631,75.3159362992107,75.8109488859583,76.3059614727059,76.8009740594535,
77.2959866462011,77.7909992329487,78.2860118196963,78.5398163397448),
 .UNSPECIFIED.);
#376=B_SPLINE_CURVE_WITH_KNOTS('',3,(#53249,#53250,#53251,#53252,#53253,
#53254,#53255,#53256,#53257,#53258,#53259,#53260,#53261,#53262,#53263,#53264,
#53265),.UNSPECIFIED.,.F.,.F.,(4,1,1,1,1,1,1,1,1,1,1,1,1,1,4),(72.2566310325653,
72.5607202074117,73.0509905016804,73.5412607959491,74.0315310902178,74.5218013844865,
75.0120716787551,75.5023419730238,75.9926122672925,76.4828825615612,76.9731528558299,
77.4634231500985,77.9536934443672,78.4439637386359,78.5398163397448),
 .UNSPECIFIED.);
#377=B_SPLINE_CURVE_WITH_KNOTS('',3,(#53270,#53271,#53272,#53273,#53274,
#53275,#53276,#53277,#53278,#53279,#53280,#53281,#53282,#53283,#53284,#53285),
 .UNSPECIFIED.,.F.,.F.,(4,1,1,1,1,1,1,1,1,1,1,1,1,4),(65.9734457253856,
66.4057097377538,66.9007223245014,67.3957349112491,67.8907474979967,68.3857600847443,
68.8807726714919,69.3757852582395,69.8707978449871,70.3658104317347,70.8608230184823,
71.3558356052299,71.8508481919775,72.2566310325653),.UNSPECIFIED.);
#378=B_SPLINE_CURVE_WITH_KNOTS('',3,(#53286,#53287,#53288,#53289,#53290,
#53291,#53292,#53293,#53294,#53295,#53296,#53297,#53298,#53299,#53300,#53301,
#53302),.UNSPECIFIED.,.F.,.F.,(4,1,1,1,1,1,1,1,1,1,1,1,1,1,4),(65.9734457253856,
66.1872063819189,66.6774766761876,67.1677469704563,67.6580172647249,68.1482875589936,
68.6385578532623,69.128828147531,69.6190984417997,70.1093687360683,70.599639030337,
71.0899093246057,71.5801796188744,72.0704499131431,72.2566310325653),
 .UNSPECIFIED.);
#379=B_SPLINE_CURVE_WITH_KNOTS('',3,(#53645,#53646,#53647,#53648,#53649,
#53650,#53651,#53652,#53653,#53654,#53655,#53656,#53657,#53658,#53659,#53660),
 .UNSPECIFIED.,.F.,.F.,(4,3,3,3,3,4),(0.,0.000595938657993939,0.0422635503527143,
0.0630916558022166,0.101044021572731,0.126729429815141),.UNSPECIFIED.);
#380=B_SPLINE_CURVE_WITH_KNOTS('',3,(#53662,#53663,#53664,#53665,#53666,
#53667,#53668,#53669,#53670),.UNSPECIFIED.,.F.,.F.,(4,1,1,1,1,1,4),(58.2972797775322,
58.586820436873,59.2476946594652,59.5781317707613,60.2390059933534,60.8998802159456,
61.1317270633727),.UNSPECIFIED.);
#381=B_SPLINE_CURVE_WITH_KNOTS('',3,(#53672,#53673,#53674,#53675,#53676,
#53677,#53678,#53679,#53680,#53681),.UNSPECIFIED.,.F.,.F.,(4,2,2,2,4),(0.000574071133364476,
0.000967589686564383,0.0339148109550191,0.0832234192490246,0.162484616113956),
 .UNSPECIFIED.);
#382=B_SPLINE_CURVE_WITH_KNOTS('',3,(#53683,#53684,#53685,#53686,#53687,
#53688,#53689,#53690,#53691,#53692,#53693,#53694,#53695),.UNSPECIFIED.,
 .F.,.F.,(4,3,3,3,4),(0.,0.00275985983460007,0.0770052601636086,0.109906700875405,
0.130628524523904),.UNSPECIFIED.);
#383=B_SPLINE_CURVE_WITH_KNOTS('',3,(#53696,#53697,#53698,#53699,#53700,
#53701,#53702,#53703,#53704,#53705,#53706,#53707,#53708,#53709,#53710,#53711,
#53712,#53713,#53714),.UNSPECIFIED.,.F.,.F.,(4,3,3,3,3,3,4),(49.9514450922859,
50.281882203582,50.9427564261742,51.2731935374703,51.9340677600624,52.5949419826546,
52.8217841885201),.UNSPECIFIED.);
#384=B_SPLINE_CURVE_WITH_KNOTS('',3,(#53905,#53906,#53907,#53908,#53909,
#53910,#53911,#53912,#53913,#53914,#53915,#53916,#53917,#53918,#53919,#53920,
#53921,#53922,#53923,#53924,#53925,#53926,#53927,#53928,#53929,#53930,#53931,
#53932,#53933,#53934,#53935,#53936,#53937,#53938,#53939,#53940,#53941,#53942,
#53943,#53944,#53945,#53946,#53947,#53948,#53949,#53950),.UNSPECIFIED.,
 .F.,.F.,(4,3,3,3,3,3,3,3,3,3,3,3,3,3,3,4),(0.,0.00275985982614405,0.0773717195497823,
0.109906700365477,0.16313770113851,0.167106859846252,0.168197417803669,
0.168838059532748,0.169391172021586,0.170064784109231,0.171335649429611,
0.178574548147706,0.187829968841971,0.233407245541387,0.305551783846953,
0.338436359320456),.UNSPECIFIED.);
#385=B_SPLINE_CURVE_WITH_KNOTS('',3,(#53952,#53953,#53954,#53955,#53956,
#53957,#53958,#53959,#53960,#53961,#53962,#53963,#53964,#53965,#53966,#53967,
#53968,#53969,#53970,#53971,#53972,#53973,#53974,#53975,#53976,#53977,#53978,
#53979,#53980,#53981,#53982,#53983,#53984,#53985,#53986,#53987,#53988,#53989,
#53990,#53991,#53992,#53993,#53994),.UNSPECIFIED.,.F.,.F.,(4,3,3,3,3,3,
3,3,3,3,3,3,3,3,4),(65.6568234492589,65.7265928569268,66.2168631511955,
66.7071334454641,67.1974037397328,67.6876740340015,68.1779443282702,68.6682146225388,
69.1584849168075,69.6487552110762,70.1390255053449,70.6292957996136,71.1195660938823,
71.6098363881509,71.6713401100588),.UNSPECIFIED.);
#386=B_SPLINE_CURVE_WITH_KNOTS('',3,(#53996,#53997,#53998,#53999,#54000,
#54001,#54002,#54003,#54004,#54005,#54006,#54007,#54008,#54009,#54010,#54011,
#54012,#54013,#54014,#54015,#54016,#54017,#54018,#54019,#54020,#54021,#54022,
#54023,#54024,#54025,#54026,#54027,#54028,#54029,#54030,#54031,#54032,#54033,
#54034,#54035,#54036,#54037,#54038,#54039,#54040,#54041),.UNSPECIFIED.,
 .F.,.F.,(4,3,3,3,3,3,3,3,3,3,3,3,3,3,3,4),(0.,0.00275985982151374,0.0771562456781327,
0.109906700101125,0.163137700733035,0.1671068594303,0.168197417389794,0.168838059129582,
0.169391171634666,0.170064783742003,0.17133564910631,0.178574548151433,
0.187829969232375,0.233407247858854,0.305703464500967,0.338436366447218),
 .UNSPECIFIED.);
#387=B_SPLINE_CURVE_WITH_KNOTS('',3,(#54043,#54044,#54045,#54046,#54047,
#54048,#54049,#54050,#54051,#54052,#54053,#54054,#54055,#54056,#54057,#54058,
#54059,#54060,#54061,#54062,#54063,#54064,#54065,#54066,#54067,#54068,#54069,
#54070,#54071,#54072,#54073,#54074,#54075,#54076,#54077,#54078,#54079,#54080,
#54081,#54082),.UNSPECIFIED.,.F.,.F.,(4,3,3,3,3,3,3,3,3,3,3,3,3,4),(59.3736381420792,
59.8433493257026,60.3336196199713,60.82388991424,61.3141602085087,61.8044305027773,
62.294700797046,62.7849710913147,63.2752413855834,63.7655116798521,64.2557819741207,
64.7460522683894,65.2363225626581,65.3881548028793),.UNSPECIFIED.);
#388=B_SPLINE_CURVE_WITH_KNOTS('',3,(#54084,#54085,#54086,#54087,#54088,
#54089,#54090,#54091,#54092,#54093,#54094,#54095,#54096,#54097,#54098,#54099,
#54100,#54101,#54102,#54103,#54104,#54105,#54106,#54107,#54108,#54109,#54110,
#54111,#54112,#54113,#54114,#54115,#54116,#54117,#54118,#54119,#54120,#54121,
#54122,#54123,#54124,#54125,#54126,#54127,#54128,#54129,#54130,#54131,#54132),
 .UNSPECIFIED.,.F.,.F.,(4,3,3,3,3,3,3,3,3,3,3,3,3,3,3,3,4),(0.,0.00275985983466315,
0.0768512497472772,0.109906700870624,0.163137701889579,0.167106860614449,
0.168197418582742,0.168838060333893,0.169391172850375,0.170064784950834,
0.171335650271267,0.178574549075021,0.187829969490077,0.233407245213584,
0.306223710050725,0.312212167181286,0.338436362006313),.UNSPECIFIED.);
#389=B_SPLINE_CURVE_WITH_KNOTS('',3,(#54134,#54135,#54136,#54137,#54138,
#54139,#54140,#54141,#54142,#54143,#54144,#54145,#54146,#54147,#54148,#54149,
#54150,#54151,#54152,#54153,#54154,#54155,#54156,#54157,#54158,#54159,#54160,
#54161,#54162,#54163,#54164,#54165,#54166,#54167,#54168,#54169,#54170,#54171,
#54172,#54173),.UNSPECIFIED.,.F.,.F.,(4,3,3,3,3,3,3,3,3,3,3,3,3,4),(53.0904528348997,
53.4698355002098,53.9601057944785,54.4503760887471,54.9406463830158,55.4309166772845,
55.9211869715532,56.4114572658219,56.9017275600905,57.3919978543592,57.8822681486279,
58.3725384428966,58.8628087371653,59.1049694956997),.UNSPECIFIED.);
#390=B_SPLINE_CURVE_WITH_KNOTS('',3,(#54175,#54176,#54177,#54178,#54179,
#54180,#54181,#54182,#54183,#54184),.UNSPECIFIED.,.F.,.F.,(4,3,3,4),(0.198401836072916,
0.23340724983945,0.304766656516156,0.338436371365031),.UNSPECIFIED.);
#391=B_SPLINE_CURVE_WITH_KNOTS('',3,(#54186,#54187,#54188,#54189,#54190,
#54191,#54192,#54193,#54194,#54195),.UNSPECIFIED.,.F.,.F.,(4,2,2,2,4),(0.,
0.00656666019327175,0.0703003168502551,0.107768285611947,0.160871499936812),
 .UNSPECIFIED.);
#392=B_SPLINE_CURVE_WITH_KNOTS('',3,(#54196,#54197,#54198,#54199,#54200,
#54201,#54202,#54203,#54204,#54205,#54206,#54207,#54208),.UNSPECIFIED.,
 .F.,.F.,(4,1,1,1,1,1,1,1,1,1,4),(61.3832284283791,61.7747737335008,62.2650440277695,
62.7553143220381,63.2455846163068,63.7358549105755,64.2261252048442,64.7163954991129,
65.2066657933815,65.6969360876502,65.9734457253856),.UNSPECIFIED.);
#393=B_SPLINE_CURVE_WITH_KNOTS('',3,(#54210,#54211,#54212,#54213,#54214,
#54215,#54216,#54217,#54218,#54219,#54220,#54221,#54222,#54223,#54224,#54225,
#54226,#54227,#54228,#54229,#54230,#54231,#54232,#54233,#54234,#54235,#54236,
#54237,#54238,#54239,#54240,#54241,#54242,#54243,#54244,#54245,#54246,#54247,
#54248,#54249,#54250,#54251,#54252,#54253,#54254,#54255,#54256,#54257,#54258,
#54259,#54260,#54261,#54262,#54263,#54264,#54265,#54266,#54267,#54268,#54269,
#54270,#54271,#54272,#54273,#54274,#54275,#54276,#54277,#54278,#54279,#54280,
#54281,#54282,#54283,#54284,#54285,#54286,#54287,#54288,#54289,#54290,#54291,
#54292,#54293,#54294,#54295,#54296,#54297,#54298,#54299,#54300,#54301,#54302,
#54303,#54304,#54305,#54306,#54307,#54308,#54309,#54310,#54311,#54312,#54313,
#54314,#54315,#54316,#54317,#54318,#54319,#54320,#54321,#54322,#54323,#54324,
#54325,#54326,#54327,#54328,#54329,#54330,#54331,#54332,#54333),
 .UNSPECIFIED.,.F.,.F.,(4,3,3,3,3,3,3,3,3,3,3,3,3,3,3,3,3,3,3,3,3,3,3,3,
3,3,3,3,3,3,3,3,3,3,3,3,3,3,3,3,3,4),(-2.4657711816956,-2.37711779550954,
-2.28851752377278,-2.22320398650821,-2.18602278417013,-2.17028473161443,
-2.15866200237192,-2.07068230873769,-1.98294419157819,-1.89589333530891,
-1.87402539857354,-1.86347823865937,-1.77633674922564,-1.76600922565624,
-1.67904910353692,-1.591716101066,-1.50460771625274,-1.41982386317424,-1.39830915580724,
-1.38520554468227,-1.29903699636726,-1.21307297743482,-1.16547230393873,
-1.07917498089865,-0.993139567163436,-0.941084428724779,-0.925274659028494,
-0.913998245978635,-0.828843082626024,-0.743624729749914,-0.659209653948047,
-0.576698459654186,-0.504611152197413,-0.473072955185075,-0.459906411912699,
-0.450573022198668,-0.366966623021441,-0.282778978986007,-0.198778607846025,
-0.115420401362767,-0.0335266982944923,0.),.UNSPECIFIED.);
#394=B_SPLINE_CURVE_WITH_KNOTS('',3,(#54334,#54335,#54336,#54337,#54338,
#54339,#54340),.UNSPECIFIED.,.F.,.F.,(4,3,4),(71.9400087564384,72.1001066824196,
72.5200028658207),.UNSPECIFIED.);
#395=B_SPLINE_CURVE_WITH_KNOTS('',3,(#54683,#54684,#54685,#54686,#54687,
#54688,#54689,#54690,#54691,#54692,#54693,#54694,#54695,#54696,#54697,#54698,
#54699,#54700,#54701,#54702,#54703,#54704,#54705,#54706,#54707,#54708,#54709,
#54710,#54711,#54712,#54713,#54714,#54715,#54716,#54717,#54718,#54719,#54720,
#54721,#54722,#54723,#54724,#54725,#54726,#54727,#54728),.UNSPECIFIED.,
 .F.,.F.,(4,3,3,3,3,3,3,3,3,3,3,3,3,3,3,4),(0.,0.00275985982436321,0.0772952705909694,
0.109906700261339,0.163137700981914,0.167106859688835,0.168197417644868,
0.168838059371253,0.169391171859311,0.170064783946173,0.171335649280755,
0.178574548125793,0.187829969035857,0.233407246747053,0.305622875587664,
0.338436362095157),.UNSPECIFIED.);
#396=B_SPLINE_CURVE_WITH_KNOTS('',3,(#54730,#54731,#54732,#54733,#54734,
#54735,#54736,#54737,#54738,#54739,#54740,#54741,#54742,#54743,#54744,#54745,
#54746,#54747,#54748),.UNSPECIFIED.,.F.,.F.,(4,3,3,3,3,3,4),(0.,0.491594831458664,
0.983189662917332,1.474784494376,1.96637932583467,2.45797415729334,2.55630173108341),
 .UNSPECIFIED.);
#397=B_SPLINE_CURVE_WITH_KNOTS('',3,(#54750,#54751,#54752,#54753,#54754,
#54755,#54756,#54757,#54758,#54759,#54760,#54761,#54762,#54763,#54764,#54765,
#54766,#54767,#54768,#54769,#54770,#54771,#54772,#54773,#54774,#54775,#54776,
#54777,#54778,#54779,#54780,#54781,#54782,#54783,#54784,#54785,#54786,#54787,
#54788,#54789,#54790,#54791,#54792,#54793,#54794,#54795,#54796,#54797,#54798,
#54799,#54800,#54801,#54802,#54803,#54804,#54805,#54806,#54807,#54808,#54809,
#54810,#54811,#54812,#54813,#54814,#54815,#54816,#54817,#54818,#54819,#54820,
#54821,#54822,#54823,#54824,#54825,#54826,#54827,#54828,#54829,#54830,#54831,
#54832,#54833,#54834,#54835,#54836,#54837,#54838,#54839,#54840,#54841,#54842,
#54843,#54844,#54845,#54846,#54847,#54848,#54849,#54850,#54851,#54852,#54853,
#54854,#54855,#54856,#54857,#54858,#54859,#54860,#54861,#54862,#54863,#54864,
#54865,#54866,#54867,#54868,#54869,#54870),.UNSPECIFIED.,.F.,.F.,(4,3,3,
3,3,3,3,3,3,3,3,3,3,3,3,3,3,3,3,3,3,3,3,3,3,3,3,3,3,3,3,3,3,3,3,3,3,3,3,
3,4),(-2.47011828786777,-2.39429498938945,-2.31085421816921,-2.2487987703988,
-2.21702958300785,-2.19665005734925,-2.18345847963518,-2.09925341052227,
-2.01449221995017,-1.92999116531367,-1.91521693514107,-1.90306118528872,
-1.81441063600599,-1.72993839179506,-1.64463244122103,-1.55899127324955,
-1.47459368269514,-1.44567397692449,-1.43778803581126,-1.35160714559026,
-1.264927968677,-1.22140091103189,-1.13509194280059,-1.04848479472449,-0.994484091434478,
-0.978663130413089,-0.969072712221302,-0.880924326267074,-0.793336817843973,
-0.704907993124182,-0.616479168404391,-0.539419272353842,-0.505705567831727,
-0.490288007695899,-0.482050594893607,-0.394957153060787,-0.306838265627068,
-0.218098308664458,-0.129586226722169,-0.0421749412600055,0.),
 .UNSPECIFIED.);
#398=B_SPLINE_CURVE_WITH_KNOTS('',3,(#54871,#54872,#54873,#54874,#54875,
#54876,#54877,#54878,#54879,#54880,#54881,#54882,#54883,#54884,#54885),
 .UNSPECIFIED.,.F.,.F.,(4,1,1,1,1,1,1,1,1,1,1,1,4),(10.3363935212333,10.7629123905843,
11.254507222043,11.7461020535017,12.2376968849604,12.729291716419,13.2208865478777,
13.7124813793364,14.204076210795,14.6956710422537,15.1872658737124,15.678860705171,
15.7079632679489),.UNSPECIFIED.);
#399=B_SPLINE_CURVE_WITH_KNOTS('',3,(#54887,#54888,#54889,#54890,#54891,
#54892),.UNSPECIFIED.,.F.,.F.,(4,2,4),(0.000204756358194638,0.0248404679347799,
0.148913229629469),.UNSPECIFIED.);
#400=B_SPLINE_CURVE_WITH_KNOTS('',3,(#54894,#54895,#54896,#54897),
 .UNSPECIFIED.,.F.,.F.,(4,4),(0.,0.00184861559299079),.UNSPECIFIED.);
#401=B_SPLINE_CURVE_WITH_KNOTS('',3,(#54899,#54900,#54901,#54902,#54903,
#54904,#54905,#54906,#54907,#54908,#54909,#54910,#54911,#54912,#54913,#54914,
#54915,#54916,#54917,#54918,#54919,#54920,#54921,#54922,#54923,#54924,#54925,
#54926,#54927,#54928,#54929,#54930,#54931,#54932,#54933,#54934,#54935,#54936,
#54937,#54938),.UNSPECIFIED.,.F.,.F.,(4,3,3,3,3,3,3,3,3,3,3,3,3,4),(34.240896913361,
34.4116382021068,34.9032330335655,35.3948278650241,35.8864226964828,36.3780175279415,
36.8696123594001,37.3612071908588,37.8528020223175,38.3443968537762,38.8359916852348,
39.3275865166935,39.8191813481521,40.255413574161),.UNSPECIFIED.);
#402=B_SPLINE_CURVE_WITH_KNOTS('',3,(#54940,#54941,#54942,#54943,#54944,
#54945,#54946,#54947,#54948,#54949,#54950,#54951,#54952,#54953,#54954,#54955,
#54956,#54957,#54958,#54959,#54960,#54961,#54962,#54963,#54964,#54965,#54966,
#54967,#54968,#54969,#54970,#54971,#54972,#54973,#54974,#54975,#54976,#54977,
#54978,#54979,#54980,#54981,#54982,#54983,#54984,#54985),.UNSPECIFIED.,
 .F.,.F.,(4,3,3,3,3,3,3,3,3,3,3,3,3,3,3,4),(0.,0.00275985982611835,0.0773912087755722,
0.109906700382361,0.163137701138107,0.167106859845295,0.168197417801363,
0.168838059529032,0.169391172014476,0.170064784081102,0.171335649356011,
0.178574547909555,0.187829967619597,0.233407240256718,0.305530899139838,
0.33843635522598),.UNSPECIFIED.);
#403=B_SPLINE_CURVE_WITH_KNOTS('',3,(#54987,#54988,#54989,#54990,#54991,
#54992,#54993,#54994,#54995,#54996,#54997,#54998,#54999,#55000,#55001,#55002,
#55003,#55004,#55005,#55006,#55007,#55008,#55009,#55010,#55011,#55012,#55013,
#55014,#55015,#55016,#55017,#55018,#55019,#55020,#55021,#55022,#55023,#55024,
#55025,#55026,#55027,#55028,#55029),.UNSPECIFIED.,.F.,.F.,(4,3,3,3,3,3,
3,3,3,3,3,3,3,3,4),(27.9577116061813,28.0209053931441,28.5125002246028,
29.0040950560614,29.4956898875201,29.9872847189788,30.4788795504374,30.9704743818961,
31.4620692133548,31.9536640448135,32.4452588762721,32.9368537077308,33.4284485391895,
33.9200433706481,33.9722282669813),.UNSPECIFIED.);
#404=B_SPLINE_CURVE_WITH_KNOTS('',3,(#55031,#55032,#55033,#55034,#55035,
#55036,#55037,#55038,#55039,#55040,#55041,#55042,#55043,#55044,#55045,#55046,
#55047,#55048,#55049,#55050,#55051,#55052,#55053,#55054,#55055,#55056,#55057,
#55058,#55059,#55060,#55061,#55062,#55063,#55064,#55065,#55066,#55067,#55068,
#55069,#55070,#55071,#55072,#55073,#55074,#55075,#55076),.UNSPECIFIED.,
 .F.,.F.,(4,3,3,3,3,3,3,3,3,3,3,3,3,3,3,4),(0.,0.00275985983231624,0.0771358287561839,
0.109906700741802,0.163137701683987,0.167106860406336,0.168197418376005,
0.168838060124296,0.169391172636416,0.170064784747918,0.171335650104608,
0.178574549108691,0.187829970005815,0.233407247867916,0.30571251857187,
0.338436366489491),.UNSPECIFIED.);
#405=B_SPLINE_CURVE_WITH_KNOTS('',3,(#55078,#55079,#55080,#55081,#55082,
#55083,#55084,#55085,#55086,#55087,#55088,#55089,#55090,#55091,#55092,#55093,
#55094,#55095,#55096,#55097,#55098,#55099,#55100,#55101,#55102,#55103,#55104,
#55105,#55106,#55107,#55108,#55109,#55110,#55111,#55112,#55113,#55114,#55115,
#55116,#55117),.UNSPECIFIED.,.F.,.F.,(4,3,3,3,3,3,3,3,3,3,3,3,3,4),(21.6745262990017,
22.1217674156401,22.6133622470988,23.1049570785574,23.5965519100161,24.0881467414748,
24.5797415729334,25.0713364043921,25.5629312358508,26.0545260673094,26.5461208987681,
27.0377157302268,27.5293105616854,27.6890429598018),.UNSPECIFIED.);
#406=B_SPLINE_CURVE_WITH_KNOTS('',3,(#55119,#55120,#55121,#55122,#55123,
#55124,#55125,#55126,#55127,#55128,#55129,#55130,#55131,#55132,#55133,#55134,
#55135,#55136,#55137,#55138,#55139,#55140,#55141,#55142,#55143,#55144,#55145,
#55146,#55147,#55148,#55149,#55150,#55151,#55152,#55153,#55154,#55155,#55156,
#55157,#55158,#55159,#55160,#55161,#55162,#55163,#55164),.UNSPECIFIED.,
 .F.,.F.,(4,3,3,3,3,3,3,3,3,3,3,3,3,3,3,4),(0.,0.00275985982612918,0.0767519898615825,
0.109906700366968,0.16313770113734,0.167106859849563,0.168197417798545,
0.168838059528161,0.169391172050885,0.170064784160668,0.171335649470964,
0.178574548234285,0.187829968981913,0.233407245948613,0.282033220718275,
0.338436360379489),.UNSPECIFIED.);
#407=B_SPLINE_CURVE_WITH_KNOTS('',3,(#55166,#55167,#55168,#55169,#55170,
#55171,#55172,#55173,#55174,#55175,#55176,#55177,#55178,#55179,#55180,#55181,
#55182,#55183,#55184,#55185,#55186,#55187,#55188,#55189,#55190,#55191,#55192,
#55193,#55194,#55195,#55196,#55197,#55198,#55199,#55200,#55201,#55202,#55203,
#55204,#55205),.UNSPECIFIED.,.F.,.F.,(4,3,3,3,3,3,3,3,3,3,3,3,3,4),(15.3913409918222,
15.7310346066774,16.2226294381361,16.7142242695947,17.2058191010534,17.6974139325121,
18.1890087639707,18.6806035954294,19.1721984268881,19.6637932583467,20.1553880898054,
20.6469829212641,21.1385777527227,21.4058576526223),.UNSPECIFIED.);
#408=B_SPLINE_CURVE_WITH_KNOTS('',3,(#55207,#55208,#55209,#55210,#55211,
#55212,#55213,#55214,#55215,#55216,#55217,#55218,#55219,#55220,#55221,#55222,
#55223,#55224,#55225,#55226,#55227,#55228,#55229,#55230,#55231,#55232,#55233,
#55234,#55235,#55236,#55237,#55238,#55239,#55240,#55241,#55242,#55243,#55244,
#55245,#55246,#55247,#55248,#55249,#55250,#55251,#55252,#55253,#55254,#55255),
 .UNSPECIFIED.,.F.,.F.,(4,3,3,3,3,3,3,3,3,3,3,3,3,3,3,3,4),(0.,0.00275985983348124,
0.0762148369746939,0.109906700802838,0.147108383127543,0.163137701785669,
0.167106860511849,0.168197418475418,0.168838060209463,0.169391172706176,
0.170064784805486,0.17133565015834,0.178574549091358,0.187829970095521,
0.233407248291307,0.304987043084035,0.338436364998264),.UNSPECIFIED.);
#409=B_SPLINE_CURVE_WITH_KNOTS('',3,(#55257,#55258,#55259,#55260,#55261,
#55262,#55263,#55264,#55265,#55266,#55267,#55268,#55269,#55270,#55271,#55272,
#55273,#55274,#55275,#55276,#55277,#55278,#55279,#55280,#55281,#55282,#55283,
#55284,#55285,#55286,#55287,#55288,#55289,#55290,#55291,#55292,#55293,#55294,
#55295,#55296),.UNSPECIFIED.,.F.,.F.,(4,3,3,3,3,3,3,3,3,3,3,3,3,4),(9.10815568464253,
9.3403017977147,9.83189662917337,10.323491460632,10.8150862920907,11.3066811235494,
11.798275955008,12.2898707864667,12.7814656179254,13.273060449384,13.7646552808427,
14.2562501123014,14.7478449437601,15.1226723454426),.UNSPECIFIED.);
#410=B_SPLINE_CURVE_WITH_KNOTS('',3,(#55298,#55299,#55300,#55301,#55302,
#55303,#55304,#55305,#55306,#55307,#55308,#55309,#55310,#55311,#55312,#55313,
#55314,#55315,#55316,#55317,#55318,#55319,#55320,#55321,#55322,#55323,#55324,
#55325,#55326,#55327,#55328,#55329,#55330,#55331,#55332,#55333,#55334,#55335,
#55336,#55337,#55338,#55339,#55340,#55341,#55342,#55343,#55344,#55345,#55346),
 .UNSPECIFIED.,.F.,.F.,(4,3,3,3,3,3,3,3,3,3,3,3,3,3,3,3,4),(0.,0.00275985982495649,
0.0117382940614391,0.0866092230060178,0.10990670029821,0.163137701034397,
0.167106859741717,0.168197417701499,0.16883805943631,0.169391171934133,
0.170064784030677,0.171335649369872,0.178574548176285,0.187829968961567,
0.233407246130877,0.305372769891771,0.338436361290398),.UNSPECIFIED.);
#411=B_SPLINE_CURVE_WITH_KNOTS('',3,(#55347,#55348,#55349,#55350,#55351,
#55352,#55353,#55354,#55355,#55356,#55357,#55358,#55359,#55360,#55361,#55362,
#55363,#55364,#55365,#55366,#55367,#55368,#55369,#55370,#55371,#55372,#55373,
#55374,#55375,#55376,#55377,#55378,#55379,#55380,#55381,#55382,#55383,#55384,
#55385,#55386),.UNSPECIFIED.,.F.,.F.,(4,3,3,3,3,3,3,3,3,3,3,3,3,4),(2.82497037746304,
2.94956898875201,3.44116382021067,3.93275865166934,4.42435348312801,4.91594831458668,
5.40754314604535,5.89913797750402,6.39073280896269,6.88232764042136,7.37392247188002,
7.86551730333869,8.35711213479736,8.8394870382631),.UNSPECIFIED.);
#412=B_SPLINE_CURVE_WITH_KNOTS('',3,(#55424,#55425,#55426,#55427,#55428,
#55429,#55430,#55431,#55432,#55433,#55434,#55435,#55436),.UNSPECIFIED.,
 .F.,.F.,(4,3,3,3,4),(0.,0.037446429103661,0.0586081614907165,0.0940217092267908,
0.11745568348674),.UNSPECIFIED.);
#413=B_SPLINE_CURVE_WITH_KNOTS('',3,(#55438,#55439,#55440,#55441,#55442,
#55443,#55444,#55445,#55446,#55447,#55448,#55449,#55450,#55451,#55452,#55453,
#55454,#55455,#55456),.UNSPECIFIED.,.F.,.F.,(4,3,3,3,3,3,4),(40.5278112792784,
41.1194668394256,41.4405772287596,41.7616876180936,42.4039083967615,42.7250187860955,
43.3613098903777),.UNSPECIFIED.);
#414=B_SPLINE_CURVE_WITH_KNOTS('',3,(#55457,#55458,#55459,#55460,#55461,
#55462,#55463,#55464,#55465,#55466,#55467,#55468,#55469,#55470,#55471,#55472,
#55473,#55474,#55475),.UNSPECIFIED.,.F.,.F.,(4,3,3,3,3,3,4),(0.,0.00617385261260148,
0.0296247466034154,0.0555909177237707,0.0757825634092935,0.10848938045471,
0.133283104059319),.UNSPECIFIED.);
#415=B_SPLINE_CURVE_WITH_KNOTS('',3,(#55514,#55515,#55516,#55517,#55518,
#55519,#55520,#55521,#55522,#55523,#55524,#55525,#55526),.UNSPECIFIED.,
 .F.,.F.,(4,3,3,3,4),(0.,0.0429420950889889,0.0600161086838339,0.10053591690027,
0.119365066230604),.UNSPECIFIED.);
#416=B_SPLINE_CURVE_WITH_KNOTS('',3,(#55528,#55529,#55530,#55531,#55532,
#55533,#55534,#55535,#55536,#55537,#55538,#55539,#55540,#55541,#55542,#55543,
#55544,#55545,#55546),.UNSPECIFIED.,.F.,.F.,(4,3,3,3,3,3,4),(43.7031624395564,
44.3223587209537,44.6334770539754,44.944595386997,45.5668320530402,46.1890687190835,
46.5001870521051),.UNSPECIFIED.);
#417=B_SPLINE_CURVE_WITH_KNOTS('',3,(#55548,#55549,#55550,#55551,#55552,
#55553,#55554,#55555,#55556,#55557,#55558,#55559,#55560,#55561,#55562,#55563),
 .UNSPECIFIED.,.F.,.F.,(4,3,3,3,3,4),(0.,0.000528350741057718,0.0356313944030074,
0.05930235574727,0.0966015584375564,0.117357984280487),.UNSPECIFIED.);
#418=B_SPLINE_CURVE_WITH_KNOTS('',3,(#55564,#55565,#55566,#55567,#55568,
#55569,#55570,#55571,#55572),.UNSPECIFIED.,.F.,.F.,(4,1,1,1,1,1,4),(52.0050602882015,
52.6272969542447,52.9384152872664,53.249533620288,53.8717702863312,54.4940069523745,
54.7879760688686),.UNSPECIFIED.);
#419=B_SPLINE_CURVE_WITH_KNOTS('',3,(#55611,#55612,#55613,#55614,#55615,
#55616,#55617,#55618,#55619,#55620,#55621,#55622,#55623,#55624,#55625,#55626),
 .UNSPECIFIED.,.F.,.F.,(4,3,3,3,3,4),(0.,0.000603782874981952,0.0414065099753013,
0.0599624018758385,0.103177307014501,0.119350753234639),.UNSPECIFIED.);
#420=B_SPLINE_CURVE_WITH_KNOTS('',3,(#55628,#55629,#55630,#55631,#55632,
#55633,#55634,#55635,#55636),.UNSPECIFIED.,.F.,.F.,(4,1,1,1,1,1,4),(55.168486169442,
55.4633418551201,56.0919205048047,56.7204991544894,57.0347884793317,57.349077804174,
57.9383886020288),.UNSPECIFIED.);
#421=B_SPLINE_CURVE_WITH_KNOTS('',3,(#55638,#55639,#55640,#55641,#55642,
#55643,#55644,#55645,#55646,#55647,#55648,#55649,#55650),.UNSPECIFIED.,
 .F.,.F.,(4,3,3,3,4),(0.,0.0383618973007027,0.0643956823821936,0.106213551033925,
0.126965609850118),.UNSPECIFIED.);
#422=B_SPLINE_CURVE_WITH_KNOTS('',3,(#55651,#55652,#55653,#55654,#55655,
#55656,#55657,#55658,#55659,#55660,#55661,#55662,#55663,#55664,#55665,#55666,
#55667,#55668,#55669),.UNSPECIFIED.,.F.,.F.,(4,3,3,3,3,3,4),(46.8441142969868,
47.1584036218291,47.7869822715137,48.4155609211983,48.7298502460407,49.044139570883,
49.6727182205676),.UNSPECIFIED.);
#423=B_SPLINE_CURVE_WITH_KNOTS('',3,(#55860,#55861,#55862,#55863,#55864,
#55865,#55866,#55867,#55868,#55869,#55870,#55871,#55872,#55873,#55874,#55875,
#55876,#55877,#55878,#55879,#55880,#55881,#55882,#55883,#55884,#55885,#55886,
#55887,#55888,#55889,#55890,#55891,#55892,#55893,#55894,#55895,#55896,#55897,
#55898,#55899,#55900,#55901,#55902,#55903,#55904,#55905),.UNSPECIFIED.,
 .F.,.F.,(4,3,3,3,3,3,3,3,3,3,3,3,3,3,3,4),(0.,0.00275985982602131,0.0774481870978171,
0.109906700355626,0.163137701127091,0.167106859837268,0.168197417788825,
0.168838059519517,0.169391172034677,0.170064784150426,0.171335649507718,
0.178574548452424,0.187829969840206,0.233407249547609,0.305452969896819,
0.338436364727379),.UNSPECIFIED.);
#424=B_SPLINE_CURVE_WITH_KNOTS('',3,(#55907,#55908,#55909,#55910,#55911,
#55912,#55913,#55914,#55915,#55916,#55917,#55918,#55919,#55920,#55921,#55922,
#55923,#55924,#55925,#55926,#55927,#55928,#55929,#55930,#55931,#55932,#55933,
#55934,#55935,#55936,#55937,#55938,#55939,#55940,#55941,#55942,#55943,#55944,
#55945,#55946),.UNSPECIFIED.,.F.,.F.,(4,3,3,3,3,3,3,3,3,3,3,3,3,4),(-74.551458153763,
-74.0564455670154,-73.5614329802678,-73.0664203935202,-72.5714078067726,
-72.076395220025,-71.5813826332774,-71.0863700465298,-70.5913574597822,
-70.0963448730346,-69.601332286287,-69.1063196995394,-68.6113071127918,
-68.5901919358345),.UNSPECIFIED.);
#425=B_SPLINE_CURVE_WITH_KNOTS('',3,(#55947,#55948,#55949,#55950,#55951,
#55952,#55953,#55954,#55955,#55956,#55957,#55958,#55959,#55960,#55961,#55962,
#55963,#55964,#55965,#55966,#55967,#55968,#55969,#55970,#55971,#55972,#55973,
#55974,#55975,#55976,#55977,#55978,#55979,#55980,#55981,#55982,#55983,#55984,
#55985,#55986,#55987,#55988,#55989,#55990,#55991,#55992,#55993,#55994,#55995,
#55996,#55997,#55998,#55999,#56000,#56001,#56002,#56003,#56004,#56005,#56006,
#56007,#56008,#56009,#56010,#56011,#56012,#56013,#56014,#56015,#56016,#56017,
#56018,#56019,#56020,#56021,#56022,#56023,#56024,#56025,#56026,#56027,#56028,
#56029,#56030,#56031,#56032,#56033,#56034,#56035,#56036,#56037,#56038,#56039,
#56040,#56041,#56042,#56043,#56044,#56045,#56046,#56047,#56048,#56049,#56050,
#56051,#56052,#56053,#56054,#56055,#56056,#56057,#56058,#56059,#56060,#56061,
#56062,#56063,#56064,#56065,#56066,#56067,#56068,#56069,#56070),
 .UNSPECIFIED.,.F.,.F.,(4,3,3,3,3,3,3,3,3,3,3,3,3,3,3,3,3,3,3,3,3,3,3,3,
3,3,3,3,3,3,3,3,3,3,3,3,3,3,3,3,3,4),(-2.47011828786777,-2.41024950183313,
-2.32691774162747,-2.2429717964809,-2.20769641248666,-2.19373056076968,
-2.18265358177193,-2.09840120325056,-2.0136380142207,-1.92915370148376,
-1.91349624184333,-1.90340003136624,-1.82664733476972,-1.74228691319791,
-1.65704413290003,-1.57140550422496,-1.48598895300347,-1.45395774629541,
-1.44439537040528,-1.43517678553118,-1.34896088996718,-1.2622812294094,
-1.22973929933899,-1.1434685919942,-1.05685735056476,-1.00234107811919,
-0.97705394199646,-0.963473476685488,-0.876380514947321,-0.788767505252353,
-0.701239870826566,-0.620727171000232,-0.543136274625203,-0.509190257461128,
-0.49537754808107,-0.482348253819253,-0.395240424237199,-0.307110366650991,
-0.21836748424028,-0.129858392843112,-0.0424592967429643,0.),
 .UNSPECIFIED.);
#426=B_SPLINE_CURVE_WITH_KNOTS('',3,(#56072,#56073,#56074,#56075,#56076,
#56077,#56078),.UNSPECIFIED.,.F.,.F.,(4,1,1,1,4),(64.4256593907634,64.920671977511,
65.4156845642586,65.9106971510062,65.9734457253856),.UNSPECIFIED.);
#427=B_SPLINE_CURVE_WITH_KNOTS('',3,(#56080,#56081,#56082,#56083,#56084,
#56085,#56086,#56087,#56088,#56089),.UNSPECIFIED.,.F.,.F.,(4,2,2,2,4),(0.,
0.000413391377648547,0.0678668660539045,0.107676089687835,0.167694447832979),
 .UNSPECIFIED.);
#428=B_SPLINE_CURVE_WITH_KNOTS('',3,(#56091,#56092,#56093,#56094,#56095,
#56096,#56097,#56098,#56099,#56100,#56101,#56102,#56103,#56104,#56105,#56106,
#56107,#56108,#56109,#56110,#56111,#56112),.UNSPECIFIED.,.F.,.F.,(4,3,3,
3,3,3,3,4),(-55.7551526750958,-55.7409798573541,-55.2459672706065,-54.7509546838589,
-54.2559420971113,-53.7609295103637,-53.2659169236161,-52.8657784087353),
 .UNSPECIFIED.);
#429=B_SPLINE_CURVE_WITH_KNOTS('',3,(#56114,#56115,#56116,#56117,#56118,
#56119,#56120,#56121,#56122,#56123,#56124,#56125,#56126,#56127,#56128,#56129,
#56130,#56131,#56132,#56133,#56134,#56135,#56136,#56137,#56138,#56139,#56140,
#56141,#56142,#56143,#56144,#56145,#56146,#56147,#56148,#56149,#56150,#56151,
#56152,#56153,#56154,#56155,#56156,#56157,#56158,#56159),.UNSPECIFIED.,
 .F.,.F.,(4,3,3,3,3,3,3,3,3,3,3,3,3,3,3,4),(0.,0.00275985982145796,0.0769740122567431,
0.109906700085914,0.163137700726612,0.167106859425189,0.168197417377174,
0.168838059113662,0.16939117163383,0.170064783759705,0.171335649155779,
0.178574548370381,0.187829970155368,0.233407251759405,0.305760949417455,
0.338436370550636),.UNSPECIFIED.);
#430=B_SPLINE_CURVE_WITH_KNOTS('',3,(#56161,#56162,#56163,#56164,#56165,
#56166,#56167,#56168,#56169,#56170,#56171,#56172,#56173,#56174,#56175,#56176,
#56177,#56178,#56179,#56180,#56181,#56182,#56183,#56184,#56185,#56186,#56187,
#56188,#56189,#56190,#56191,#56192,#56193,#56194,#56195,#56196,#56197,#56198,
#56199,#56200),.UNSPECIFIED.,.F.,.F.,(4,3,3,3,3,3,3,3,3,3,3,3,3,4),(-62.0383379822753,
-61.6811308983253,-61.1861183115777,-60.6911057248301,-60.1960931380825,
-59.7010805513349,-59.2060679645873,-58.7110553778397,-58.2160427910921,
-57.7210302043445,-57.2260176175969,-56.7310050308493,-56.2359924441017,
-56.0238213214754),.UNSPECIFIED.);
#431=B_SPLINE_CURVE_WITH_KNOTS('',3,(#56202,#56203,#56204,#56205,#56206,
#56207,#56208,#56209,#56210,#56211,#56212,#56213,#56214,#56215,#56216,#56217,
#56218,#56219,#56220,#56221,#56222,#56223,#56224,#56225,#56226,#56227,#56228,
#56229,#56230,#56231,#56232,#56233,#56234,#56235,#56236,#56237,#56238,#56239,
#56240,#56241,#56242,#56243,#56244,#56245,#56246,#56247,#56248,#56249,#56250),
 .UNSPECIFIED.,.F.,.F.,(4,3,3,3,3,3,3,3,3,3,3,3,3,3,3,3,4),(0.,0.00275985982151005,
0.0762872625369273,0.109906700097837,0.163137700732282,0.164734489152777,
0.167106859431402,0.168197417392199,0.168838059132773,0.169391171638563,
0.170064783750812,0.17133564913502,0.178574548241108,0.187829969458916,
0.233407248703376,0.304919373849625,0.338436367941764),.UNSPECIFIED.);
#432=B_SPLINE_CURVE_WITH_KNOTS('',3,(#56251,#56252,#56253,#56254,#56255,
#56256,#56257,#56258,#56259,#56260,#56261,#56262,#56263,#56264,#56265,#56266,
#56267,#56268,#56269,#56270,#56271,#56272,#56273,#56274,#56275,#56276,#56277,
#56278,#56279,#56280,#56281,#56282,#56283,#56284,#56285,#56286,#56287,#56288,
#56289,#56290),.UNSPECIFIED.,.F.,.F.,(4,3,3,3,3,3,3,3,3,3,3,3,3,4),(-68.321523289455,
-68.1162945260442,-67.6212819392966,-67.126269352549,-66.6312567658014,
-66.1362441790538,-65.6412315923062,-65.1462190055586,-64.651206418811,
-64.1561938320634,-63.6611812453157,-63.1661686585681,-62.6711560718205,
-62.3070066286549),.UNSPECIFIED.);
#433=B_SPLINE_CURVE_WITH_KNOTS('',3,(#56329,#56330,#56331,#56332,#56333,
#56334,#56335,#56336,#56337,#56338,#56339,#56340,#56341,#56342,#56343,#56344),
 .UNSPECIFIED.,.F.,.F.,(4,3,3,3,3,4),(0.,0.000524175925068961,0.0370091730147864,
0.0592526903266393,0.094159836272508,0.118128821372448),.UNSPECIFIED.);
#434=B_SPLINE_CURVE_WITH_KNOTS('',3,(#56346,#56347,#56348,#56349,#56350,
#56351,#56352,#56353,#56354,#56355,#56356,#56357,#56358,#56359,#56360,#56361,
#56362,#56363,#56364),.UNSPECIFIED.,.F.,.F.,(4,3,3,3,3,3,4),(-52.6241835979417,
-52.387037036532,-51.730035730462,-51.073034424392,-50.744533771357,-50.087532465287,
-49.7715547347365),.UNSPECIFIED.);
#435=B_SPLINE_CURVE_WITH_KNOTS('',3,(#56366,#56367,#56368,#56369,#56370,
#56371,#56372,#56373),.UNSPECIFIED.,.F.,.F.,(4,2,2,4),(0.,0.0343081782947535,
0.0828883632862996,0.165726765447382),.UNSPECIFIED.);
#436=B_SPLINE_CURVE_WITH_KNOTS('',3,(#56374,#56375,#56376,#56377,#56378,
#56379,#56380,#56381,#56382),.UNSPECIFIED.,.F.,.F.,(4,1,1,1,1,1,4),(61.413786866147,
61.742287519182,62.399288825252,62.727789478287,63.384790784357,64.041792090427,
64.370292743462),.UNSPECIFIED.);
#437=B_SPLINE_CURVE_WITH_KNOTS('',3,(#56421,#56422,#56423,#56424,#56425,
#56426,#56427,#56428,#56429,#56430,#56431,#56432,#56433,#56434,#56435,#56436),
 .UNSPECIFIED.,.F.,.F.,(4,3,3,3,3,4),(0.,0.000559897176802773,0.042322412952373,
0.0600025715731581,0.0991684809679751,0.118377563451883),.UNSPECIFIED.);
#438=B_SPLINE_CURVE_WITH_KNOTS('',3,(#56438,#56439,#56440,#56441,#56442,
#56443,#56444,#56445,#56446,#56447,#56448,#56449,#56450,#56451,#56452,#56453,
#56454,#56455,#56456),.UNSPECIFIED.,.F.,.F.,(4,3,3,3,3,3,4),(-49.4385230424123,
-49.1359708046958,-48.5118455167721,-47.8877202288484,-47.5756575848866,
-47.2635949409247,-46.639469653001),.UNSPECIFIED.);
#439=B_SPLINE_CURVE_WITH_KNOTS('',3,(#56458,#56459,#56460,#56461,#56462,
#56463,#56464,#56465,#56466,#56467,#56468,#56469,#56470),.UNSPECIFIED.,
 .F.,.F.,(4,3,3,3,4),(0.,0.0344844180980609,0.0592774715655555,0.0955221408315289,
0.117941444539697),.UNSPECIFIED.);
#440=B_SPLINE_CURVE_WITH_KNOTS('',3,(#56471,#56472,#56473,#56474,#56475,
#56476,#56477,#56478,#56479),.UNSPECIFIED.,.F.,.F.,(4,1,1,1,1,1,4),(58.3068143978534,
58.9183499948197,59.2304126387815,59.5424752827434,60.166600570667,60.7907258585907,
61.1027885025526),.UNSPECIFIED.);
#441=B_SPLINE_CURVE_WITH_KNOTS('',3,(#56822,#56823,#56824,#56825,#56826,
#56827,#56828,#56829,#56830,#56831,#56832,#56833,#56834,#56835,#56836,#56837,
#56838,#56839,#56840,#56841,#56842,#56843,#56844,#56845,#56846,#56847,#56848,
#56849,#56850,#56851,#56852,#56853,#56854,#56855,#56856,#56857,#56858,#56859,
#56860,#56861,#56862,#56863,#56864,#56865,#56866,#56867),.UNSPECIFIED.,
 .F.,.F.,(4,3,3,3,3,3,3,3,3,3,3,3,3,3,3,4),(0.,0.00275985983228642,0.077257938139478,
0.109906700732534,0.163137701680564,0.167106860403426,0.168197418365421,
0.168838060104028,0.169391172613466,0.170064784717482,0.171335650058926,
0.178574549011496,0.187829969760767,0.233407246964211,0.305648570218663,
0.338436365203866),.UNSPECIFIED.);
#442=B_SPLINE_CURVE_WITH_KNOTS('',3,(#56869,#56870,#56871,#56872,#56873,
#56874,#56875,#56876,#56877,#56878,#56879,#56880,#56881,#56882,#56883,#56884,
#56885,#56886,#56887,#56888,#56889,#56890,#56891,#56892,#56893,#56894,#56895,
#56896,#56897,#56898,#56899,#56900,#56901,#56902,#56903,#56904,#56905,#56906,
#56907,#56908,#56909,#56910,#56911),.UNSPECIFIED.,.F.,.F.,(4,3,3,3,3,3,
3,3,3,3,3,3,3,3,4),(-11.7728555248387,-11.7422679037385,-11.2530067410827,
-10.7637455784269,-10.2744844157712,-9.78522325311539,-9.29596209045961,
-8.80670092780385,-8.31743976514808,-7.82817860249231,-7.33891743983654,
-6.84965627718077,-6.360395114525,-5.87113395186923,-5.75833886403865),
 .UNSPECIFIED.);
#443=B_SPLINE_CURVE_WITH_KNOTS('',3,(#56913,#56914,#56915,#56916,#56917,
#56918,#56919,#56920,#56921,#56922,#56923,#56924,#56925,#56926,#56927,#56928,
#56929,#56930,#56931,#56932,#56933,#56934,#56935,#56936,#56937,#56938,#56939,
#56940,#56941,#56942,#56943,#56944,#56945,#56946,#56947,#56948,#56949,#56950,
#56951,#56952,#56953,#56954,#56955,#56956,#56957,#56958),.UNSPECIFIED.,
 .F.,.F.,(4,3,3,3,3,3,3,3,3,3,3,3,3,3,3,4),(0.,0.00275985982376174,0.0770370771830512,
0.109906700228133,0.163137700929448,0.167106859635108,0.168197417591288,
0.168838059324371,0.169391171829,0.170064783926107,0.171335649248441,0.178574548066871,
0.187829968616436,0.233407244865315,0.30574397986754,0.338436361285487),
 .UNSPECIFIED.);
#444=B_SPLINE_CURVE_WITH_KNOTS('',3,(#56960,#56961,#56962,#56963,#56964,
#56965,#56966,#56967,#56968,#56969,#56970,#56971,#56972,#56973,#56974,#56975,
#56976,#56977,#56978,#56979,#56980,#56981,#56982,#56983,#56984,#56985,#56986,
#56987,#56988,#56989,#56990,#56991,#56992,#56993,#56994,#56995,#56996,#56997,
#56998,#56999),.UNSPECIFIED.,.F.,.F.,(4,3,3,3,3,3,3,3,3,3,3,3,3,4),(-18.0560408320183,
-17.6134018556077,-17.1241406929519,-16.6348795302962,-16.1456183676404,
-15.6563572049846,-15.1670960423288,-14.6778348796731,-14.1885737170173,
-13.6993125543615,-13.2100513917058,-12.72079022905,-12.2315290663942,-12.0415241712181),
 .UNSPECIFIED.);
#445=B_SPLINE_CURVE_WITH_KNOTS('',3,(#57001,#57002,#57003,#57004,#57005,
#57006,#57007,#57008,#57009,#57010,#57011,#57012,#57013,#57014,#57015,#57016,
#57017,#57018,#57019,#57020,#57021,#57022,#57023,#57024,#57025,#57026,#57027,
#57028,#57029,#57030,#57031,#57032,#57033,#57034,#57035,#57036,#57037,#57038,
#57039,#57040,#57041,#57042,#57043,#57044,#57045,#57046),.UNSPECIFIED.,
 .F.,.F.,(4,3,3,3,3,3,3,3,3,3,3,3,3,3,3,4),(0.,0.00275985983113353,0.0767461432217819,
0.10990670066103,0.163137701579206,0.167106860299809,0.168197418254294,
0.168838059995389,0.169391172533029,0.17006478467472,0.171335650088616,
0.178574549335223,0.187829970571773,0.233407250081592,0.279164911505272,
0.338436372145432),.UNSPECIFIED.);
#446=B_SPLINE_CURVE_WITH_KNOTS('',3,(#57048,#57049,#57050,#57051,#57052,
#57053,#57054,#57055,#57056,#57057,#57058,#57059,#57060,#57061,#57062,#57063,
#57064,#57065,#57066,#57067,#57068,#57069,#57070,#57071,#57072,#57073,#57074,
#57075,#57076,#57077,#57078,#57079,#57080,#57081,#57082,#57083,#57084,#57085,
#57086,#57087),.UNSPECIFIED.,.F.,.F.,(4,3,3,3,3,3,3,3,3,3,3,3,3,4),(-24.3392261391979,
-23.9737969701327,-23.4845358074769,-22.9952746448212,-22.5060134821654,
-22.0167523195096,-21.5274911568539,-21.0382299941981,-20.5489688315423,
-20.0597076688865,-19.5704465062308,-19.081185343575,-18.5919241809192,
-18.3247094783978),.UNSPECIFIED.);
#447=B_SPLINE_CURVE_WITH_KNOTS('',3,(#57089,#57090,#57091,#57092,#57093,
#57094,#57095,#57096,#57097,#57098,#57099,#57100,#57101,#57102,#57103,#57104,
#57105,#57106,#57107,#57108,#57109,#57110,#57111,#57112,#57113,#57114,#57115,
#57116,#57117,#57118,#57119,#57120,#57121,#57122,#57123,#57124,#57125,#57126,
#57127,#57128,#57129,#57130,#57131,#57132,#57133,#57134,#57135,#57136,#57137),
 .UNSPECIFIED.,.F.,.F.,(4,3,3,3,3,3,3,3,3,3,3,3,3,3,3,3,4),(0.,0.00275985982375089,
0.0763759506442948,0.109906700228139,0.163137700928605,0.167106859632871,
0.168197417593916,0.168838059333146,0.169391171837645,0.170064783944139,
0.171335649305587,0.17857454832124,0.182207199497083,0.18782996934018,0.233407247686735,
0.304865724045757,0.338436365949266),.UNSPECIFIED.);
#448=B_SPLINE_CURVE_WITH_KNOTS('',3,(#57139,#57140,#57141,#57142,#57143,
#57144,#57145,#57146,#57147,#57148,#57149,#57150,#57151,#57152,#57153,#57154,
#57155,#57156,#57157,#57158,#57159,#57160,#57161,#57162,#57163,#57164,#57165,
#57166,#57167,#57168,#57169,#57170,#57171,#57172,#57173,#57174,#57175,#57176,
#57177,#57178),.UNSPECIFIED.,.F.,.F.,(4,3,3,3,3,3,3,3,3,3,3,3,3,4),(-30.6224114463774,
-30.3341920846577,-29.8449309220019,-29.3556697593462,-28.8664085966904,
-28.3771474340346,-27.8878862713788,-27.3986251087231,-26.9093639460673,
-26.4201027834115,-25.9308416207558,-25.4415804581,-24.9523192954442,-24.6078947855774),
 .UNSPECIFIED.);
#449=B_SPLINE_CURVE_WITH_KNOTS('',3,(#57180,#57181,#57182,#57183,#57184,
#57185,#57186,#57187,#57188,#57189,#57190,#57191,#57192,#57193,#57194,#57195,
#57196,#57197,#57198,#57199,#57200,#57201,#57202,#57203,#57204,#57205,#57206,
#57207,#57208,#57209,#57210,#57211,#57212,#57213,#57214,#57215,#57216,#57217,
#57218,#57219,#57220,#57221,#57222,#57223,#57224,#57225,#57226,#57227,#57228),
 .UNSPECIFIED.,.F.,.F.,(4,3,3,3,3,3,3,3,3,3,3,3,3,3,3,3,4),(0.,0.00275985982375613,
0.0756134546611658,0.0855438259912015,0.10990670022032,0.163137700928118,
0.167106859633686,0.168197417590077,0.168838059326623,0.169391171839922,
0.170064783940488,0.171335649227684,0.178574547859423,0.187829968945836,
0.233407247069485,0.305184663799026,0.338436357196743),.UNSPECIFIED.);
#450=B_SPLINE_CURVE_WITH_KNOTS('',3,(#57230,#57231,#57232,#57233,#57234,
#57235,#57236,#57237,#57238,#57239,#57240,#57241,#57242,#57243,#57244,#57245,
#57246,#57247,#57248,#57249,#57250,#57251,#57252,#57253,#57254,#57255,#57256,
#57257,#57258,#57259,#57260,#57261,#57262,#57263,#57264,#57265,#57266,#57267,
#57268,#57269),.UNSPECIFIED.,.F.,.F.,(4,3,3,3,3,3,3,3,3,3,3,3,3,4),(-36.905596753557,
-36.6945871991827,-36.2053260365269,-35.7160648738711,-35.2268037112154,
-34.7375425485596,-34.2482813859039,-33.7590202232481,-33.2697590605923,
-32.7804978979365,-32.2912367352808,-31.801975572625,-31.3127144099692,
-30.8910800927569),.UNSPECIFIED.);
#451=B_SPLINE_CURVE_WITH_KNOTS('',3,(#57271,#57272,#57273,#57274,#57275,
#57276,#57277,#57278,#57279,#57280,#57281,#57282,#57283,#57284,#57285,#57286,
#57287,#57288,#57289,#57290,#57291,#57292,#57293,#57294,#57295,#57296,#57297,
#57298,#57299,#57300,#57301,#57302,#57303,#57304,#57305,#57306,#57307,#57308,
#57309,#57310,#57311,#57312,#57313,#57314,#57315,#57316),.UNSPECIFIED.,
 .F.,.F.,(4,3,3,3,3,3,3,3,3,3,3,3,3,3,3,4),(0.,0.00275985982374703,0.0774602223847068,
0.109906700228556,0.163137700928317,0.167106859634754,0.168197417583678,
0.168838059317443,0.169391171848623,0.170064783974852,0.171335649325392,
0.178574548289135,0.187829969380545,0.233407247950148,0.305428214865697,
0.338436364853883),.UNSPECIFIED.);
#452=B_SPLINE_CURVE_WITH_KNOTS('',3,(#57318,#57319,#57320,#57321,#57322,
#57323,#57324,#57325,#57326,#57327,#57328,#57329,#57330,#57331,#57332,#57333,
#57334,#57335,#57336,#57337,#57338,#57339),.UNSPECIFIED.,.F.,.F.,(4,3,3,
3,3,3,3,4),(-40.1194153377731,-39.6301541751173,-39.1408930124615,-38.6516318498058,
-38.16237068715,-37.6731095244942,-37.1838483618385,-37.1742653999366),
 .UNSPECIFIED.);
#453=B_SPLINE_CURVE_WITH_KNOTS('',3,(#57340,#57341,#57342,#57343,#57344,
#57345,#57346,#57347,#57348,#57349,#57350,#57351,#57352,#57353,#57354,#57355,
#57356,#57357,#57358,#57359,#57360,#57361),.UNSPECIFIED.,.F.,.F.,(4,3,3,
3,3,3,3,4),(0.,0.0298454239823248,0.0587107917683048,0.0694364850727102,
0.0931059490162252,0.116200547796362,0.13859691269707,0.149774774907473),
 .UNSPECIFIED.);
#454=B_SPLINE_CURVE_WITH_KNOTS('',3,(#57363,#57364,#57365,#57366,#57367,
#57368,#57369,#57370,#57371,#57372,#57373,#57374),.UNSPECIFIED.,.F.,.F.,
(4,1,1,1,1,1,1,1,1,4),(11.654755053895,12.1440162165507,12.6332773792065,
13.1225385418623,13.611799704518,14.1010608671738,14.5903220298296,15.0795831924853,
15.5688443551411,15.707963267949),.UNSPECIFIED.);
#455=B_SPLINE_CURVE_WITH_KNOTS('',3,(#57376,#57377,#57378,#57379,#57380,
#57381,#57382,#57383,#57384,#57385,#57386,#57387,#57388,#57389,#57390,#57391,
#57392,#57393,#57394,#57395,#57396,#57397,#57398,#57399,#57400,#57401,#57402,
#57403,#57404,#57405,#57406,#57407,#57408,#57409,#57410,#57411,#57412,#57413,
#57414,#57415,#57416,#57417,#57418,#57419,#57420,#57421,#57422,#57423,#57424,
#57425,#57426,#57427,#57428,#57429,#57430,#57431,#57432,#57433,#57434,#57435,
#57436,#57437,#57438,#57439,#57440,#57441,#57442,#57443,#57444,#57445,#57446,
#57447,#57448,#57449,#57450,#57451,#57452,#57453,#57454,#57455,#57456,#57457,
#57458,#57459,#57460,#57461,#57462,#57463,#57464,#57465,#57466,#57467,#57468,
#57469,#57470,#57471,#57472,#57473,#57474,#57475,#57476,#57477,#57478,#57479,
#57480,#57481,#57482,#57483,#57484,#57485,#57486,#57487,#57488,#57489,#57490,
#57491,#57492,#57493,#57494,#57495,#57496,#57497,#57498,#57499,#57500,#57501,
#57502),.UNSPECIFIED.,.F.,.F.,(4,3,3,3,3,3,3,3,3,3,3,3,3,3,3,3,3,3,3,3,
3,3,3,3,3,3,3,3,3,3,3,3,3,3,3,3,3,3,3,3,3,3,4),(-2.4657711816956,-2.37742988198504,
-2.37203686248739,-2.2834262203604,-2.21828108582746,-2.18798524934555,
-2.16783026643965,-2.15520023029036,-2.06721376735589,-1.9794908344413,
-1.8924658234541,-1.87064293008793,-1.86055558238173,-1.77341354772103,
-1.76226514409688,-1.67528516349454,-1.58795101178645,-1.50086017635826,
-1.4164004091096,-1.3970664196555,-1.385204327045,-1.29903625463541,-1.21307140372724,
-1.16302110736361,-1.07672492900881,-0.990705158543006,-0.938804325301365,
-0.925019860062695,-0.913972265813138,-0.828818892685938,-0.743601294890201,
-0.659189663034413,-0.575498492609885,-0.503561181033649,-0.472088607219046,
-0.460708940919763,-0.450070986721853,-0.366465695615636,-0.282278701507383,
-0.198277355611721,-0.114917112729238,-0.0330178077316585,0.),
 .UNSPECIFIED.);
#456=B_SPLINE_CURVE_WITH_KNOTS('',3,(#57503,#57504,#57505,#57506,#57507,
#57508,#57509,#57510,#57511,#57512,#57513,#57514,#57515,#57516,#57517,#57518,
#57519,#57520,#57521,#57522,#57523,#57524,#57525,#57526,#57527),
 .UNSPECIFIED.,.F.,.F.,(4,3,3,3,3,3,3,3,4),(-5.48967021765908,-5.38187278921346,
-4.89261162655769,-4.40335046390192,-3.91408930124615,-3.42482813859038,
-2.93556697593462,-2.44630581327885,-2.03145528794232),.UNSPECIFIED.);
#457=B_SPLINE_CURVE_WITH_KNOTS('',3,(#57566,#57567,#57568,#57569,#57570,
#57571,#57572,#57573,#57574,#57575,#57576,#57577,#57578),.UNSPECIFIED.,
 .F.,.F.,(4,3,3,3,4),(0.,0.0431803782595757,0.0615400944013658,0.102677518916927,
0.124427909767835),.UNSPECIFIED.);
#458=B_SPLINE_CURVE_WITH_KNOTS('',3,(#57580,#57581,#57582,#57583,#57584,
#57585,#57586,#57587,#57588),.UNSPECIFIED.,.F.,.F.,(4,1,1,1,1,1,4),(51.9824652652652,
52.230691972308,52.8804712757956,53.2053609275394,53.855140231027,54.1800298827708,
54.7942738648993),.UNSPECIFIED.);
#459=B_SPLINE_CURVE_WITH_KNOTS('',3,(#57590,#57591,#57592,#57593,#57594,
#57595,#57596,#57597,#57598,#57599,#57600,#57601,#57602,#57603,#57604,#57605,
#57606,#57607,#57608,#57609,#57610,#57611),.UNSPECIFIED.,.F.,.F.,(4,3,3,
3,3,3,3,4),(0.,0.000338425381540912,0.0224866539540187,0.045452247155042,
0.0654166068739022,0.0935951529420607,0.122883934914188,0.150189106809355),
 .UNSPECIFIED.);
#460=B_SPLINE_CURVE_WITH_KNOTS('',3,(#57612,#57613,#57614,#57615,#57616,
#57617,#57618,#57619,#57620,#57621,#57622,#57623,#57624,#57625,#57626,#57627,
#57628,#57629,#57630),.UNSPECIFIED.,.F.,.F.,(4,3,3,3,3,3,4),(-43.1750541323635,
-42.5252748288759,-42.2003851771321,-41.5506058736444,-41.2257162219006,
-40.575936918413,-40.2510472666692),.UNSPECIFIED.);
#461=B_SPLINE_CURVE_WITH_KNOTS('',3,(#57632,#57633,#57634,#57635,#57636,
#57637),.UNSPECIFIED.,.F.,.F.,(4,2,4),(0.134768241793669,0.16617963596043,
0.185292243031058),.UNSPECIFIED.);
#462=B_SPLINE_CURVE_WITH_KNOTS('',3,(#57638,#57639,#57640,#57641,#57642,
#57643),.UNSPECIFIED.,.F.,.F.,(4,2,4),(0.970784459515729,0.997055295420078,
1.03386954271643),.UNSPECIFIED.);
#463=B_SPLINE_CURVE_WITH_KNOTS('',3,(#57647,#57648,#57649,#57650),
 .UNSPECIFIED.,.F.,.F.,(4,4),(0.705578480917695,0.742911382707452),
 .UNSPECIFIED.);
#464=B_SPLINE_CURVE_WITH_KNOTS('',3,(#57651,#57652,#57653,#57654,#57655,
#57656),.UNSPECIFIED.,.F.,.F.,(4,2,4),(0.490224693667975,0.498523894319622,
0.54050457124268),.UNSPECIFIED.);
#465=B_SPLINE_CURVE_WITH_KNOTS('',3,(#57658,#57659,#57660,#57661),
 .UNSPECIFIED.,.F.,.F.,(4,4),(0.686256720735745,0.723216288120665),
 .UNSPECIFIED.);
#466=B_SPLINE_CURVE_WITH_KNOTS('',3,(#57662,#57663,#57664,#57665),
 .UNSPECIFIED.,.F.,.F.,(4,4),(0.518163743605581,0.562900565143627),
 .UNSPECIFIED.);
#467=B_SPLINE_CURVE_WITH_KNOTS('',3,(#57668,#57669,#57670,#57671),
 .UNSPECIFIED.,.F.,.F.,(4,4),(1.28135134421279,1.31862990715387),
 .UNSPECIFIED.);
#468=B_SPLINE_CURVE_WITH_KNOTS('',3,(#57673,#57674,#57675,#57676,#57677,
#57678,#57679,#57680,#57681),.UNSPECIFIED.,.F.,.F.,(4,1,1,1,1,1,4),(55.1638586060211,
55.4429246232081,56.0685764469255,56.3814023587843,57.0070541825018,57.3198800943605,
57.9305195965772),.UNSPECIFIED.);
#469=B_SPLINE_CURVE_WITH_KNOTS('',3,(#57682,#57683,#57684,#57685),
 .UNSPECIFIED.,.F.,.F.,(4,4),(1.26160163394232,1.29910180138512),
 .UNSPECIFIED.);
#470=B_SPLINE_CURVE_WITH_KNOTS('',3,(#57735,#57736,#57737,#57738,#57739,
#57740,#57741,#57742,#57743,#57744,#57745,#57746,#57747,#57748,#57749,#57750),
 .UNSPECIFIED.,.F.,.F.,(4,3,3,3,3,4),(0.,0.000515694897373992,0.0418024345464061,
0.0635027671358636,0.106468605792955,0.124601478701958),.UNSPECIFIED.);
#471=B_SPLINE_CURVE_WITH_KNOTS('',3,(#57752,#57753,#57754,#57755,#57756,
#57757,#57758,#57759,#57760,#57761,#57762,#57763,#57764,#57765,#57766,#57767,
#57768,#57769,#57770),.UNSPECIFIED.,.F.,.F.,(4,3,3,3,3,3,4),(-46.290776864183,
-45.6651250404655,-45.3522991286068,-44.7266473048893,-44.4138213930306,
-43.7881695693131,-43.4753436574544),.UNSPECIFIED.);
#472=B_SPLINE_CURVE_WITH_KNOTS('',3,(#57771,#57772,#57773,#57774,#57775,
#57776,#57777,#57778,#57779,#57780,#57781,#57782,#57783),.UNSPECIFIED.,
 .F.,.F.,(4,3,3,3,4),(0.,0.0393665545192843,0.0589812601558904,0.101040205845147,
0.118470175365851),.UNSPECIFIED.);
#473=B_SPLINE_CURVE_WITH_KNOTS('',3,(#57826,#57827,#57828,#57829,#57830,
#57831),.UNSPECIFIED.,.F.,.F.,(4,2,4),(0.805938743676149,0.830541752976356,
0.840481356535727),.UNSPECIFIED.);
#474=B_SPLINE_CURVE_WITH_KNOTS('',3,(#57838,#57839,#57840,#57841),
 .UNSPECIFIED.,.F.,.F.,(4,4),(1.16287000320261,1.19712104343039),
 .UNSPECIFIED.);
#475=B_SPLINE_CURVE_WITH_KNOTS('',3,(#57842,#57843,#57844,#57845),
 .UNSPECIFIED.,.F.,.F.,(4,4),(-0.0717727639817645,-0.0462671248394357),
 .UNSPECIFIED.);
#476=B_SPLINE_CURVE_WITH_KNOTS('',3,(#57855,#57856,#57857,#57858,#57859,
#57860),.UNSPECIFIED.,.F.,.F.,(4,2,4),(0.332215634323022,0.415268209319378,
0.418708545872871),.UNSPECIFIED.);
#477=B_SPLINE_CURVE_WITH_KNOTS('',3,(#57861,#57862,#57863,#57864),
 .UNSPECIFIED.,.F.,.F.,(4,4),(0.255235312149345,0.332215634323022),
 .UNSPECIFIED.);
#478=B_SPLINE_CURVE_WITH_KNOTS('',3,(#57865,#57866,#57867,#57868),
 .UNSPECIFIED.,.F.,.F.,(4,4),(0.517942109132407,0.546042694596367),
 .UNSPECIFIED.);
#479=B_SPLINE_CURVE_WITH_KNOTS('',3,(#57870,#57871,#57872,#57873),
 .UNSPECIFIED.,.F.,.F.,(4,4),(0.701030951378668,0.726642077695294),
 .UNSPECIFIED.);
#480=B_SPLINE_CURVE_WITH_KNOTS('',3,(#57874,#57875,#57876,#57877),
 .UNSPECIFIED.,.F.,.F.,(4,4),(0.621839088202796,0.647297338681728),
 .UNSPECIFIED.);
#481=B_SPLINE_CURVE_WITH_KNOTS('',3,(#57879,#57880,#57881,#57882),
 .UNSPECIFIED.,.F.,.F.,(4,4),(0.0269607932098941,0.052218921738027),
 .UNSPECIFIED.);
#482=B_SPLINE_CURVE_WITH_KNOTS('',3,(#57884,#57885,#57886,#57887),
 .UNSPECIFIED.,.F.,.F.,(4,4),(0.108777077446072,0.139263533037876),
 .UNSPECIFIED.);
#483=B_SPLINE_CURVE_WITH_KNOTS('',3,(#58080,#58081,#58082,#58083,#58084,
#58085,#58086,#58087,#58088,#58089,#58090,#58091,#58092,#58093,#58094,#58095,
#58096,#58097,#58098,#58099,#58100,#58101,#58102,#58103,#58104,#58105,#58106,
#58107),.UNSPECIFIED.,.F.,.F.,(4,2,2,2,2,2,2,2,2,2,2,2,2,4),(0.000552255324501238,
0.00250712865869175,0.00542730315934362,0.0100897003910396,0.0208199668277967,
0.03914332528473,0.0566413877982004,0.0737548216775457,0.0916180344917143,
0.113112730500366,0.124811949413757,0.129415141422697,0.131466822655317,
0.132736838801192),.UNSPECIFIED.);
#484=B_SPLINE_CURVE_WITH_KNOTS('',3,(#58116,#58117,#58118,#58119),
 .UNSPECIFIED.,.F.,.F.,(4,4),(0.973845213090798,1.86224631803132),
 .UNSPECIFIED.);
#485=B_SPLINE_CURVE_WITH_KNOTS('',3,(#58124,#58125,#58126,#58127),
 .UNSPECIFIED.,.F.,.F.,(4,4),(1.01459402224647,1.90299512718699),
 .UNSPECIFIED.);
#486=B_SPLINE_CURVE_WITH_KNOTS('',3,(#58132,#58133,#58134,#58135,#58136,
#58137,#58138,#58139,#58140,#58141,#58142,#58143,#58144,#58145,#58146,#58147,
#58148,#58149,#58150,#58151,#58152,#58153,#58154,#58155,#58156,#58157,#58158,
#58159,#58160),.UNSPECIFIED.,.F.,.F.,(4,3,2,2,2,2,2,2,2,2,2,2,2,4),(0.220457494411324,
0.221514163345612,0.224063974278064,0.227827813747527,0.235231812673064,
0.248804927504688,0.261986328480532,0.275641459334015,0.28913004114437,
0.303381192089668,0.310291199891665,0.313709542902219,0.316059908336669,
0.316319431229452),.UNSPECIFIED.);
#487=B_SPLINE_CURVE_WITH_KNOTS('',3,(#58166,#58167,#58168,#58169,#58170,
#58171,#58172,#58173,#58174,#58175,#58176,#58177,#58178,#58179,#58180,#58181,
#58182,#58183,#58184,#58185,#58186,#58187,#58188,#58189,#58190,#58191,#58192,
#58193,#58194,#58195,#58196,#58197),.UNSPECIFIED.,.F.,.F.,(4,2,2,2,2,2,
2,2,2,2,2,2,2,2,2,4),(0.000552255618180187,0.00250735066624725,0.00544388471025156,
0.010201420453688,0.022077523574172,0.0441976068676189,0.055996906725916,
0.0645228057028066,0.0728085455699138,0.0835882268125382,0.102795441848339,
0.125000410030466,0.136058920133137,0.140727854440821,0.142845621851799,
0.144031712293079),.UNSPECIFIED.);
#488=B_SPLINE_CURVE_WITH_KNOTS('',3,(#58206,#58207,#58208,#58209),
 .UNSPECIFIED.,.F.,.F.,(4,4),(1.01302199639782,1.90133038588088),
 .UNSPECIFIED.);
#489=B_SPLINE_CURVE_WITH_KNOTS('',3,(#58214,#58215,#58216,#58217),
 .UNSPECIFIED.,.F.,.F.,(4,4),(1.01910936201615,1.90741775149922),
 .UNSPECIFIED.);
#490=B_SPLINE_CURVE_WITH_KNOTS('',3,(#58222,#58223,#58224,#58225,#58226,
#58227,#58228,#58229,#58230,#58231,#58232,#58233,#58234,#58235,#58236,#58237,
#58238,#58239,#58240,#58241,#58242,#58243,#58244,#58245,#58246,#58247,#58248,
#58249,#58250,#58251,#58252,#58253,#58254),.UNSPECIFIED.,.F.,.F.,(4,3,2,
2,2,2,2,2,2,2,2,2,2,2,2,4),(0.196959320052513,0.198017145092129,0.200540880261076,
0.20420524906308,0.212045863749151,0.231522357859952,0.239816668297063,
0.245036313836856,0.249558567699146,0.254824767282906,0.263328140173216,
0.280727522166969,0.28716729720564,0.290158226145309,0.292204134755108,
0.292205277806419),.UNSPECIFIED.);
#491=B_SPLINE_CURVE_WITH_KNOTS('',3,(#58260,#58261,#58262,#58263,#58264,
#58265,#58266,#58267,#58268,#58269,#58270,#58271,#58272,#58273,#58274,#58275,
#58276,#58277,#58278,#58279,#58280,#58281,#58282,#58283,#58284,#58285,#58286,
#58287,#58288,#58289,#58290,#58291),.UNSPECIFIED.,.F.,.F.,(4,2,2,2,2,2,
2,2,2,2,2,2,2,2,2,4),(0.000552255618326259,0.00250735068795714,0.00544388481129021,
0.0102014206832928,0.0220775241250821,0.0441976080155335,0.0559969081923875,
0.0645228073995753,0.0728085474906832,0.0835882290248828,0.102795444580419,
0.125000413363,0.136058923763291,0.140727858196649,0.142845625664765,0.144031716095406),
 .UNSPECIFIED.);
#492=B_SPLINE_CURVE_WITH_KNOTS('',3,(#58300,#58301,#58302,#58303),
 .UNSPECIFIED.,.F.,.F.,(4,4),(1.02924883146194,1.91752828913416),
 .UNSPECIFIED.);
#493=B_SPLINE_CURVE_WITH_KNOTS('',3,(#58308,#58309,#58310,#58311),
 .UNSPECIFIED.,.F.,.F.,(4,4),(1.020135190352,1.90841464802423),
 .UNSPECIFIED.);
#494=B_SPLINE_CURVE_WITH_KNOTS('',3,(#58316,#58317,#58318,#58319,#58320,
#58321,#58322,#58323,#58324,#58325,#58326,#58327,#58328,#58329,#58330,#58331,
#58332,#58333,#58334,#58335,#58336,#58337,#58338,#58339,#58340,#58341,#58342,
#58343,#58344,#58345,#58346,#58347,#58348),.UNSPECIFIED.,.F.,.F.,(4,3,2,
2,2,2,2,2,2,2,2,2,2,2,2,4),(0.196959320035475,0.198017145075089,0.200540880244035,
0.204205249046031,0.212045863731981,0.231522357842223,0.239816668279115,
0.245036313818745,0.249558567680855,0.254824767264382,0.263328140154285,
0.28072752214711,0.287167297185208,0.290158226124563,0.292204134734147,
0.292205277785457),.UNSPECIFIED.);
#495=B_SPLINE_CURVE_WITH_KNOTS('',3,(#58354,#58355,#58356,#58357,#58358,
#58359,#58360,#58361,#58362,#58363,#58364,#58365,#58366,#58367,#58368,#58369,
#58370,#58371,#58372,#58373,#58374,#58375,#58376,#58377,#58378,#58379,#58380,
#58381,#58382,#58383,#58384,#58385),.UNSPECIFIED.,.F.,.F.,(4,2,2,2,2,2,
2,2,2,2,2,2,2,2,2,4),(0.000552255618176519,0.00250735066570793,0.00544388470773694,
0.0102014204479581,0.0220775235604603,0.0441976068391316,0.0559969066895389,
0.0645228056607815,0.0728085455224931,0.0835882267580784,0.102795441781326,
0.125000409948151,0.136058920042637,0.140727854346809,0.142845621756309,
0.14403171221705),.UNSPECIFIED.);
#496=B_SPLINE_CURVE_WITH_KNOTS('',3,(#58394,#58395,#58396,#58397),
 .UNSPECIFIED.,.F.,.F.,(4,4),(0.992149273556617,1.8805029517096),
 .UNSPECIFIED.);
#497=B_SPLINE_CURVE_WITH_KNOTS('',3,(#58402,#58403,#58404,#58405),
 .UNSPECIFIED.,.F.,.F.,(4,4),(1.01721488555274,1.90556856370572),
 .UNSPECIFIED.);
#498=B_SPLINE_CURVE_WITH_KNOTS('',3,(#58410,#58411,#58412,#58413,#58414,
#58415,#58416,#58417,#58418,#58419,#58420,#58421,#58422,#58423,#58424,#58425,
#58426,#58427,#58428,#58429,#58430,#58431,#58432,#58433,#58434,#58435,#58436,
#58437,#58438),.UNSPECIFIED.,.F.,.F.,(4,3,2,2,2,2,2,2,2,2,2,2,2,4),(0.244877808035713,
0.245941379437421,0.248507773432569,0.2523525700864,0.260140357197957,0.274281958050968,
0.285777166411162,0.296461087015459,0.307606399535247,0.320385682652649,
0.337686825300976,0.344715117359311,0.34902320135799,0.350883558016063),
 .UNSPECIFIED.);
#499=B_SPLINE_CURVE_WITH_KNOTS('',3,(#58444,#58445,#58446,#58447,#58448,
#58449,#58450,#58451,#58452,#58453,#58454,#58455,#58456,#58457,#58458,#58459,
#58460,#58461,#58462,#58463,#58464,#58465,#58466,#58467,#58468,#58469,#58470,
#58471),.UNSPECIFIED.,.F.,.F.,(4,2,2,2,2,2,2,2,2,2,2,2,2,4),(0.00055225541740831,
0.00250719881231768,0.0054323728801237,0.0101226773987657,0.0211144007255414,
0.0395050112937957,0.0554921421757053,0.0705100097030702,0.0866125226194124,
0.105123282533283,0.115750637514577,0.119917613254093,0.121610784601848,
0.122782730208698),.UNSPECIFIED.);
#500=B_SPLINE_CURVE_WITH_KNOTS('',3,(#58480,#58481,#58482,#58483),
 .UNSPECIFIED.,.F.,.F.,(4,4),(0.960106131022675,1.84854766340329),
 .UNSPECIFIED.);
#501=B_SPLINE_CURVE_WITH_KNOTS('',3,(#58488,#58489,#58490,#58491),
 .UNSPECIFIED.,.F.,.F.,(4,4),(1.0115487697186,1.89999030209922),
 .UNSPECIFIED.);
#502=B_SPLINE_CURVE_WITH_KNOTS('',3,(#58496,#58497,#58498,#58499,#58500,
#58501,#58502,#58503,#58504,#58505,#58506,#58507,#58508,#58509,#58510,#58511,
#58512,#58513,#58514,#58515,#58516,#58517,#58518,#58519,#58520,#58521,#58522),
 .UNSPECIFIED.,.F.,.F.,(4,3,2,2,2,2,2,2,2,2,2,2,4),(0.232932117987348,0.233989323147965,
0.236545962444758,0.24033528190873,0.247744949647774,0.261894911831567,
0.277641329371112,0.294641376545692,0.309755553896968,0.323519464298202,
0.330173674908094,0.334332814154483,0.336361587070415),.UNSPECIFIED.);
#503=B_SPLINE_CURVE_WITH_KNOTS('',3,(#58528,#58529,#58530,#58531,#58532,
#58533,#58534,#58535,#58536,#58537,#58538,#58539,#58540,#58541,#58542,#58543,
#58544,#58545,#58546,#58547,#58548,#58549,#58550,#58551,#58552,#58553,#58554,
#58555),.UNSPECIFIED.,.F.,.F.,(4,2,2,2,2,2,2,2,2,2,2,2,2,4),(0.000552255417408364,
0.00250719881231768,0.00543237288013685,0.0101226773988465,0.0211144007254288,
0.0395050112923411,0.0554921421730382,0.0705100096993886,0.0866125226146962,
0.105123282527376,0.115750637508154,0.119917613246771,0.121610784594084,
0.122782730200613),.UNSPECIFIED.);
#504=B_SPLINE_CURVE_WITH_KNOTS('',3,(#58564,#58565,#58566,#58567),
 .UNSPECIFIED.,.F.,.F.,(4,4),(0.960106131022676,1.84854766340329),
 .UNSPECIFIED.);
#505=B_SPLINE_CURVE_WITH_KNOTS('',3,(#58572,#58573,#58574,#58575),
 .UNSPECIFIED.,.F.,.F.,(4,4),(1.0115487697186,1.89999030209922),
 .UNSPECIFIED.);
#506=B_SPLINE_CURVE_WITH_KNOTS('',3,(#58580,#58581,#58582,#58583,#58584,
#58585,#58586,#58587,#58588,#58589,#58590,#58591,#58592,#58593,#58594,#58595,
#58596,#58597,#58598,#58599,#58600,#58601,#58602,#58603,#58604,#58605,#58606),
 .UNSPECIFIED.,.F.,.F.,(4,3,2,2,2,2,2,2,2,2,2,2,4),(0.232932117990906,0.233989323151543,
0.236545962448293,0.240335281912072,0.247744949650985,0.261894911834848,
0.277641329374929,0.294641376550107,0.309755553901947,0.323519464303881,
0.330173674914252,0.334332814160932,0.33636158707699),.UNSPECIFIED.);
#507=B_SPLINE_CURVE_WITH_KNOTS('',3,(#58612,#58613,#58614,#58615,#58616,
#58617,#58618,#58619,#58620,#58621,#58622,#58623,#58624,#58625,#58626,#58627,
#58628,#58629,#58630,#58631,#58632,#58633,#58634,#58635,#58636,#58637,#58638,
#58639,#58640,#58641,#58642,#58643),.UNSPECIFIED.,.F.,.F.,(4,2,2,2,2,2,
2,2,2,2,2,2,2,2,2,4),(0.000552255618199786,0.00250735066915548,0.00544388472378785,
0.0102014204844693,0.0220775236482432,0.0441976070226107,0.0559969069240703,
0.0645228059321239,0.0728085458295457,0.0835882271116238,0.102795442217763,
0.125000410480877,0.136058920623433,0.140727854947894,0.142845622366623,
0.144031712827498),.UNSPECIFIED.);
#508=B_SPLINE_CURVE_WITH_KNOTS('',3,(#58652,#58653,#58654,#58655),
 .UNSPECIFIED.,.F.,.F.,(4,4),(0.992149273556618,1.8805029517096),
 .UNSPECIFIED.);
#509=B_SPLINE_CURVE_WITH_KNOTS('',3,(#58660,#58661,#58662,#58663),
 .UNSPECIFIED.,.F.,.F.,(4,4),(1.01721488555274,1.90556856370572),
 .UNSPECIFIED.);
#510=B_SPLINE_CURVE_WITH_KNOTS('',3,(#58668,#58669,#58670,#58671,#58672,
#58673,#58674,#58675,#58676,#58677,#58678,#58679,#58680,#58681,#58682,#58683,
#58684,#58685,#58686,#58687,#58688,#58689,#58690,#58691,#58692,#58693,#58694,
#58695,#58696),.UNSPECIFIED.,.F.,.F.,(4,3,2,2,2,2,2,2,2,2,2,2,2,4),(0.244877808040074,
0.24594137944178,0.248507773436917,0.25235257009068,0.260140357202121,0.274281958055093,
0.285777166415387,0.296461087019819,0.307606399539854,0.320385682657535,
0.337686825306311,0.3447151173649,0.349023201363699,0.350883558021839),
 .UNSPECIFIED.);
#511=B_SPLINE_CURVE_WITH_KNOTS('',3,(#58702,#58703,#58704,#58705,#58706,
#58707,#58708,#58709,#58710,#58711,#58712,#58713,#58714,#58715,#58716,#58717,
#58718,#58719,#58720,#58721,#58722,#58723,#58724,#58725,#58726,#58727,#58728,
#58729,#58730,#58731,#58732,#58733),.UNSPECIFIED.,.F.,.F.,(4,2,2,2,2,2,
2,2,2,2,2,2,2,2,2,4),(0.000552255618307427,0.00250735068515379,0.00544388479824744,
0.0102014206536779,0.0220775240540609,0.0441976078674591,0.0559969080032229,
0.0645228071807259,0.0728085472428637,0.0835882287392999,0.102795444227548,
0.125000412932329,0.136058923294133,0.14072785771123,0.142845625171944,
0.144031715617256),.UNSPECIFIED.);
#512=B_SPLINE_CURVE_WITH_KNOTS('',3,(#58742,#58743,#58744,#58745),
 .UNSPECIFIED.,.F.,.F.,(4,4),(1.02924883146194,1.91752828913416),
 .UNSPECIFIED.);
#513=B_SPLINE_CURVE_WITH_KNOTS('',3,(#58750,#58751,#58752,#58753),
 .UNSPECIFIED.,.F.,.F.,(4,4),(1.020135190352,1.90841464802423),
 .UNSPECIFIED.);
#514=B_SPLINE_CURVE_WITH_KNOTS('',3,(#58758,#58759,#58760,#58761,#58762,
#58763,#58764,#58765,#58766,#58767,#58768,#58769,#58770,#58771,#58772,#58773,
#58774,#58775,#58776,#58777,#58778,#58779,#58780,#58781,#58782,#58783,#58784,
#58785,#58786,#58787,#58788,#58789,#58790),.UNSPECIFIED.,.F.,.F.,(4,3,2,
2,2,2,2,2,2,2,2,2,2,2,2,4),(0.196959320035786,0.198017145075391,0.20054088024434,
0.204205249046347,0.21204586373224,0.231522357841158,0.239816668277358,
0.24503631381662,0.249558567678421,0.254824767261635,0.263328140151098,
0.280727522143284,0.287167297181241,0.290158226120517,0.292204134730046,
0.292205277781356),.UNSPECIFIED.);
#515=B_SPLINE_CURVE_WITH_KNOTS('',3,(#58796,#58797,#58798,#58799,#58800,
#58801,#58802,#58803,#58804,#58805,#58806,#58807,#58808,#58809,#58810,#58811,
#58812,#58813,#58814,#58815,#58816,#58817,#58818,#58819,#58820,#58821,#58822,
#58823,#58824,#58825,#58826,#58827),.UNSPECIFIED.,.F.,.F.,(4,2,2,2,2,2,
2,2,2,2,2,2,2,2,2,4),(0.000552255618140622,0.00250735066035639,0.00544388468282173,
0.0102014203913002,0.0220775234245199,0.0441976065560588,0.0559969063279555,
0.064522805242411,0.0728085450487638,0.0835882262122293,0.102795441107005,
0.125000409125109,0.136058919145561,0.140727853418389,0.142845620813663,
0.144031711309052),.UNSPECIFIED.);
#516=B_SPLINE_CURVE_WITH_KNOTS('',3,(#58836,#58837,#58838,#58839),
 .UNSPECIFIED.,.F.,.F.,(4,4),(1.01302199639782,1.90133038588089),
 .UNSPECIFIED.);
#517=B_SPLINE_CURVE_WITH_KNOTS('',3,(#58844,#58845,#58846,#58847),
 .UNSPECIFIED.,.F.,.F.,(4,4),(1.01910936201615,1.90741775149922),
 .UNSPECIFIED.);
#518=B_SPLINE_CURVE_WITH_KNOTS('',3,(#58852,#58853,#58854,#58855,#58856,
#58857,#58858,#58859,#58860,#58861,#58862,#58863,#58864,#58865,#58866,#58867,
#58868,#58869,#58870,#58871,#58872,#58873,#58874,#58875,#58876,#58877,#58878,
#58879,#58880,#58881,#58882,#58883,#58884),.UNSPECIFIED.,.F.,.F.,(4,3,2,
2,2,2,2,2,2,2,2,2,2,2,2,4),(0.196959320037348,0.198017145076955,0.200540880245902,
0.204205249047899,0.212045863733824,0.231522357843424,0.239816668280005,
0.245036313819491,0.249558567681539,0.254824767264985,0.263328140154792,
0.280727522147479,0.287167297185466,0.290158226124763,0.292204134734313,
0.292205277785624),.UNSPECIFIED.);
#519=B_SPLINE_CURVE_WITH_KNOTS('',3,(#58890,#58891,#58892,#58893,#58894,
#58895,#58896,#58897,#58898,#58899,#58900,#58901,#58902,#58903,#58904,#58905,
#58906,#58907,#58908,#58909,#58910,#58911,#58912,#58913,#58914,#58915,#58916,
#58917),.UNSPECIFIED.,.F.,.F.,(4,2,2,2,2,2,2,2,2,2,2,2,2,4),(0.000552255324449124,
0.0025071286509707,0.00542730312346706,0.0100897003100863,0.0208199666431741,
0.0391433249235541,0.0566413872684798,0.0737548209829379,0.0916180336249932,
0.113112729425786,0.124811948226245,0.129415140189881,0.131466821402301,
0.132736837572989),.UNSPECIFIED.);
#520=B_SPLINE_CURVE_WITH_KNOTS('',3,(#58926,#58927,#58928,#58929),
 .UNSPECIFIED.,.F.,.F.,(4,4),(0.973845213090799,1.86224631803132),
 .UNSPECIFIED.);
#521=B_SPLINE_CURVE_WITH_KNOTS('',3,(#58934,#58935,#58936,#58937),
 .UNSPECIFIED.,.F.,.F.,(4,4),(1.01459402224647,1.90299512718699),
 .UNSPECIFIED.);
#522=B_SPLINE_CURVE_WITH_KNOTS('',3,(#58942,#58943,#58944,#58945,#58946,
#58947,#58948,#58949,#58950,#58951,#58952,#58953,#58954,#58955,#58956,#58957,
#58958,#58959,#58960,#58961,#58962,#58963,#58964,#58965,#58966,#58967,#58968,
#58969,#58970),.UNSPECIFIED.,.F.,.F.,(4,3,2,2,2,2,2,2,2,2,2,2,2,4),(0.220457494407796,
0.221514163342054,0.224063974274498,0.227827813743946,0.235231812669523,
0.248804927500911,0.26198632847626,0.275641459329111,0.289130041138783,
0.303381192083739,0.310291199885813,0.313709542896337,0.316059908330814,
0.316319431223601),.UNSPECIFIED.);
#523=B_SPLINE_CURVE_WITH_KNOTS('',3,(#58976,#58977,#58978,#58979,#58980,
#58981,#58982,#58983,#58984,#58985,#58986,#58987,#58988,#58989,#58990,#58991),
 .UNSPECIFIED.,.F.,.F.,(4,2,2,2,2,2,2,4),(0.000552255452524527,0.0025072256329463,
0.00543435587026899,0.010135846530597,0.0212263042677829,0.0396611687049569,
0.0549611368371748,0.0626032386529709),.UNSPECIFIED.);
#524=B_SPLINE_CURVE_WITH_KNOTS('',3,(#58999,#59000,#59001,#59002,#59003,
#59004,#59005,#59006,#59007,#59008,#59009,#59010,#59011,#59012,#59013,#59014),
 .UNSPECIFIED.,.F.,.F.,(4,2,2,2,2,2,2,4),(0.0626032386529709,0.0690038332396629,
0.0841023648099793,0.102253718460132,0.114574293882771,0.118850101323579,
0.120613951052394,0.121845703091679),.UNSPECIFIED.);
#525=B_SPLINE_CURVE_WITH_KNOTS('',3,(#59017,#59018,#59019,#59020),
 .UNSPECIFIED.,.F.,.F.,(4,4),(0.952234974413515,1.84070284457626),
 .UNSPECIFIED.);
#526=B_SPLINE_CURVE_WITH_KNOTS('',3,(#59025,#59026,#59027,#59028),
 .UNSPECIFIED.,.F.,.F.,(4,4),(1.00739097317572,1.89585884333848),
 .UNSPECIFIED.);
#527=B_SPLINE_CURVE_WITH_KNOTS('',3,(#59034,#59035,#59036,#59037,#59038,
#59039,#59040,#59041,#59042,#59043,#59044,#59045,#59046,#59047,#59048,#59049),
 .UNSPECIFIED.,.F.,.F.,(4,2,2,2,2,2,2,4),(0.265850124074439,0.273928386135499,
0.284993617049668,0.300677807852058,0.308332988403192,0.3136252683209,0.316793712699132,
0.318373416046925),.UNSPECIFIED.);
#528=B_SPLINE_CURVE_WITH_KNOTS('',3,(#59050,#59051,#59052,#59053,#59054,
#59055,#59056,#59057,#59058,#59059,#59060,#59061,#59062,#59063,#59064,#59065,
#59066,#59067,#59068),.UNSPECIFIED.,.F.,.F.,(4,3,2,2,2,2,2,2,4),(0.214188423781497,
0.215245209126414,0.217829605846206,0.221760415278908,0.229921784182885,
0.245839020956828,0.256431324628773,0.265077654336287,0.265850124074439),
 .UNSPECIFIED.);
#529=B_SPLINE_CURVE_WITH_KNOTS('',3,(#59074,#59075,#59076,#59077,#59078,
#59079,#59080,#59081,#59082,#59083,#59084,#59085,#59086,#59087,#59088,#59089,
#59090,#59091,#59092,#59093,#59094,#59095,#59096,#59097,#59098,#59099,#59100,
#59101),.UNSPECIFIED.,.F.,.F.,(4,2,2,2,2,2,2,2,2,2,2,2,2,4),(0.000552255324103493,
0.00250712859975242,0.00542730288565579,0.0100896997742742,0.0208199654208688,
0.039143322528832,0.0566413837541626,0.0737548163735086,0.0916180278724114,
0.113112722297835,0.124811940352812,0.129415132021259,0.131466813102152,
0.132736829274288),.UNSPECIFIED.);
#530=B_SPLINE_CURVE_WITH_KNOTS('',3,(#59110,#59111,#59112,#59113),
 .UNSPECIFIED.,.F.,.F.,(4,4),(0.973845213090798,1.86224631803132),
 .UNSPECIFIED.);
#531=B_SPLINE_CURVE_WITH_KNOTS('',3,(#59118,#59119,#59120,#59121),
 .UNSPECIFIED.,.F.,.F.,(4,4),(1.01459402224647,1.90299512718699),
 .UNSPECIFIED.);
#532=B_SPLINE_CURVE_WITH_KNOTS('',3,(#59126,#59127,#59128,#59129,#59130,
#59131,#59132,#59133,#59134,#59135,#59136,#59137,#59138,#59139,#59140,#59141,
#59142,#59143,#59144,#59145,#59146,#59147,#59148,#59149,#59150,#59151,#59152,
#59153,#59154),.UNSPECIFIED.,.F.,.F.,(4,3,2,2,2,2,2,2,2,2,2,2,2,4),(0.220457494412775,
0.221514163347042,0.224063974279508,0.227827813749052,0.235231812674751,
0.248804927506449,0.261986328482189,0.275641459335547,0.289130041145789,
0.303381192091107,0.310291199893207,0.313709542903786,0.316059908338292,
0.316319431231083),.UNSPECIFIED.);
#533=B_SPLINE_CURVE_WITH_KNOTS('',3,(#59160,#59161,#59162,#59163,#59164,
#59165,#59166,#59167,#59168,#59169,#59170,#59171,#59172,#59173,#59174,#59175,
#59176,#59177,#59178,#59179,#59180,#59181,#59182,#59183,#59184,#59185,#59186,
#59187,#59188,#59189,#59190,#59191),.UNSPECIFIED.,.F.,.F.,(4,2,2,2,2,2,
2,2,2,2,2,2,2,2,2,4),(0.000552255618150325,0.00250735066180447,0.00544388468956596,
0.010201420406642,0.0220775234613036,0.0441976066326517,0.055996906425799,
0.0645228053555453,0.0728085451768181,0.0835882263598216,0.102795441289329,
0.125000409347919,0.13605891938857,0.140727853669976,0.142845621069164,
0.144031711509465),.UNSPECIFIED.);
#534=B_SPLINE_CURVE_WITH_KNOTS('',3,(#59200,#59201,#59202,#59203),
 .UNSPECIFIED.,.F.,.F.,(4,4),(1.01302199639782,1.90133038588089),
 .UNSPECIFIED.);
#535=B_SPLINE_CURVE_WITH_KNOTS('',3,(#59208,#59209,#59210,#59211),
 .UNSPECIFIED.,.F.,.F.,(4,4),(1.01910936201615,1.90741775149922),
 .UNSPECIFIED.);
#536=B_SPLINE_CURVE_WITH_KNOTS('',3,(#59216,#59217,#59218,#59219,#59220,
#59221,#59222,#59223,#59224,#59225,#59226,#59227,#59228,#59229,#59230,#59231,
#59232,#59233,#59234,#59235,#59236,#59237,#59238,#59239,#59240,#59241,#59242,
#59243,#59244,#59245,#59246,#59247,#59248),.UNSPECIFIED.,.F.,.F.,(4,3,2,
2,2,2,2,2,2,2,2,2,2,2,2,4),(0.196959320041271,0.19801714508091,0.200540880249857,
0.204205249051859,0.212045863737848,0.231522357847912,0.239816668284666,
0.245036313824251,0.249558567686326,0.254824767269862,0.263328140159838,
0.280727522153003,0.287167297191319,0.290158226130778,0.29220413474042,
0.292205277791729),.UNSPECIFIED.);
#537=B_SPLINE_CURVE_WITH_KNOTS('',3,(#59254,#59255,#59256,#59257,#59258,
#59259,#59260,#59261,#59262,#59263,#59264,#59265,#59266,#59267,#59268,#59269,
#59270,#59271,#59272,#59273,#59274,#59275,#59276,#59277,#59278,#59279,#59280,
#59281,#59282,#59283,#59284,#59285),.UNSPECIFIED.,.F.,.F.,(4,2,2,2,2,2,
2,2,2,2,2,2,2,2,2,4),(0.000552255618256276,0.00250735067755829,0.00544388476289,
0.0102014205732942,0.0220775238611849,0.0441976074657267,0.0559969074900062,
0.0645228065868935,0.0728085465706407,0.0835882279650627,0.102795443271529,
0.125000411766022,0.136058922023308,0.140727856396235,0.142845623836849,
0.14403171428955),.UNSPECIFIED.);
#538=B_SPLINE_CURVE_WITH_KNOTS('',3,(#59294,#59295,#59296,#59297),
 .UNSPECIFIED.,.F.,.F.,(4,4),(1.02924883146194,1.91752828913416),
 .UNSPECIFIED.);
#539=B_SPLINE_CURVE_WITH_KNOTS('',3,(#59302,#59303,#59304,#59305),
 .UNSPECIFIED.,.F.,.F.,(4,4),(1.020135190352,1.90841464802423),
 .UNSPECIFIED.);
#540=B_SPLINE_CURVE_WITH_KNOTS('',3,(#59310,#59311,#59312,#59313,#59314,
#59315,#59316,#59317,#59318,#59319,#59320,#59321,#59322,#59323,#59324,#59325,
#59326,#59327,#59328,#59329,#59330,#59331,#59332,#59333,#59334,#59335,#59336,
#59337,#59338,#59339,#59340,#59341,#59342),.UNSPECIFIED.,.F.,.F.,(4,3,2,
2,2,2,2,2,2,2,2,2,2,2,2,4),(0.196959320024652,0.198017145064251,0.200540880233189,
0.204205249035151,0.212045863720946,0.231522357830115,0.239816668266482,
0.245036313805818,0.249558567667623,0.254824767250817,0.263328140140195,
0.280727522132095,0.287167297169923,0.290158226109145,0.292204134718638,
0.292205277769948),.UNSPECIFIED.);
#541=B_SPLINE_CURVE_WITH_KNOTS('',3,(#59348,#59349,#59350,#59351,#59352,
#59353,#59354,#59355,#59356,#59357,#59358,#59359,#59360,#59361,#59362,#59363,
#59364,#59365,#59366,#59367,#59368,#59369,#59370,#59371,#59372,#59373,#59374,
#59375,#59376,#59377,#59378,#59379),.UNSPECIFIED.,.F.,.F.,(4,2,2,2,2,2,
2,2,2,2,2,2,2,2,2,4),(0.000552255618195755,0.00250735066855508,0.00544388472099276,
0.0102014204781084,0.0220775236328774,0.0441976069902035,0.055996906882568,
0.0645228058841012,0.0728085457752267,0.0835882270490723,0.10279544214055,
0.125000410385944,0.136058920518909,0.140727854839246,0.142845622256129,
0.144031712714974),.UNSPECIFIED.);
#542=B_SPLINE_CURVE_WITH_KNOTS('',3,(#59388,#59389,#59390,#59391),
 .UNSPECIFIED.,.F.,.F.,(4,4),(0.992149273556617,1.8805029517096),
 .UNSPECIFIED.);
#543=B_SPLINE_CURVE_WITH_KNOTS('',3,(#59396,#59397,#59398,#59399),
 .UNSPECIFIED.,.F.,.F.,(4,4),(1.01721488555274,1.90556856370572),
 .UNSPECIFIED.);
#544=B_SPLINE_CURVE_WITH_KNOTS('',3,(#59404,#59405,#59406,#59407,#59408,
#59409,#59410,#59411,#59412,#59413,#59414,#59415,#59416,#59417,#59418,#59419,
#59420,#59421,#59422,#59423,#59424,#59425,#59426,#59427,#59428,#59429,#59430,
#59431,#59432),.UNSPECIFIED.,.F.,.F.,(4,3,2,2,2,2,2,2,2,2,2,2,2,4),(0.244877808035147,
0.245941379436854,0.248507773431997,0.252352570085808,0.260140357197332,
0.274281958050489,0.285777166411083,0.296461087015731,0.307606399535822,
0.32038568265349,0.337686825302001,0.344715117360385,0.349023201359046,
0.350883558017123),.UNSPECIFIED.);
#545=B_SPLINE_CURVE_WITH_KNOTS('',3,(#59438,#59439,#59440,#59441,#59442,
#59443,#59444,#59445,#59446,#59447,#59448,#59449,#59450,#59451,#59452,#59453,
#59454,#59455,#59456,#59457,#59458,#59459,#59460,#59461,#59462,#59463,#59464,
#59465),.UNSPECIFIED.,.F.,.F.,(4,2,2,2,2,2,2,2,2,2,2,2,2,4),(0.000552255417408142,
0.00250719881228533,0.00543237287997538,0.0101226773984433,0.021114400724837,
0.0395050112925363,0.0554921421739572,0.0705100097009322,0.0866125226168388,
0.10512328253025,0.115750637511601,0.119917613252859,0.121610784601703,
0.122782730209295),.UNSPECIFIED.);
#546=B_SPLINE_CURVE_WITH_KNOTS('',3,(#59474,#59475,#59476,#59477),
 .UNSPECIFIED.,.F.,.F.,(4,4),(0.960106131022676,1.84854766340329),
 .UNSPECIFIED.);
#547=B_SPLINE_CURVE_WITH_KNOTS('',3,(#59482,#59483,#59484,#59485),
 .UNSPECIFIED.,.F.,.F.,(4,4),(1.0115487697186,1.89999030209922),
 .UNSPECIFIED.);
#548=B_SPLINE_CURVE_WITH_KNOTS('',3,(#59490,#59491,#59492,#59493,#59494,
#59495,#59496,#59497,#59498,#59499,#59500,#59501,#59502,#59503,#59504,#59505,
#59506,#59507,#59508,#59509,#59510,#59511,#59512,#59513,#59514,#59515,#59516),
 .UNSPECIFIED.,.F.,.F.,(4,3,2,2,2,2,2,2,2,2,2,2,4),(0.232932117998903,0.233989323159604,
0.236545962456403,0.240335281920403,0.247744949659532,0.261894911843477,
0.277641329383194,0.294641376558072,0.309755553909664,0.323519464311306,
0.330173674921484,0.334332814168025,0.336361587084032),.UNSPECIFIED.);
#549=B_SPLINE_CURVE_WITH_KNOTS('',3,(#59522,#59523,#59524,#59525,#59526,
#59527,#59528,#59529,#59530,#59531,#59532,#59533,#59534,#59535,#59536,#59537,
#59538,#59539,#59540,#59541,#59542,#59543,#59544,#59545,#59546,#59547,#59548,
#59549),.UNSPECIFIED.,.F.,.F.,(4,2,2,2,2,2,2,2,2,2,2,2,2,4),(0.000552255417408064,
0.00250719881228644,0.00543237287999154,0.0101226773985182,0.0211144007248477,
0.0395050112920569,0.0554921421730817,0.0705100096996193,0.086612522615075,
0.105123282527957,0.115750637508788,0.119917613246066,0.121610784592526,
0.122782730198486),.UNSPECIFIED.);
#550=B_SPLINE_CURVE_WITH_KNOTS('',3,(#59558,#59559,#59560,#59561),
 .UNSPECIFIED.,.F.,.F.,(4,4),(0.960106131022676,1.8485476634033),
 .UNSPECIFIED.);
#551=B_SPLINE_CURVE_WITH_KNOTS('',3,(#59566,#59567,#59568,#59569),
 .UNSPECIFIED.,.F.,.F.,(4,4),(1.0115487697186,1.89999030209922),
 .UNSPECIFIED.);
#552=B_SPLINE_CURVE_WITH_KNOTS('',3,(#59574,#59575,#59576,#59577,#59578,
#59579,#59580,#59581,#59582,#59583,#59584,#59585,#59586,#59587,#59588,#59589,
#59590,#59591,#59592,#59593,#59594,#59595,#59596,#59597,#59598,#59599,#59600),
 .UNSPECIFIED.,.F.,.F.,(4,3,2,2,2,2,2,2,2,2,2,2,4),(0.232932117987128,0.233989323147793,
0.236545962444563,0.240335281908429,0.24774494964748,0.261894911831244,
0.277641329370738,0.294641376545414,0.30975555389686,0.323519464298527,
0.33017367490881,0.3343328141555,0.336361587071577),.UNSPECIFIED.);
#553=B_SPLINE_CURVE_WITH_KNOTS('',3,(#59606,#59607,#59608,#59609,#59610,
#59611,#59612,#59613,#59614,#59615,#59616,#59617,#59618,#59619,#59620,#59621,
#59622,#59623,#59624,#59625,#59626,#59627,#59628,#59629,#59630,#59631,#59632,
#59633,#59634,#59635,#59636,#59637),.UNSPECIFIED.,.F.,.F.,(4,2,2,2,2,2,
2,2,2,2,2,2,2,2,2,4),(0.000552255618197645,0.00250735066884162,0.00544388472231144,
0.0102014204810308,0.0220775236397517,0.044197607004219,0.0559969069004104,
0.0645228059047183,0.0728085457984712,0.0835882270757895,0.102795442173472,
0.125000410426586,0.136058920564129,0.140727854886482,0.142845622304253,
0.144031712762546),.UNSPECIFIED.);
#554=B_SPLINE_CURVE_WITH_KNOTS('',3,(#59646,#59647,#59648,#59649),
 .UNSPECIFIED.,.F.,.F.,(4,4),(0.992149273556617,1.8805029517096),
 .UNSPECIFIED.);
#555=B_SPLINE_CURVE_WITH_KNOTS('',3,(#59654,#59655,#59656,#59657),
 .UNSPECIFIED.,.F.,.F.,(4,4),(1.01721488555274,1.90556856370572),
 .UNSPECIFIED.);
#556=B_SPLINE_CURVE_WITH_KNOTS('',3,(#59662,#59663,#59664,#59665,#59666,
#59667,#59668,#59669,#59670,#59671,#59672,#59673,#59674,#59675,#59676,#59677,
#59678,#59679,#59680,#59681,#59682,#59683,#59684,#59685,#59686,#59687,#59688,
#59689,#59690),.UNSPECIFIED.,.F.,.F.,(4,3,2,2,2,2,2,2,2,2,2,2,2,4),(0.244877808034099,
0.245941379435807,0.248507773430932,0.252352570084648,0.260140357196049,
0.274281958048573,0.28577716640828,0.296461087012187,0.30760639953159,0.320385682648555,
0.337686825296551,0.34471511735484,0.349023201353445,0.350883558011521),
 .UNSPECIFIED.);
#557=B_SPLINE_CURVE_WITH_KNOTS('',3,(#59696,#59697,#59698,#59699,#59700,
#59701,#59702,#59703,#59704,#59705,#59706,#59707,#59708,#59709,#59710,#59711,
#59712,#59713,#59714,#59715,#59716,#59717,#59718,#59719,#59720,#59721,#59722,
#59723,#59724,#59725,#59726,#59727),.UNSPECIFIED.,.F.,.F.,(4,2,2,2,2,2,
2,2,2,2,2,2,2,2,2,4),(0.000552255618249655,0.00250735067656752,0.00544388475827691,
0.0102014205628046,0.0220775238360495,0.0441976074134883,0.055996907423309,
0.0645228065097832,0.0728085464834914,0.0835882278647535,0.102795443147687,
0.125000411614945,0.136058921858814,0.140727856226151,0.142845623664258,
0.144031714104742),.UNSPECIFIED.);
#558=B_SPLINE_CURVE_WITH_KNOTS('',3,(#59736,#59737,#59738,#59739),
 .UNSPECIFIED.,.F.,.F.,(4,4),(1.02924883146194,1.91752828913416),
 .UNSPECIFIED.);
#559=B_SPLINE_CURVE_WITH_KNOTS('',3,(#59744,#59745,#59746,#59747),
 .UNSPECIFIED.,.F.,.F.,(4,4),(1.020135190352,1.90841464802423),
 .UNSPECIFIED.);
#560=B_SPLINE_CURVE_WITH_KNOTS('',3,(#59752,#59753,#59754,#59755,#59756,
#59757,#59758,#59759,#59760,#59761,#59762,#59763,#59764,#59765,#59766,#59767,
#59768,#59769,#59770,#59771,#59772,#59773,#59774,#59775,#59776,#59777,#59778,
#59779,#59780,#59781,#59782,#59783,#59784),.UNSPECIFIED.,.F.,.F.,(4,3,2,
2,2,2,2,2,2,2,2,2,2,2,2,4),(0.196959320042169,0.198017145081817,0.200540880250775,
0.204205249052827,0.212045863738905,0.231522357849409,0.239816668286406,
0.245036313826137,0.249558567688347,0.254824767272002,0.263328140162152,
0.280727522155542,0.287167297193858,0.290158226133316,0.29220413474297,
0.292205277794279),.UNSPECIFIED.);
#561=B_SPLINE_CURVE_WITH_KNOTS('',3,(#59790,#59791,#59792,#59793,#59794,
#59795,#59796,#59797,#59798,#59799,#59800,#59801,#59802,#59803,#59804,#59805,
#59806,#59807,#59808,#59809,#59810,#59811,#59812,#59813,#59814,#59815,#59816,
#59817,#59818,#59819,#59820,#59821),.UNSPECIFIED.,.F.,.F.,(4,2,2,2,2,2,
2,2,2,2,2,2,2,2,2,4),(0.000552255618140626,0.00250735066035772,0.0054438846828297,
0.0102014203913245,0.022077523424572,0.0441976065561941,0.055996906328127,
0.0645228052426097,0.0728085450491545,0.0835882262128905,0.102795441108078,
0.12500040912679,0.136058919148013,0.14072785342133,0.142845620816795,0.144031711312269),
 .UNSPECIFIED.);
#562=B_SPLINE_CURVE_WITH_KNOTS('',3,(#59830,#59831,#59832,#59833),
 .UNSPECIFIED.,.F.,.F.,(4,4),(1.01302199639782,1.90133038588089),
 .UNSPECIFIED.);
#563=B_SPLINE_CURVE_WITH_KNOTS('',3,(#59838,#59839,#59840,#59841),
 .UNSPECIFIED.,.F.,.F.,(4,4),(1.01910936201615,1.90741775149922),
 .UNSPECIFIED.);
#564=B_SPLINE_CURVE_WITH_KNOTS('',3,(#59846,#59847,#59848,#59849,#59850,
#59851,#59852,#59853,#59854,#59855,#59856,#59857,#59858,#59859,#59860,#59861,
#59862,#59863,#59864,#59865,#59866,#59867,#59868,#59869,#59870,#59871,#59872,
#59873,#59874,#59875,#59876,#59877,#59878),.UNSPECIFIED.,.F.,.F.,(4,3,2,
2,2,2,2,2,2,2,2,2,2,2,2,4),(0.19695932004261,0.198017145082242,0.200540880251192,
0.204205249053208,0.212045863739241,0.23152235784927,0.239816668286048,
0.24503631382569,0.24955856768786,0.254824767271468,0.263328140161551,0.280727522154842,
0.287167297192917,0.290158226132224,0.292204134741798,0.292205277793109),
 .UNSPECIFIED.);
#565=B_SPLINE_CURVE_WITH_KNOTS('',3,(#59884,#59885,#59886,#59887,#59888,
#59889,#59890,#59891,#59892,#59893,#59894,#59895,#59896,#59897,#59898,#59899,
#59900,#59901,#59902,#59903,#59904,#59905,#59906,#59907,#59908,#59909,#59910,
#59911),.UNSPECIFIED.,.F.,.F.,(4,2,2,2,2,2,2,2,2,2,2,2,2,4),(0.000552255324019496,
0.00250712858729281,0.00542730282780847,0.0100896996439777,0.0208199651240228,
0.0391433219483803,0.056641382902855,0.0737548152573535,0.0916180264797638,
0.113112720573213,0.124811938447872,0.129415130046053,0.13146681109567,
0.132736827221508),.UNSPECIFIED.);
#566=B_SPLINE_CURVE_WITH_KNOTS('',3,(#59920,#59921,#59922,#59923),
 .UNSPECIFIED.,.F.,.F.,(4,4),(0.973845213090798,1.86224631803132),
 .UNSPECIFIED.);
#567=B_SPLINE_CURVE_WITH_KNOTS('',3,(#59928,#59929,#59930,#59931),
 .UNSPECIFIED.,.F.,.F.,(4,4),(1.01459402224647,1.90299512718699),
 .UNSPECIFIED.);
#568=B_SPLINE_CURVE_WITH_KNOTS('',3,(#59936,#59937,#59938,#59939,#59940,
#59941,#59942,#59943,#59944,#59945,#59946,#59947,#59948,#59949,#59950,#59951,
#59952,#59953,#59954,#59955,#59956,#59957,#59958,#59959,#59960,#59961,#59962,
#59963,#59964),.UNSPECIFIED.,.F.,.F.,(4,3,2,2,2,2,2,2,2,2,2,2,2,4),(0.220457494407383,
0.221514163341664,0.224063974274128,0.227827813743661,0.235231812669406,
0.248804927500478,0.261986328474954,0.275641459327076,0.289130041136135,
0.303381192080165,0.310291199881849,0.313709542892314,0.316059908326691,
0.316319431219465),.UNSPECIFIED.);
#569=B_SPLINE_CURVE_WITH_KNOTS('',3,(#59970,#59971,#59972,#59973,#59974,
#59975,#59976,#59977,#59978,#59979,#59980,#59981,#59982,#59983,#59984,#59985,
#59986,#59987,#59988,#59989,#59990,#59991,#59992,#59993,#59994,#59995,#59996,
#59997),.UNSPECIFIED.,.F.,.F.,(4,2,2,2,2,2,2,2,2,2,2,2,2,4),(0.000552255452470749,
0.0025072256249705,0.00543435583319841,0.0101358464467806,0.0212263040739443,
0.0396611683296533,0.0549611363112922,0.069003832575456,0.0841023639971007,
0.102253717468459,0.114574292768908,0.118850100165663,0.120613949875907,
0.121845701929046),.UNSPECIFIED.);
#570=B_SPLINE_CURVE_WITH_KNOTS('',3,(#60006,#60007,#60008,#60009),
 .UNSPECIFIED.,.F.,.F.,(4,4),(0.952234974413515,1.84070284457626),
 .UNSPECIFIED.);
#571=B_SPLINE_CURVE_WITH_KNOTS('',3,(#60014,#60015,#60016,#60017),
 .UNSPECIFIED.,.F.,.F.,(4,4),(1.00739097317572,1.89585884333848),
 .UNSPECIFIED.);
#572=B_SPLINE_CURVE_WITH_KNOTS('',3,(#60022,#60023,#60024,#60025,#60026,
#60027,#60028,#60029,#60030,#60031,#60032,#60033,#60034,#60035,#60036,#60037,
#60038,#60039,#60040,#60041,#60042,#60043,#60044,#60045,#60046,#60047,#60048,
#60049,#60050,#60051,#60052),.UNSPECIFIED.,.F.,.F.,(4,3,2,2,2,2,2,2,2,2,
2,2,2,2,4),(0.214188423795365,0.215245209140312,0.217829605860112,0.22176041529285,
0.229921784196946,0.245839020971122,0.256431324643212,0.265077654350895,
0.273928386150392,0.28499361706498,0.300677807868051,0.308332988419563,
0.31362526833756,0.316793712715947,0.31837341606385),.UNSPECIFIED.);
#573=B_SPLINE_CURVE_WITH_KNOTS('',3,(#60147,#60148,#60149,#60150,#60151,
#60152,#60153,#60154,#60155,#60156,#60157,#60158,#60159,#60160,#60161,#60162,
#60163,#60164,#60165,#60166,#60167,#60168,#60169,#60170,#60171,#60172,#60173,
#60174),.UNSPECIFIED.,.F.,.F.,(4,2,2,2,2,2,2,2,2,2,2,2,2,4),(0.000544534331770364,
0.00261482458396479,0.00566461977284545,0.0105091354087174,0.0191944349126956,
0.0290670716136037,0.0385711899201246,0.0479537104295029,0.0577071251500524,
0.0693239212081265,0.0751757960734721,0.0775973292620321,0.0787013199411384,
0.0793612603968366),.UNSPECIFIED.);
#574=B_SPLINE_CURVE_WITH_KNOTS('',3,(#60183,#60184,#60185,#60186),
 .UNSPECIFIED.,.F.,.F.,(4,4),(0.972622216146951,1.74476629192075),
 .UNSPECIFIED.);
#575=B_SPLINE_CURVE_WITH_KNOTS('',3,(#60191,#60192,#60193,#60194),
 .UNSPECIFIED.,.F.,.F.,(4,4),(1.00913865884316,1.78128273461697),
 .UNSPECIFIED.);
#576=B_SPLINE_CURVE_WITH_KNOTS('',3,(#60199,#60200,#60201,#60202,#60203,
#60204,#60205,#60206,#60207,#60208,#60209,#60210,#60211,#60212,#60213,#60214,
#60215,#60216,#60217,#60218,#60219,#60220,#60221,#60222,#60223,#60224,#60225),
 .UNSPECIFIED.,.F.,.F.,(4,3,2,2,2,2,2,2,2,2,2,2,4),(0.227117616561984,0.228178838531469,
0.230853194575438,0.234806311591967,0.242541867555993,0.256464561825903,
0.270271019853529,0.284767676904166,0.299196973939493,0.314541585771187,
0.323020081002097,0.328061711878854,0.331723678699563),.UNSPECIFIED.);
#577=B_SPLINE_CURVE_WITH_KNOTS('',3,(#60231,#60232,#60233,#60234,#60235,
#60236,#60237,#60238,#60239,#60240,#60241,#60242,#60243,#60244,#60245,#60246,
#60247,#60248,#60249,#60250,#60251,#60252,#60253,#60254,#60255,#60256,#60257,
#60258,#60259,#60260),.UNSPECIFIED.,.F.,.F.,(4,2,2,2,2,2,2,2,2,2,2,2,2,
2,4),(0.00054453482582504,0.00261525007563638,0.00568461731727823,0.0106418232707552,
0.0201008492843188,0.0304143383071815,0.0361114848938895,0.0403561756098437,
0.044582919067582,0.050204579699446,0.0603086215837312,0.0719443708674587,
0.0783632089262617,0.0816596245840498,0.0839489891389517),.UNSPECIFIED.);
#578=B_SPLINE_CURVE_WITH_KNOTS('',3,(#60269,#60270,#60271,#60272),
 .UNSPECIFIED.,.F.,.F.,(4,4),(1.01074747522778,1.7828236876201),
 .UNSPECIFIED.);
#579=B_SPLINE_CURVE_WITH_KNOTS('',3,(#60277,#60278,#60279,#60280),
 .UNSPECIFIED.,.F.,.F.,(4,4),(1.01328568624373,1.78536189863605),
 .UNSPECIFIED.);
#580=B_SPLINE_CURVE_WITH_KNOTS('',3,(#60285,#60286,#60287,#60288,#60289,
#60290,#60291,#60292,#60293,#60294,#60295,#60296,#60297,#60298,#60299,#60300,
#60301,#60302,#60303,#60304,#60305,#60306,#60307,#60308,#60309,#60310,#60311,
#60312,#60313,#60314,#60315),.UNSPECIFIED.,.F.,.F.,(4,3,2,2,2,2,2,2,2,2,
2,2,2,2,4),(0.214163227121214,0.21522148611425,0.217879469870484,0.221777671209004,
0.230219855510565,0.250403074215797,0.259557360898345,0.265568826006539,
0.270963492852842,0.2774499439387,0.288207765299504,0.310806527050195,0.318607986189108,
0.322642260344804,0.324958092305149),.UNSPECIFIED.);
#581=B_SPLINE_CURVE_WITH_KNOTS('',3,(#60321,#60322,#60323,#60324,#60325,
#60326,#60327,#60328,#60329,#60330,#60331,#60332,#60333,#60334,#60335,#60336,
#60337,#60338,#60339,#60340,#60341,#60342,#60343,#60344,#60345,#60346,#60347,
#60348,#60349,#60350),.UNSPECIFIED.,.F.,.F.,(4,2,2,2,2,2,2,2,2,2,2,2,2,
2,4),(0.000544534825876113,0.00261525008513596,0.00568461736158124,0.0106418233713403,
0.0201008494923424,0.030414338631891,0.0361114852830982,0.0403561760471232,
0.0445829195527737,0.0502045802484256,0.0603086222473851,0.0719443716631595,
0.0783632097946434,0.0816596254898528,0.0839489900425068),.UNSPECIFIED.);
#582=B_SPLINE_CURVE_WITH_KNOTS('',3,(#60359,#60360,#60361,#60362),
 .UNSPECIFIED.,.F.,.F.,(4,4),(1.01074747522778,1.7828236876201),
 .UNSPECIFIED.);
#583=B_SPLINE_CURVE_WITH_KNOTS('',3,(#60367,#60368,#60369,#60370),
 .UNSPECIFIED.,.F.,.F.,(4,4),(1.01328568624373,1.78536189863605),
 .UNSPECIFIED.);
#584=B_SPLINE_CURVE_WITH_KNOTS('',3,(#60375,#60376,#60377,#60378,#60379,
#60380,#60381,#60382,#60383,#60384,#60385,#60386,#60387,#60388,#60389,#60390,
#60391,#60392,#60393,#60394,#60395,#60396,#60397,#60398,#60399,#60400,#60401,
#60402,#60403,#60404,#60405),.UNSPECIFIED.,.F.,.F.,(4,3,2,2,2,2,2,2,2,2,
2,2,2,2,4),(0.214163227114599,0.21522148610762,0.217879469863857,0.221777671202393,
0.230219855504022,0.250403074209431,0.259557360892022,0.265568826000264,
0.270963492846616,0.277449943932527,0.288207765293429,0.310806527044066,
0.318607986182513,0.322642260337867,0.324958092298005),.UNSPECIFIED.);
#585=B_SPLINE_CURVE_WITH_KNOTS('',3,(#60411,#60412,#60413,#60414,#60415,
#60416,#60417,#60418,#60419,#60420,#60421,#60422,#60423,#60424,#60425,#60426,
#60427,#60428,#60429,#60430,#60431,#60432,#60433,#60434,#60435,#60436,#60437,
#60438),.UNSPECIFIED.,.F.,.F.,(4,2,2,2,2,2,2,2,2,2,2,2,2,4),(0.000544534331649385,
0.00261482456155126,0.00566461966862882,0.0105091351745479,0.0191944344450001,
0.0290670708802926,0.0385711889311368,0.0479537091880883,0.0577071236462347,
0.0693239193914192,0.075175794100405,0.0775973272235677,0.078701317872934,
0.0793612583498743),.UNSPECIFIED.);
#586=B_SPLINE_CURVE_WITH_KNOTS('',3,(#60447,#60448,#60449,#60450),
 .UNSPECIFIED.,.F.,.F.,(4,4),(0.972622216146952,1.74476629192075),
 .UNSPECIFIED.);
#587=B_SPLINE_CURVE_WITH_KNOTS('',3,(#60455,#60456,#60457,#60458),
 .UNSPECIFIED.,.F.,.F.,(4,4),(1.00913865884317,1.78128273461697),
 .UNSPECIFIED.);
#588=B_SPLINE_CURVE_WITH_KNOTS('',3,(#60463,#60464,#60465,#60466,#60467,
#60468,#60469,#60470,#60471,#60472,#60473,#60474,#60475,#60476,#60477,#60478,
#60479,#60480,#60481,#60482,#60483,#60484,#60485,#60486,#60487,#60488,#60489),
 .UNSPECIFIED.,.F.,.F.,(4,3,2,2,2,2,2,2,2,2,2,2,4),(0.227117616565019,0.228178838534504,
0.230853194578471,0.234806311594996,0.242541867559022,0.256464561829114,
0.270271019857134,0.284767676908152,0.299196973943848,0.314541585775807,
0.323020081006769,0.328061711883539,0.331723678704291),.UNSPECIFIED.);
#589=B_SPLINE_CURVE_WITH_KNOTS('',3,(#60495,#60496,#60497,#60498,#60499,
#60500,#60501,#60502,#60503,#60504,#60505,#60506,#60507,#60508,#60509,#60510,
#60511,#60512,#60513,#60514,#60515,#60516,#60517,#60518,#60519,#60520,#60521,
#60522),.UNSPECIFIED.,.F.,.F.,(4,2,2,2,2,2,2,2,2,2,2,2,2,4),(0.000544534549921907,
0.00261501248850167,0.00567325101762964,0.0105645437460391,0.0195297150491738,
0.0291097118185737,0.0371551154138167,0.0446716615983505,0.0528464746815875,
0.0626030531723468,0.0695733104345648,0.0738617500897138,0.0760814802251334,
0.0776419689378844),.UNSPECIFIED.);
#590=B_SPLINE_CURVE_WITH_KNOTS('',3,(#60531,#60532,#60533,#60534),
 .UNSPECIFIED.,.F.,.F.,(4,4),(0.950799700125448,1.72299586285748),
 .UNSPECIFIED.);
#591=B_SPLINE_CURVE_WITH_KNOTS('',3,(#60539,#60540,#60541,#60542),
 .UNSPECIFIED.,.F.,.F.,(4,4),(1.00192780386193,1.77412396659396),
 .UNSPECIFIED.);
#592=B_SPLINE_CURVE_WITH_KNOTS('',3,(#60547,#60548,#60549,#60550,#60551,
#60552,#60553,#60554,#60555,#60556,#60557,#60558,#60559,#60560,#60561,#60562,
#60563,#60564,#60565,#60566,#60567,#60568,#60569,#60570,#60571,#60572,#60573,
#60574,#60575,#60576,#60577),.UNSPECIFIED.,.F.,.F.,(4,3,2,2,2,2,2,2,2,2,
2,2,2,2,4),(0.18213885585433,0.183202254112354,0.185821008015182,0.189544523355733,
0.197294447985539,0.212715272503728,0.222658444672328,0.230577174767301,
0.238278170345223,0.247433567012496,0.261550284890387,0.268370460413016,
0.271469240197429,0.273499326101355,0.273748394098311),.UNSPECIFIED.);
#593=B_SPLINE_CURVE_WITH_KNOTS('',3,(#60583,#60584,#60585,#60586,#60587,
#60588,#60589,#60590,#60591,#60592,#60593,#60594,#60595,#60596,#60597,#60598,
#60599,#60600,#60601,#60602,#60603,#60604,#60605,#60606,#60607,#60608,#60609,
#60610),.UNSPECIFIED.,.F.,.F.,(4,2,2,2,2,2,2,2,2,2,2,2,2,4),(0.000544534331647821,
0.00261482456124733,0.00566461966720797,0.010509135171325,0.0191944344388363,
0.0290670708710745,0.0385711889189857,0.0479537091730275,0.0577071236281329,
0.0693239193698956,0.0751757940772305,0.0775973271996817,0.0787013178487444,
0.0793612583258265),.UNSPECIFIED.);
#594=B_SPLINE_CURVE_WITH_KNOTS('',3,(#60619,#60620,#60621,#60622),
 .UNSPECIFIED.,.F.,.F.,(4,4),(0.972622216146952,1.74476629192075),
 .UNSPECIFIED.);
#595=B_SPLINE_CURVE_WITH_KNOTS('',3,(#60627,#60628,#60629,#60630),
 .UNSPECIFIED.,.F.,.F.,(4,4),(1.00913865884317,1.78128273461697),
 .UNSPECIFIED.);
#596=B_SPLINE_CURVE_WITH_KNOTS('',3,(#60635,#60636,#60637,#60638,#60639,
#60640,#60641,#60642,#60643,#60644,#60645,#60646,#60647,#60648,#60649,#60650,
#60651,#60652,#60653,#60654,#60655,#60656,#60657,#60658,#60659,#60660,#60661),
 .UNSPECIFIED.,.F.,.F.,(4,3,2,2,2,2,2,2,2,2,2,2,4),(0.227117616562292,0.228178838531774,
0.230853194575744,0.234806311592284,0.242541867556376,0.256464561826322,
0.27027101985389,0.284767676904497,0.299196973939812,0.314541585771443,
0.323020081002267,0.328061711879021,0.331723678699715),.UNSPECIFIED.);
#597=B_SPLINE_CURVE_WITH_KNOTS('',3,(#60667,#60668,#60669,#60670,#60671,
#60672,#60673,#60674,#60675,#60676,#60677,#60678,#60679,#60680,#60681,#60682,
#60683,#60684,#60685,#60686,#60687,#60688,#60689,#60690,#60691,#60692,#60693,
#60694,#60695,#60696),.UNSPECIFIED.,.F.,.F.,(4,2,2,2,2,2,2,2,2,2,2,2,2,
2,4),(0.000544534825850911,0.00261525008045177,0.00568461733973985,0.0106418233217765,
0.0201008493894312,0.0304143384705787,0.0361114850895091,0.0403561758295001,
0.0445829193111929,0.0502045799749338,0.0603086219165353,0.0719443712661402,
0.0783632093611635,0.0816596250376284,0.0839489895887599),.UNSPECIFIED.);
#598=B_SPLINE_CURVE_WITH_KNOTS('',3,(#60705,#60706,#60707,#60708),
 .UNSPECIFIED.,.F.,.F.,(4,4),(1.01074747522778,1.7828236876201),
 .UNSPECIFIED.);
#599=B_SPLINE_CURVE_WITH_KNOTS('',3,(#60713,#60714,#60715,#60716),
 .UNSPECIFIED.,.F.,.F.,(4,4),(1.01328568624374,1.78536189863605),
 .UNSPECIFIED.);
#600=B_SPLINE_CURVE_WITH_KNOTS('',3,(#60721,#60722,#60723,#60724,#60725,
#60726,#60727,#60728,#60729,#60730,#60731,#60732,#60733,#60734,#60735,#60736,
#60737,#60738,#60739,#60740,#60741,#60742,#60743,#60744,#60745,#60746,#60747,
#60748,#60749,#60750,#60751),.UNSPECIFIED.,.F.,.F.,(4,3,2,2,2,2,2,2,2,2,
2,2,2,2,4),(0.214163227115852,0.215221486108889,0.217879469865123,0.221777671203643,
0.230219855505183,0.250403074210647,0.25955736089342,0.265568826001748,
0.270963492848269,0.277449943934345,0.288207765295491,0.310806527046658,
0.318607986185197,0.322642260340538,0.324958092300691),.UNSPECIFIED.);
#601=B_SPLINE_CURVE_WITH_KNOTS('',3,(#60757,#60758,#60759,#60760,#60761,
#60762,#60763,#60764,#60765,#60766,#60767,#60768,#60769,#60770,#60771,#60772,
#60773,#60774,#60775,#60776,#60777,#60778,#60779,#60780,#60781,#60782,#60783,
#60784,#60785,#60786),.UNSPECIFIED.,.F.,.F.,(4,2,2,2,2,2,2,2,2,2,2,2,2,
2,4),(0.000544534825862876,0.00261525008268697,0.00568461735014547,0.0106418233453183,
0.0201008494382171,0.0304143385469081,0.0361114851810566,0.040356175932351,
0.0445829194252694,0.0502045801039656,0.0603086220724571,0.0719443714532619,
0.0783632095663442,0.0816596252524092,0.0839489898001846),.UNSPECIFIED.);
#602=B_SPLINE_CURVE_WITH_KNOTS('',3,(#60795,#60796,#60797,#60798),
 .UNSPECIFIED.,.F.,.F.,(4,4),(1.01074747522778,1.7828236876201),
 .UNSPECIFIED.);
#603=B_SPLINE_CURVE_WITH_KNOTS('',3,(#60803,#60804,#60805,#60806),
 .UNSPECIFIED.,.F.,.F.,(4,4),(1.01328568624373,1.78536189863605),
 .UNSPECIFIED.);
#604=B_SPLINE_CURVE_WITH_KNOTS('',3,(#60811,#60812,#60813,#60814,#60815,
#60816,#60817,#60818,#60819,#60820,#60821,#60822,#60823,#60824,#60825,#60826,
#60827,#60828,#60829,#60830,#60831,#60832,#60833,#60834,#60835,#60836,#60837,
#60838,#60839,#60840,#60841),.UNSPECIFIED.,.F.,.F.,(4,3,2,2,2,2,2,2,2,2,
2,2,2,2,4),(0.214163227114928,0.21522148610796,0.217879469864186,0.221777671202672,
0.230219855504225,0.25040307420936,0.259557360891831,0.265568825999994,
0.270963492846248,0.27744994393201,0.288207765292651,0.310806527042822,
0.318607986181364,0.322642260336865,0.3249580922971),.UNSPECIFIED.);
#605=B_SPLINE_CURVE_WITH_KNOTS('',3,(#60847,#60848,#60849,#60850,#60851,
#60852,#60853,#60854,#60855,#60856,#60857,#60858,#60859,#60860,#60861,#60862,
#60863,#60864,#60865,#60866,#60867,#60868,#60869,#60870,#60871,#60872,#60873,
#60874),.UNSPECIFIED.,.F.,.F.,(4,2,2,2,2,2,2,2,2,2,2,2,2,4),(0.000544534331706975,
0.00261482457222462,0.00566461971825641,0.0105091352860569,0.0191944346676074,
0.0290670712291455,0.0385711894015179,0.0479537097784548,0.057707124361322,
0.0693239202552609,0.0751757950384062,0.077597328192707,0.07870131885622,
0.0793612593163129),.UNSPECIFIED.);
#606=B_SPLINE_CURVE_WITH_KNOTS('',3,(#60883,#60884,#60885,#60886),
 .UNSPECIFIED.,.F.,.F.,(4,4),(0.972622216146952,1.74476629192075),
 .UNSPECIFIED.);
#607=B_SPLINE_CURVE_WITH_KNOTS('',3,(#60891,#60892,#60893,#60894),
 .UNSPECIFIED.,.F.,.F.,(4,4),(1.00913865884317,1.78128273461697),
 .UNSPECIFIED.);
#608=B_SPLINE_CURVE_WITH_KNOTS('',3,(#60899,#60900,#60901,#60902,#60903,
#60904,#60905,#60906,#60907,#60908,#60909,#60910,#60911,#60912,#60913,#60914,
#60915,#60916,#60917,#60918,#60919,#60920,#60921,#60922,#60923,#60924,#60925),
 .UNSPECIFIED.,.F.,.F.,(4,3,2,2,2,2,2,2,2,2,2,2,4),(0.227117616560756,0.228178838530236,
0.230853194574207,0.234806311590749,0.242541867554764,0.256464561824811,
0.270271019852753,0.284767676903674,0.299196973939247,0.314541585771045,
0.3230200810019,0.328061711878609,0.331723678699319),.UNSPECIFIED.);
#609=B_SPLINE_CURVE_WITH_KNOTS('',3,(#60931,#60932,#60933,#60934,#60935,
#60936,#60937,#60938,#60939,#60940,#60941,#60942,#60943,#60944,#60945,#60946),
 .UNSPECIFIED.,.F.,.F.,(4,2,2,2,2,2,2,4),(0.000544534550093875,0.00261501252043313,
0.00567325116628869,0.0105645440814823,0.0195297157273874,0.02910971286263,
0.037155116765118,0.0404959091580222),.UNSPECIFIED.);
#610=B_SPLINE_CURVE_WITH_KNOTS('',3,(#60954,#60955,#60956,#60957,#60958,
#60959,#60960,#60961,#60962,#60963,#60964,#60965,#60966,#60967,#60968,#60969),
 .UNSPECIFIED.,.F.,.F.,(4,2,2,2,2,2,2,4),(0.0404959091580222,0.0446716632368038,
0.0528464766324242,0.062603055496004,0.0695733130238269,0.0738617528426058,
0.0760814830627305,0.0776419717712023),.UNSPECIFIED.);
#611=B_SPLINE_CURVE_WITH_KNOTS('',3,(#60972,#60973,#60974,#60975),
 .UNSPECIFIED.,.F.,.F.,(4,4),(0.950799700125448,1.72299586285748),
 .UNSPECIFIED.);
#612=B_SPLINE_CURVE_WITH_KNOTS('',3,(#60980,#60981,#60982,#60983),
 .UNSPECIFIED.,.F.,.F.,(4,4),(1.00192780386193,1.77412396659396),
 .UNSPECIFIED.);
#613=B_SPLINE_CURVE_WITH_KNOTS('',3,(#60989,#60990,#60991,#60992,#60993,
#60994,#60995,#60996,#60997,#60998,#60999,#61000,#61001,#61002,#61003,#61004),
 .UNSPECIFIED.,.F.,.F.,(4,2,2,2,2,2,2,4),(0.23072740937187,0.238278170343491,
0.247433567010806,0.261550284888684,0.268370460411144,0.271469240195438,
0.273499326099292,0.27374839409624),.UNSPECIFIED.);
#614=B_SPLINE_CURVE_WITH_KNOTS('',3,(#61005,#61006,#61007,#61008,#61009,
#61010,#61011,#61012,#61013,#61014,#61015,#61016,#61017,#61018,#61019,#61020,
#61021,#61022,#61023),.UNSPECIFIED.,.F.,.F.,(4,3,2,2,2,2,2,2,4),(0.182138855852465,
0.183202254110488,0.185821008013318,0.189544523353877,0.197294447983706,
0.212715272501937,0.222658444670555,0.230577174765548,0.23072740937187),
 .UNSPECIFIED.);
#615=B_SPLINE_CURVE_WITH_KNOTS('',3,(#61029,#61030,#61031,#61032,#61033,
#61034,#61035,#61036,#61037,#61038,#61039,#61040,#61041,#61042,#61043,#61044,
#61045,#61046,#61047,#61048,#61049,#61050,#61051,#61052,#61053,#61054,#61055,
#61056),.UNSPECIFIED.,.F.,.F.,(4,2,2,2,2,2,2,2,2,2,2,2,2,4),(0.000544534331659907,
0.00261482456349501,0.00566461967766457,0.0105091351948414,0.0191944344856125,
0.0290670709441028,0.0385711890172752,0.0479537092962682,0.0577071237773125,
0.0693239195500253,0.0751757942726928,0.0775973274016732,0.0787013180536914,
0.0793612585221559),.UNSPECIFIED.);
#616=B_SPLINE_CURVE_WITH_KNOTS('',3,(#61065,#61066,#61067,#61068),
 .UNSPECIFIED.,.F.,.F.,(4,4),(0.972622216146952,1.74476629192075),
 .UNSPECIFIED.);
#617=B_SPLINE_CURVE_WITH_KNOTS('',3,(#61073,#61074,#61075,#61076),
 .UNSPECIFIED.,.F.,.F.,(4,4),(1.00913865884317,1.78128273461697),
 .UNSPECIFIED.);
#618=B_SPLINE_CURVE_WITH_KNOTS('',3,(#61081,#61082,#61083,#61084,#61085,
#61086,#61087,#61088,#61089,#61090,#61091,#61092,#61093,#61094,#61095,#61096,
#61097,#61098,#61099,#61100,#61101,#61102,#61103,#61104,#61105,#61106,#61107),
 .UNSPECIFIED.,.F.,.F.,(4,3,2,2,2,2,2,2,2,2,2,2,4),(0.227117616559912,0.228178838529394,
0.230853194573358,0.234806311589871,0.242541867553882,0.256464561823589,
0.270271019850829,0.284767676901017,0.299196973935865,0.314541585767127,
0.323020080997816,0.32806171187444,0.331723678695039),.UNSPECIFIED.);
#619=B_SPLINE_CURVE_WITH_KNOTS('',3,(#61113,#61114,#61115,#61116,#61117,
#61118,#61119,#61120,#61121,#61122,#61123,#61124,#61125,#61126,#61127,#61128,
#61129,#61130,#61131,#61132,#61133,#61134,#61135,#61136,#61137,#61138,#61139,
#61140,#61141,#61142),.UNSPECIFIED.,.F.,.F.,(4,2,2,2,2,2,2,2,2,2,2,2,2,
2,4),(0.000544534825927728,0.0026152500947561,0.00568461740644579,0.0106418234731972,
0.0201008497031229,0.0304143389610872,0.036111485677717,0.0403561764905055,
0.0445829200447778,0.0502045808051401,0.0603086229204531,0.0719443724704426,
0.0783632106754923,0.0816596264082429,0.0839489909616778),.UNSPECIFIED.);
#620=B_SPLINE_CURVE_WITH_KNOTS('',3,(#61151,#61152,#61153,#61154),
 .UNSPECIFIED.,.F.,.F.,(4,4),(1.01074747522778,1.7828236876201),
 .UNSPECIFIED.);
#621=B_SPLINE_CURVE_WITH_KNOTS('',3,(#61159,#61160,#61161,#61162),
 .UNSPECIFIED.,.F.,.F.,(4,4),(1.01328568624373,1.78536189863605),
 .UNSPECIFIED.);
#622=B_SPLINE_CURVE_WITH_KNOTS('',3,(#61167,#61168,#61169,#61170,#61171,
#61172,#61173,#61174,#61175,#61176,#61177,#61178,#61179,#61180,#61181,#61182,
#61183,#61184,#61185,#61186,#61187,#61188,#61189,#61190,#61191,#61192,#61193,
#61194,#61195,#61196,#61197),.UNSPECIFIED.,.F.,.F.,(4,3,2,2,2,2,2,2,2,2,
2,2,2,2,4),(0.214163227107514,0.215221486100543,0.217879469856777,0.221777671195291,
0.230219855496679,0.250403074200591,0.259557360882527,0.265568825990305,
0.270963492836326,0.277449943921837,0.288207765282045,0.310806527031384,
0.318607986169581,0.322642260324875,0.324958092284982),.UNSPECIFIED.);
#623=B_SPLINE_CURVE_WITH_KNOTS('',3,(#61203,#61204,#61205,#61206,#61207,
#61208,#61209,#61210,#61211,#61212,#61213,#61214,#61215,#61216,#61217,#61218,
#61219,#61220,#61221,#61222,#61223,#61224,#61225,#61226,#61227,#61228,#61229,
#61230,#61231,#61232),.UNSPECIFIED.,.F.,.F.,(4,2,2,2,2,2,2,2,2,2,2,2,2,
2,4),(0.000544534825852039,0.00261525008066538,0.00568461734072438,0.0106418233239587,
0.0201008493939144,0.0304143384775563,0.0361114850978667,0.0403561758388711,
0.0445829193215816,0.0502045799867152,0.0603086219308081,0.071944371283317,
0.0783632093794051,0.0816596250561908,0.0839489896124222),.UNSPECIFIED.);
#624=B_SPLINE_CURVE_WITH_KNOTS('',3,(#61241,#61242,#61243,#61244),
 .UNSPECIFIED.,.F.,.F.,(4,4),(1.01074747522778,1.7828236876201),
 .UNSPECIFIED.);
#625=B_SPLINE_CURVE_WITH_KNOTS('',3,(#61249,#61250,#61251,#61252),
 .UNSPECIFIED.,.F.,.F.,(4,4),(1.01328568624373,1.78536189863605),
 .UNSPECIFIED.);
#626=B_SPLINE_CURVE_WITH_KNOTS('',3,(#61257,#61258,#61259,#61260,#61261,
#61262,#61263,#61264,#61265,#61266,#61267,#61268,#61269,#61270,#61271,#61272,
#61273,#61274,#61275,#61276,#61277,#61278,#61279,#61280,#61281,#61282,#61283,
#61284,#61285,#61286,#61287),.UNSPECIFIED.,.F.,.F.,(4,3,2,2,2,2,2,2,2,2,
2,2,2,2,4),(0.214163227112882,0.2152214861059,0.217879469862119,0.221777671200573,
0.230219855502071,0.250403074207417,0.259557360890015,0.265568825998235,
0.270963492844559,0.277449943930359,0.288207765291046,0.310806527041239,
0.318607986179761,0.322642260335215,0.32495809229541),.UNSPECIFIED.);
#627=B_SPLINE_CURVE_WITH_KNOTS('',3,(#61293,#61294,#61295,#61296,#61297,
#61298,#61299,#61300,#61301,#61302,#61303,#61304,#61305,#61306,#61307,#61308,
#61309,#61310,#61311,#61312,#61313,#61314,#61315,#61316,#61317,#61318,#61319,
#61320),.UNSPECIFIED.,.F.,.F.,(4,2,2,2,2,2,2,2,2,2,2,2,2,4),(0.00054453433164722,
0.00261482456114446,0.00566461966673683,0.0105091351702915,0.0191944344367266,
0.0290670708677166,0.0385711889144227,0.0479537091672655,0.0577071236211236,
0.0693239193616052,0.0751757940684493,0.0775973271907055,0.0787013178396817,
0.0793612583163766),.UNSPECIFIED.);
#628=B_SPLINE_CURVE_WITH_KNOTS('',3,(#61329,#61330,#61331,#61332),
 .UNSPECIFIED.,.F.,.F.,(4,4),(0.972622216146952,1.74476629192075),
 .UNSPECIFIED.);
#629=B_SPLINE_CURVE_WITH_KNOTS('',3,(#61337,#61338,#61339,#61340),
 .UNSPECIFIED.,.F.,.F.,(4,4),(1.00913865884317,1.78128273461697),
 .UNSPECIFIED.);
#630=B_SPLINE_CURVE_WITH_KNOTS('',3,(#61345,#61346,#61347,#61348,#61349,
#61350,#61351,#61352,#61353,#61354,#61355,#61356,#61357,#61358,#61359,#61360,
#61361,#61362,#61363,#61364,#61365,#61366,#61367,#61368,#61369,#61370,#61371),
 .UNSPECIFIED.,.F.,.F.,(4,3,2,2,2,2,2,2,2,2,2,2,4),(0.227117616568572,0.228178838538054,
0.23085319458203,0.2348063115986,0.242541867562663,0.25646456183274,0.270271019860633,
0.284767676911501,0.299196973947014,0.314541585779187,0.323020081010486,
0.32806171188747,0.331723678708352),.UNSPECIFIED.);
#631=B_SPLINE_CURVE_WITH_KNOTS('',3,(#61377,#61378,#61379,#61380,#61381,
#61382,#61383,#61384,#61385,#61386,#61387,#61388,#61389,#61390,#61391,#61392,
#61393,#61394,#61395,#61396,#61397,#61398,#61399,#61400,#61401,#61402,#61403,
#61404),.UNSPECIFIED.,.F.,.F.,(4,2,2,2,2,2,2,2,2,2,2,2,2,4),(0.000544534549922002,
0.00261501248850168,0.00567325101762992,0.0105645437460407,0.0195297150491683,
0.02910971181855,0.0371551154137714,0.0446716615982893,0.0528464746815175,
0.0626030531722652,0.0695733104344749,0.0738617500894217,0.0760814802246236,
0.077641968937222),.UNSPECIFIED.);
#632=B_SPLINE_CURVE_WITH_KNOTS('',3,(#61413,#61414,#61415,#61416),
 .UNSPECIFIED.,.F.,.F.,(4,4),(0.950799700125448,1.72299586285748),
 .UNSPECIFIED.);
#633=B_SPLINE_CURVE_WITH_KNOTS('',3,(#61421,#61422,#61423,#61424),
 .UNSPECIFIED.,.F.,.F.,(4,4),(1.00192780386193,1.77412396659396),
 .UNSPECIFIED.);
#634=B_SPLINE_CURVE_WITH_KNOTS('',3,(#61429,#61430,#61431,#61432,#61433,
#61434,#61435,#61436,#61437,#61438,#61439,#61440,#61441,#61442,#61443,#61444,
#61445,#61446,#61447,#61448,#61449,#61450,#61451,#61452,#61453,#61454,#61455,
#61456,#61457,#61458,#61459),.UNSPECIFIED.,.F.,.F.,(4,3,2,2,2,2,2,2,2,2,
2,2,2,2,4),(0.182138855853588,0.183202254111611,0.18582100801444,0.189544523354996,
0.197294447984825,0.212715272503066,0.222658444671696,0.230577174766701,
0.238278170344655,0.247433567011968,0.261550284889895,0.268370460412409,
0.271469240196732,0.273499326100605,0.273748394097555),.UNSPECIFIED.);
#635=B_SPLINE_CURVE_WITH_KNOTS('',3,(#61465,#61466,#61467,#61468,#61469,
#61470,#61471,#61472,#61473,#61474,#61475,#61476,#61477,#61478,#61479,#61480,
#61481,#61482,#61483,#61484,#61485,#61486,#61487,#61488,#61489,#61490,#61491,
#61492),.UNSPECIFIED.,.F.,.F.,(4,2,2,2,2,2,2,2,2,2,2,2,2,4),(0.000544534331647472,
0.00261482456118744,0.00566461966693007,0.0105091351706961,0.0191944344374862,
0.0290670708688384,0.038571188915895,0.0479537091691038,0.0577071236233409,
0.0693239193640677,0.0751757940709175,0.0775973271931683,0.0787013178421332,
0.0793612583192019),.UNSPECIFIED.);
#636=B_SPLINE_CURVE_WITH_KNOTS('',3,(#61501,#61502,#61503,#61504),
 .UNSPECIFIED.,.F.,.F.,(4,4),(0.972622216146952,1.74476629192075),
 .UNSPECIFIED.);
#637=B_SPLINE_CURVE_WITH_KNOTS('',3,(#61509,#61510,#61511,#61512),
 .UNSPECIFIED.,.F.,.F.,(4,4),(1.00913865884316,1.78128273461697),
 .UNSPECIFIED.);
#638=B_SPLINE_CURVE_WITH_KNOTS('',3,(#61517,#61518,#61519,#61520,#61521,
#61522,#61523,#61524,#61525,#61526,#61527,#61528,#61529,#61530,#61531,#61532,
#61533,#61534,#61535,#61536,#61537,#61538,#61539,#61540,#61541,#61542,#61543),
 .UNSPECIFIED.,.F.,.F.,(4,3,2,2,2,2,2,2,2,2,2,2,4),(0.227117616563379,0.228178838532859,
0.230853194576822,0.234806311593326,0.242541867557314,0.256464561827109,
0.270271019854512,0.284767676904874,0.299196973939905,0.314541585771469,
0.323020081002407,0.328061711879166,0.331723678699876),.UNSPECIFIED.);
#639=B_SPLINE_CURVE_WITH_KNOTS('',3,(#61549,#61550,#61551,#61552,#61553,
#61554,#61555,#61556,#61557,#61558,#61559,#61560,#61561,#61562,#61563,#61564,
#61565,#61566,#61567,#61568,#61569,#61570,#61571,#61572,#61573,#61574,#61575,
#61576,#61577,#61578),.UNSPECIFIED.,.F.,.F.,(4,2,2,2,2,2,2,2,2,2,2,2,2,
2,4),(0.000544534825881866,0.0026152500862124,0.00568461736659321,0.010641823382684,
0.0201008495156089,0.0304143386679182,0.0361114853261834,0.0403561760954716,
0.0445829196062999,0.0502045803088476,0.0603086223202356,0.0719443717502886,
0.0783632098891355,0.0816596255879025,0.0839489901469663),.UNSPECIFIED.);
#640=B_SPLINE_CURVE_WITH_KNOTS('',3,(#61587,#61588,#61589,#61590),
 .UNSPECIFIED.,.F.,.F.,(4,4),(1.01074747522778,1.7828236876201),
 .UNSPECIFIED.);
#641=B_SPLINE_CURVE_WITH_KNOTS('',3,(#61595,#61596,#61597,#61598),
 .UNSPECIFIED.,.F.,.F.,(4,4),(1.01328568624373,1.78536189863605),
 .UNSPECIFIED.);
#642=B_SPLINE_CURVE_WITH_KNOTS('',3,(#61603,#61604,#61605,#61606,#61607,
#61608,#61609,#61610,#61611,#61612,#61613,#61614,#61615,#61616,#61617,#61618,
#61619,#61620,#61621,#61622,#61623,#61624,#61625,#61626,#61627,#61628,#61629,
#61630,#61631,#61632,#61633),.UNSPECIFIED.,.F.,.F.,(4,3,2,2,2,2,2,2,2,2,
2,2,2,2,4),(0.214163227120275,0.21522148611331,0.217879469869546,0.221777671208067,
0.230219855509598,0.250403074215009,0.259557360897752,0.265568826006071,
0.270963492852547,0.27744994393859,0.28820776529971,0.31080652705091,0.318607986189639,
0.322642260345161,0.32495809230541),.UNSPECIFIED.);
#643=B_SPLINE_CURVE_WITH_KNOTS('',3,(#61639,#61640,#61641,#61642,#61643,
#61644,#61645,#61646,#61647,#61648,#61649,#61650,#61651,#61652,#61653,#61654,
#61655,#61656,#61657,#61658,#61659,#61660,#61661,#61662,#61663,#61664,#61665,
#61666,#61667,#61668),.UNSPECIFIED.,.F.,.F.,(4,2,2,2,2,2,2,2,2,2,2,2,2,
2,4),(0.000544534825858864,0.00261525008194115,0.00568461734666706,0.0106418233374189,
0.0201008494219882,0.0304143385217521,0.0361114851509788,0.0403561758986649,
0.0445829193879516,0.0502045800618104,0.0603086220216309,0.0719443713921984,
0.0783632094984663,0.0816596251806001,0.0839489897352971),.UNSPECIFIED.);
#644=B_SPLINE_CURVE_WITH_KNOTS('',3,(#61677,#61678,#61679,#61680),
 .UNSPECIFIED.,.F.,.F.,(4,4),(1.01074747522778,1.7828236876201),
 .UNSPECIFIED.);
#645=B_SPLINE_CURVE_WITH_KNOTS('',3,(#61685,#61686,#61687,#61688),
 .UNSPECIFIED.,.F.,.F.,(4,4),(1.01328568624373,1.78536189863605),
 .UNSPECIFIED.);
#646=B_SPLINE_CURVE_WITH_KNOTS('',3,(#61693,#61694,#61695,#61696,#61697,
#61698,#61699,#61700,#61701,#61702,#61703,#61704,#61705,#61706,#61707,#61708,
#61709,#61710,#61711,#61712,#61713,#61714,#61715,#61716,#61717,#61718,#61719,
#61720,#61721,#61722,#61723),.UNSPECIFIED.,.F.,.F.,(4,3,2,2,2,2,2,2,2,2,
2,2,2,2,4),(0.214163227112987,0.215221486106032,0.217879469862266,0.221777671200784,
0.230219855502338,0.250403074207541,0.259557360890072,0.26556882599823,
0.270963492844479,0.277449943930284,0.288207765291006,0.310806527041273,
0.318607986179768,0.322642260335182,0.324958092295364),.UNSPECIFIED.);
#647=B_SPLINE_CURVE_WITH_KNOTS('',3,(#61729,#61730,#61731,#61732,#61733,
#61734,#61735,#61736,#61737,#61738,#61739,#61740,#61741,#61742,#61743,#61744,
#61745,#61746,#61747,#61748,#61749,#61750,#61751,#61752,#61753,#61754,#61755,
#61756),.UNSPECIFIED.,.F.,.F.,(4,2,2,2,2,2,2,2,2,2,2,2,2,4),(0.000544534331721061,
0.00261482457482928,0.00566461973037777,0.0105091353133324,0.0191944347221026,
0.0290670713146547,0.0385711895168917,0.0479537099233027,0.0577071245367978,
0.0693239204673549,0.075175795269208,0.0775973284310792,0.0787013190980296,
0.079361259569235),.UNSPECIFIED.);
#648=B_SPLINE_CURVE_WITH_KNOTS('',3,(#61765,#61766,#61767,#61768),
 .UNSPECIFIED.,.F.,.F.,(4,4),(0.972622216146951,1.74476629192075),
 .UNSPECIFIED.);
#649=B_SPLINE_CURVE_WITH_KNOTS('',3,(#61773,#61774,#61775,#61776),
 .UNSPECIFIED.,.F.,.F.,(4,4),(1.00913865884317,1.78128273461697),
 .UNSPECIFIED.);
#650=B_SPLINE_CURVE_WITH_KNOTS('',3,(#61781,#61782,#61783,#61784,#61785,
#61786,#61787,#61788,#61789,#61790,#61791,#61792,#61793,#61794,#61795,#61796,
#61797,#61798,#61799,#61800,#61801,#61802,#61803,#61804,#61805,#61806,#61807),
 .UNSPECIFIED.,.F.,.F.,(4,3,2,2,2,2,2,2,2,2,2,2,4),(0.22711761655784,0.228178838527325,
0.230853194571298,0.234806311587849,0.242541867551889,0.256464561821621,
0.270271019848905,0.284767676899163,0.299196973934087,0.314541585765277,
0.323020080995849,0.328061711872383,0.331723678692964),.UNSPECIFIED.);
#651=B_SPLINE_CURVE_WITH_KNOTS('',3,(#61813,#61814,#61815,#61816,#61817,
#61818,#61819,#61820,#61821,#61822,#61823,#61824,#61825,#61826,#61827,#61828,
#61829,#61830,#61831,#61832,#61833,#61834,#61835,#61836,#61837,#61838,#61839,
#61840),.UNSPECIFIED.,.F.,.F.,(4,2,2,2,2,2,2,2,2,2,2,2,2,4),(0.00054453455021207,
0.00261501254235662,0.00567325126835114,0.0105645443117739,0.0195297161928756,
0.0291097135789848,0.0371551176921656,0.0446716643607754,0.0528464779706515,
0.0626030570899518,0.0695733147999327,0.07386175473079,0.0760814850088403,
0.0776419737362139),.UNSPECIFIED.);
#652=B_SPLINE_CURVE_WITH_KNOTS('',3,(#61849,#61850,#61851,#61852),
 .UNSPECIFIED.,.F.,.F.,(4,4),(0.950799700125448,1.72299586285748),
 .UNSPECIFIED.);
#653=B_SPLINE_CURVE_WITH_KNOTS('',3,(#61857,#61858,#61859,#61860),
 .UNSPECIFIED.,.F.,.F.,(4,4),(1.00192780386193,1.77412396659396),
 .UNSPECIFIED.);
#654=B_SPLINE_CURVE_WITH_KNOTS('',3,(#61865,#61866,#61867,#61868,#61869,
#61870,#61871,#61872,#61873,#61874,#61875,#61876,#61877,#61878,#61879,#61880,
#61881,#61882,#61883,#61884,#61885,#61886,#61887,#61888,#61889,#61890,#61891,
#61892,#61893,#61894,#61895),.UNSPECIFIED.,.F.,.F.,(4,3,2,2,2,2,2,2,2,2,
2,2,2,2,4),(0.182138855853748,0.183202254111772,0.185821008014603,0.189544523355168,
0.197294447985023,0.212715272503339,0.222658444672033,0.230577174767099,
0.238278170345122,0.247433567012527,0.261550284890583,0.268370460413101,
0.271469240197419,0.273499326101292,0.273748394098242),.UNSPECIFIED.);
#655=B_SPLINE_CURVE_WITH_KNOTS('',3,(#62088,#62089,#62090,#62091),
 .UNSPECIFIED.,.F.,.F.,(4,4),(0.0459042098603345,0.091874680867398),
 .UNSPECIFIED.);
#656=B_SPLINE_CURVE_WITH_KNOTS('',3,(#62094,#62095,#62096,#62097),
 .UNSPECIFIED.,.F.,.F.,(4,4),(0.0459042098603146,0.0918746808673364),
 .UNSPECIFIED.);
#657=B_SPLINE_CURVE_WITH_KNOTS('',3,(#62163,#62164,#62165,#62166),
 .UNSPECIFIED.,.F.,.F.,(4,4),(0.0459042098603271,0.0918746808673741),
 .UNSPECIFIED.);
#658=B_SPLINE_CURVE_WITH_KNOTS('',3,(#62169,#62170,#62171,#62172),
 .UNSPECIFIED.,.F.,.F.,(4,4),(0.,0.0459735749039228),.UNSPECIFIED.);
#659=B_SPLINE_CURVE_WITH_KNOTS('',3,(#62394,#62395,#62396,#62397),
 .UNSPECIFIED.,.F.,.F.,(4,4),(0.0459042098603282,0.0918746808673777),
 .UNSPECIFIED.);
#660=B_SPLINE_CURVE_WITH_KNOTS('',3,(#62400,#62401,#62402,#62403),
 .UNSPECIFIED.,.F.,.F.,(4,4),(0.04590420986033,0.0918746808673833),
 .UNSPECIFIED.);
#661=B_SPLINE_CURVE_WITH_KNOTS('',3,(#62539,#62540,#62541,#62542),
 .UNSPECIFIED.,.F.,.F.,(4,4),(-0.0918808841872258,0.),.UNSPECIFIED.);
#662=B_SPLINE_CURVE_WITH_KNOTS('',3,(#62546,#62547,#62548,#62549),
 .UNSPECIFIED.,.F.,.F.,(4,4),(-0.0918746808673604,0.),.UNSPECIFIED.);
#663=B_SPLINE_CURVE_WITH_KNOTS('',3,(#62552,#62553,#62554,#62555),
 .UNSPECIFIED.,.F.,.F.,(4,4),(-0.0918808841872082,0.),.UNSPECIFIED.);
#664=B_SPLINE_CURVE_WITH_KNOTS('',3,(#62561,#62562,#62563,#62564),
 .UNSPECIFIED.,.F.,.F.,(4,4),(-0.0918808841872279,0.),.UNSPECIFIED.);
#665=B_SPLINE_CURVE_WITH_KNOTS('',3,(#62569,#62570,#62571,#62572),
 .UNSPECIFIED.,.F.,.F.,(4,4),(-0.0918746808673616,0.),.UNSPECIFIED.);
#666=B_SPLINE_CURVE_WITH_KNOTS('',3,(#62575,#62576,#62577,#62578),
 .UNSPECIFIED.,.F.,.F.,(4,4),(-0.0918808841872121,0.),.UNSPECIFIED.);
#667=B_SPLINE_CURVE_WITH_KNOTS('',3,(#62592,#62593,#62594,#62595),
 .UNSPECIFIED.,.F.,.F.,(4,4),(-0.0918746808673705,0.),.UNSPECIFIED.);
#668=B_SPLINE_CURVE_WITH_KNOTS('',3,(#62612,#62613,#62614,#62615),
 .UNSPECIFIED.,.F.,.F.,(4,4),(-0.0918746808673773,0.),.UNSPECIFIED.);
#669=B_SPLINE_CURVE_WITH_KNOTS('',3,(#62627,#62628,#62629,#62630),
 .UNSPECIFIED.,.F.,.F.,(4,4),(-0.0918746808673589,0.),.UNSPECIFIED.);
#670=B_SPLINE_CURVE_WITH_KNOTS('',3,(#62654,#62655,#62656,#62657),
 .UNSPECIFIED.,.F.,.F.,(4,4),(0.,0.0417760674242005),.UNSPECIFIED.);
#671=B_SPLINE_CURVE_WITH_KNOTS('',3,(#62726,#62727,#62728,#62729),
 .UNSPECIFIED.,.F.,.F.,(4,4),(-0.0918746808673938,0.),.UNSPECIFIED.);
#672=B_SPLINE_CURVE_WITH_KNOTS('',3,(#62740,#62741,#62742,#62743),
 .UNSPECIFIED.,.F.,.F.,(4,4),(-0.0918808841872246,0.),.UNSPECIFIED.);
#673=B_SPLINE_CURVE_WITH_KNOTS('',3,(#62771,#62772,#62773,#62774),
 .UNSPECIFIED.,.F.,.F.,(4,4),(-0.0918808841872257,0.),.UNSPECIFIED.);
#674=B_SPLINE_CURVE_WITH_KNOTS('',3,(#62831,#62832,#62833,#62834,#62835,
#62836),.UNSPECIFIED.,.F.,.F.,(4,2,4),(-0.0699398717026881,-0.0424031601887617,
-0.0310509275685648),.UNSPECIFIED.);
#675=B_SPLINE_CURVE_WITH_KNOTS('',3,(#62842,#62843,#62844,#62845,#62846,
#62847),.UNSPECIFIED.,.F.,.F.,(4,2,4),(-0.0581997287702625,-0.0419989606450143,
-0.0194152449888361),.UNSPECIFIED.);
#676=B_SPLINE_CURVE_WITH_KNOTS('',3,(#62850,#62851,#62852,#62853,#62854,
#62855,#62856,#62857,#62858,#62859,#62860,#62861,#62862,#62863,#62864,#62865),
 .UNSPECIFIED.,.F.,.F.,(4,2,2,2,2,2,2,4),(0.0233074596666565,0.0349077749662999,
0.0719158476770912,0.110933651903281,0.149781045314824,0.188810000879272,
0.217148839309655,0.222449805752671),.UNSPECIFIED.);
#677=B_SPLINE_CURVE_WITH_KNOTS('',3,(#62897,#62898,#62899,#62900),
 .UNSPECIFIED.,.F.,.F.,(4,4),(0.0179911303970816,0.0747141480456938),
 .UNSPECIFIED.);
#678=B_SPLINE_CURVE_WITH_KNOTS('',3,(#62904,#62905,#62906,#62907),
 .UNSPECIFIED.,.F.,.F.,(4,4),(0.0179911303970802,0.0747141480456902),
 .UNSPECIFIED.);
#679=B_SPLINE_CURVE_WITH_KNOTS('',3,(#62938,#62939,#62940,#62941),
 .UNSPECIFIED.,.F.,.F.,(4,4),(0.,0.0567455036329469),.UNSPECIFIED.);
#680=B_SPLINE_CURVE_WITH_KNOTS('',3,(#62945,#62946,#62947,#62948),
 .UNSPECIFIED.,.F.,.F.,(4,4),(0.0179911303970801,0.0747141480456939),
 .UNSPECIFIED.);
#681=B_SPLINE_CURVE_WITH_KNOTS('',3,(#62966,#62967,#62968,#62969,#62970,
#62971,#62972,#62973,#62974,#62975,#62976,#62977,#62978,#62979,#62980,#62981,
#62982,#62983,#62984,#62985,#62986,#62987,#62988),.UNSPECIFIED.,.F.,.F.,
(4,2,2,2,2,2,2,2,2,3,4),(-0.598135905708757,-0.517314332218455,-0.362696133580663,
-0.318209117763193,-0.286159070534776,-0.258657166109227,-0.231155261683679,
-0.199105214455262,-0.154618198637792,0.,0.0808215734903014),
 .UNSPECIFIED.);
#682=B_SPLINE_CURVE_WITH_KNOTS('',3,(#63099,#63100,#63101,#63102,#63103,
#63104,#63105,#63106,#63107,#63108,#63109,#63110,#63111,#63112,#63113,#63114),
 .UNSPECIFIED.,.F.,.F.,(4,3,3,3,3,4),(-4.04486473697844,-3.98046853915737,
-3.4829099717627,-2.98535140436803,-2.48779283697336,-2.01331729429997),
 .UNSPECIFIED.);
#683=B_SPLINE_CURVE_WITH_KNOTS('',3,(#63117,#63118,#63119,#63120,#63121,
#63122,#63123,#63124,#63125,#63126),.UNSPECIFIED.,.F.,.F.,(4,3,3,4),(0.,
0.497558567394675,0.995117134789351,1.11004521091141),.UNSPECIFIED.);
#684=B_SPLINE_CURVE_WITH_KNOTS('',3,(#63131,#63132,#63133,#63134,#63135,
#63136,#63137,#63138,#63139,#63140,#63141,#63142,#63143,#63144,#63145,#63146,
#63147,#63148,#63149,#63150,#63151,#63152,#63153,#63154,#63155,#63156,#63157,
#63158,#63159,#63160,#63161,#63162,#63163,#63164,#63165,#63166,#63167,#63168,
#63169,#63170),.UNSPECIFIED.,.F.,.F.,(4,3,3,3,3,3,3,3,3,3,3,3,3,4),(-10.328050044158,
-9.95117134789344,-9.45361278049877,-8.95605421310409,-8.45849564570942,
-7.96093707831475,-7.46337851092008,-6.96581994352541,-6.46826137613073,
-5.97070280873606,-5.47314424134139,-4.97558567394672,-4.47802710655205,
-4.04486473697844),.UNSPECIFIED.);
#685=B_SPLINE_CURVE_WITH_KNOTS('',3,(#63171,#63172,#63173,#63174,#63175,
#63176,#63177,#63178,#63179,#63180,#63181,#63182,#63183,#63184,#63185,#63186,
#63187,#63188,#63189,#63190,#63191,#63192,#63193,#63194,#63195,#63196,#63197,
#63198,#63199,#63200,#63201,#63202,#63203,#63204,#63205,#63206,#63207,#63208,
#63209,#63210),.UNSPECIFIED.,.F.,.F.,(4,3,3,3,3,3,3,3,3,3,3,3,3,4),(1.11004521091141,
1.49267570218402,1.99023426957869,2.48779283697337,2.98535140436804,3.48290997176271,
3.98046853915738,4.47802710655206,4.97558567394673,5.4731442413414,5.97070280873607,
6.46826137613074,6.96581994352541,7.39323051809098),.UNSPECIFIED.);
#686=B_SPLINE_CURVE_WITH_KNOTS('',3,(#63215,#63216,#63217,#63218,#63219,
#63220,#63221,#63222,#63223,#63224,#63225,#63226,#63227,#63228,#63229,#63230,
#63231,#63232,#63233,#63234,#63235,#63236,#63237,#63238,#63239,#63240,#63241,
#63242,#63243,#63244,#63245,#63246,#63247,#63248,#63249,#63250,#63251,#63252,
#63253,#63254,#63255,#63256,#63257),.UNSPECIFIED.,.F.,.F.,(4,3,3,3,3,3,
3,3,3,3,3,3,3,3,4),(-16.6112353513376,-16.4194327240242,-15.9218741566295,
-15.4243155892348,-14.9267570218402,-14.4291984544455,-13.9316398870508,
-13.4340813196561,-12.9365227522615,-12.4389641848668,-11.9414056174721,
-11.4438470500775,-10.9462884826828,-10.4487299152881,-10.328050044158),
 .UNSPECIFIED.);
#687=B_SPLINE_CURVE_WITH_KNOTS('',3,(#63258,#63259,#63260,#63261,#63262,
#63263,#63264,#63265,#63266,#63267,#63268,#63269,#63270,#63271,#63272,#63273,
#63274,#63275,#63276,#63277,#63278,#63279,#63280,#63281,#63282,#63283,#63284,
#63285,#63286,#63287,#63288,#63289,#63290,#63291,#63292,#63293,#63294,#63295,
#63296,#63297,#63298,#63299,#63300),.UNSPECIFIED.,.F.,.F.,(4,3,3,3,3,3,
3,3,3,3,3,3,3,3,4),(7.39323051809098,7.46337851092009,7.96093707831476,
8.45849564570943,8.9560542131041,9.45361278049877,9.95117134789344,10.4487299152881,
10.9462884826828,11.4438470500775,11.9414056174721,12.4389641848668,12.9365227522615,
13.4340813196561,13.6764158252706),.UNSPECIFIED.);
#688=B_SPLINE_CURVE_WITH_KNOTS('',3,(#63305,#63306,#63307,#63308,#63309,
#63310,#63311,#63312,#63313,#63314,#63315,#63316,#63317,#63318,#63319,#63320,
#63321,#63322,#63323,#63324,#63325,#63326,#63327,#63328,#63329,#63330,#63331,
#63332,#63333,#63334,#63335,#63336,#63337,#63338,#63339,#63340,#63341,#63342,
#63343,#63344,#63345,#63346,#63347),.UNSPECIFIED.,.F.,.F.,(4,3,3,3,3,3,
3,3,3,3,3,3,3,3,4),(-22.8944206585172,-22.8876941001549,-22.3901355327602,
-21.8925769653656,-21.3950183979709,-20.8974598305762,-20.3999012631815,
-19.9023426957869,-19.4047841283922,-18.9072255609975,-18.4096669936029,
-17.9121084262082,-17.4145498588135,-16.9169912914188,-16.6112353513376),
 .UNSPECIFIED.);
#689=B_SPLINE_CURVE_WITH_KNOTS('',3,(#63348,#63349,#63350,#63351,#63352,
#63353,#63354,#63355,#63356,#63357,#63358,#63359,#63360,#63361,#63362,#63363,
#63364,#63365,#63366,#63367,#63368,#63369,#63370,#63371,#63372,#63373,#63374,
#63375,#63376,#63377,#63378,#63379,#63380,#63381,#63382,#63383,#63384,#63385,
#63386,#63387,#63388,#63389,#63390),.UNSPECIFIED.,.F.,.F.,(4,3,3,3,3,3,
3,3,3,3,3,3,3,3,4),(13.6764158252706,13.9316398870508,14.4291984544455,
14.9267570218402,15.4243155892348,15.9218741566295,16.4194327240242,16.9169912914188,
17.4145498588135,17.9121084262082,18.4096669936029,18.9072255609975,19.4047841283922,
19.9023426957869,19.9596011324502),.UNSPECIFIED.);
#690=B_SPLINE_CURVE_WITH_KNOTS('',3,(#63395,#63396,#63397,#63398,#63399,
#63400,#63401,#63402,#63403,#63404,#63405,#63406,#63407,#63408,#63409,#63410,
#63411,#63412,#63413,#63414,#63415,#63416,#63417,#63418,#63419,#63420,#63421,
#63422,#63423,#63424,#63425,#63426,#63427,#63428,#63429,#63430,#63431,#63432,
#63433,#63434),.UNSPECIFIED.,.F.,.F.,(4,3,3,3,3,3,3,3,3,3,3,3,3,4),(-29.1776059656968,
-28.858396908891,-28.3608383414963,-27.8632797741016,-27.3657212067069,
-26.8681626393123,-26.3706040719176,-25.8730455045229,-25.3754869371283,
-24.8779283697336,-24.3803698023389,-23.8828112349442,-23.3852526675496,
-22.8944206585172),.UNSPECIFIED.);
#691=B_SPLINE_CURVE_WITH_KNOTS('',3,(#63435,#63436,#63437,#63438,#63439,
#63440,#63441,#63442,#63443,#63444,#63445,#63446,#63447,#63448,#63449,#63450,
#63451,#63452,#63453,#63454,#63455,#63456,#63457,#63458,#63459,#63460,#63461,
#63462,#63463,#63464,#63465,#63466,#63467,#63468,#63469,#63470,#63471,#63472,
#63473,#63474),.UNSPECIFIED.,.F.,.F.,(4,3,3,3,3,3,3,3,3,3,3,3,3,4),(19.9596011324502,
20.3999012631816,20.8974598305762,21.3950183979709,21.8925769653656,22.3901355327602,
22.8876941001549,23.3852526675496,23.8828112349443,24.3803698023389,24.8779283697336,
25.3754869371283,25.8730455045229,26.2427864396298),.UNSPECIFIED.);
#692=B_SPLINE_CURVE_WITH_KNOTS('',3,(#63479,#63480,#63481,#63482,#63483,
#63484,#63485,#63486,#63487,#63488,#63489,#63490,#63491,#63492,#63493,#63494,
#63495,#63496,#63497,#63498,#63499,#63500,#63501,#63502,#63503,#63504,#63505,
#63506,#63507,#63508,#63509,#63510,#63511,#63512,#63513,#63514,#63515,#63516,
#63517,#63518,#63519,#63520,#63521),.UNSPECIFIED.,.F.,.F.,(4,3,3,3,3,3,
3,3,3,3,3,3,3,3,4),(-35.4607912728764,-35.3266582850217,-34.829099717627,
-34.3315411502324,-33.8339825828377,-33.336424015443,-32.8388654480483,
-32.3413068806537,-31.843748313259,-31.3461897458643,-30.8486311784696,
-30.351072611075,-29.8535140436803,-29.3559554762856,-29.1776059656968),
 .UNSPECIFIED.);
#693=B_SPLINE_CURVE_WITH_KNOTS('',3,(#63522,#63523,#63524,#63525,#63526,
#63527,#63528,#63529,#63530,#63531,#63532,#63533,#63534,#63535,#63536,#63537,
#63538,#63539,#63540,#63541,#63542,#63543,#63544,#63545,#63546,#63547,#63548,
#63549,#63550,#63551,#63552,#63553,#63554,#63555,#63556,#63557,#63558,#63559,
#63560,#63561,#63562,#63563,#63564),.UNSPECIFIED.,.F.,.F.,(4,3,3,3,3,3,
3,3,3,3,3,3,3,3,4),(26.2427864396298,26.3706040719176,26.8681626393123,
27.365721206707,27.8632797741016,28.3608383414963,28.858396908891,29.3559554762856,
29.8535140436803,30.351072611075,30.8486311784697,31.3461897458643,31.843748313259,
32.3413068806537,32.5259717468093),.UNSPECIFIED.);
#694=B_SPLINE_CURVE_WITH_KNOTS('',3,(#63569,#63570,#63571,#63572,#63573,
#63574,#63575,#63576,#63577,#63578,#63579,#63580,#63581,#63582,#63583,#63584,
#63585,#63586,#63587,#63588,#63589,#63590,#63591,#63592,#63593,#63594,#63595,
#63596,#63597,#63598,#63599,#63600,#63601,#63602,#63603,#63604,#63605,#63606,
#63607,#63608),.UNSPECIFIED.,.F.,.F.,(4,3,3,3,3,3,3,3,3,3,3,3,3,4),(-41.743976580056,
-41.2973610937578,-40.7998025263631,-40.3022439589684,-39.8046853915737,
-39.3071268241791,-38.8095682567844,-38.3120096893897,-37.8144511219951,
-37.3168925546004,-36.8193339872057,-36.321775419811,-35.8242168524164,
-35.4607912728764),.UNSPECIFIED.);
#695=B_SPLINE_CURVE_WITH_KNOTS('',3,(#63609,#63610,#63611,#63612,#63613,
#63614,#63615,#63616,#63617,#63618,#63619,#63620,#63621,#63622,#63623,#63624,
#63625,#63626,#63627,#63628,#63629,#63630,#63631,#63632,#63633,#63634,#63635,
#63636,#63637,#63638,#63639,#63640,#63641,#63642,#63643,#63644,#63645,#63646,
#63647,#63648),.UNSPECIFIED.,.F.,.F.,(4,3,3,3,3,3,3,3,3,3,3,3,3,4),(32.5259717468093,
32.8388654480483,33.336424015443,33.8339825828377,34.3315411502324,34.829099717627,
35.3266582850217,35.8242168524164,36.3217754198111,36.8193339872057,37.3168925546004,
37.8144511219951,38.3120096893898,38.8091570539889),.UNSPECIFIED.);
#696=B_SPLINE_CURVE_WITH_KNOTS('',3,(#63653,#63654,#63655,#63656,#63657,
#63658,#63659,#63660,#63661,#63662,#63663,#63664,#63665,#63666,#63667,#63668,
#63669,#63670,#63671,#63672,#63673,#63674,#63675,#63676,#63677,#63678,#63679,
#63680,#63681,#63682,#63683,#63684,#63685,#63686,#63687,#63688,#63689,#63690,
#63691,#63692,#63693,#63694,#63695),.UNSPECIFIED.,.F.,.F.,(4,3,3,3,3,3,
3,3,3,3,3,3,3,3,4),(-48.0271618872356,-47.7656224698885,-47.2680639024938,
-46.7705053350992,-46.2729467677045,-45.7753882003098,-45.2778296329151,
-44.7802710655205,-44.2827124981258,-43.7851539307311,-43.2875953633364,
-42.7900367959418,-42.2924782285471,-41.7949196611524,-41.743976580056),
 .UNSPECIFIED.);
#697=B_SPLINE_CURVE_WITH_KNOTS('',3,(#63696,#63697,#63698,#63699,#63700,
#63701,#63702,#63703,#63704,#63705,#63706,#63707,#63708,#63709,#63710,#63711,
#63712,#63713,#63714,#63715,#63716,#63717,#63718,#63719,#63720,#63721,#63722,
#63723,#63724,#63725,#63726,#63727,#63728,#63729,#63730,#63731,#63732,#63733,
#63734,#63735),.UNSPECIFIED.,.F.,.F.,(4,3,3,3,3,3,3,3,3,3,3,3,3,4),(38.8091570539889,
39.3071268241791,39.8046853915738,40.3022439589684,40.7998025263631,41.2973610937578,
41.7949196611524,42.2924782285471,42.7900367959418,43.2875953633364,43.7851539307311,
44.2827124981258,44.7802710655205,45.0923423611685),.UNSPECIFIED.);
#698=B_SPLINE_CURVE_WITH_KNOTS('',3,(#63740,#63741,#63742,#63743,#63744,
#63745,#63746,#63747,#63748,#63749,#63750,#63751,#63752,#63753,#63754,#63755,
#63756,#63757,#63758,#63759,#63760,#63761,#63762,#63763,#63764,#63765,#63766,
#63767,#63768,#63769,#63770,#63771,#63772,#63773,#63774,#63775,#63776,#63777,
#63778,#63779,#63780,#63781,#63782),.UNSPECIFIED.,.F.,.F.,(4,3,3,3,3,3,
3,3,3,3,3,3,3,3,4),(-54.3103471944151,-54.2338838460192,-53.7363252786246,
-53.2387667112299,-52.7412081438352,-52.2436495764405,-51.7460910090459,
-51.2485324416512,-50.7509738742565,-50.2534153068619,-49.7558567394672,
-49.2582981720725,-48.7607396046778,-48.2631810372832,-48.0271618872356),
 .UNSPECIFIED.);
#699=B_SPLINE_CURVE_WITH_KNOTS('',3,(#63783,#63784,#63785,#63786,#63787,
#63788,#63789,#63790,#63791,#63792,#63793,#63794,#63795,#63796,#63797,#63798,
#63799,#63800,#63801,#63802,#63803,#63804,#63805,#63806,#63807,#63808,#63809,
#63810,#63811,#63812,#63813,#63814,#63815,#63816,#63817,#63818,#63819,#63820,
#63821,#63822,#63823,#63824,#63825),.UNSPECIFIED.,.F.,.F.,(4,3,3,3,3,3,
3,3,3,3,3,3,3,3,4),(45.0923423611685,45.2778296329151,45.7753882003098,
46.2729467677045,46.7705053350991,47.2680639024938,47.7656224698885,48.2631810372832,
48.7607396046778,49.2582981720725,49.7558567394672,50.2534153068619,50.7509738742565,
51.2485324416512,51.3755276683481),.UNSPECIFIED.);
#700=B_SPLINE_CURVE_WITH_KNOTS('',3,(#63830,#63831,#63832,#63833,#63834,
#63835,#63836,#63837,#63838,#63839,#63840,#63841,#63842,#63843,#63844,#63845,
#63846,#63847,#63848,#63849,#63850,#63851,#63852,#63853,#63854,#63855,#63856,
#63857,#63858,#63859,#63860,#63861,#63862,#63863,#63864,#63865,#63866,#63867,
#63868,#63869),.UNSPECIFIED.,.F.,.F.,(4,3,3,3,3,3,3,3,3,3,3,3,3,4),(-60.5935325015948,
-60.2045866547553,-59.7070280873606,-59.2094695199659,-58.7119109525713,
-58.2143523851766,-57.7167938177819,-57.2192352503872,-56.7216766829926,
-56.2241181155979,-55.7265595482032,-55.2290009808086,-54.7314424134139,
-54.3103471944151),.UNSPECIFIED.);
#701=B_SPLINE_CURVE_WITH_KNOTS('',3,(#63870,#63871,#63872,#63873,#63874,
#63875,#63876,#63877,#63878,#63879,#63880,#63881,#63882,#63883,#63884,#63885,
#63886,#63887,#63888,#63889,#63890,#63891,#63892,#63893,#63894,#63895,#63896,
#63897,#63898,#63899,#63900,#63901,#63902,#63903,#63904,#63905,#63906,#63907,
#63908,#63909),.UNSPECIFIED.,.F.,.F.,(4,3,3,3,3,3,3,3,3,3,3,3,3,4),(51.3755276683481,
51.7460910090459,52.2436495764406,52.7412081438352,53.2387667112299,53.7363252786246,
54.2338838460192,54.7314424134139,55.2290009808086,55.7265595482033,56.2241181155979,
56.7216766829926,57.2192352503873,57.6587129755277),.UNSPECIFIED.);
#702=B_SPLINE_CURVE_WITH_KNOTS('',3,(#63914,#63915,#63916,#63917,#63918,
#63919,#63920,#63921,#63922,#63923,#63924,#63925,#63926,#63927,#63928,#63929,
#63930,#63931,#63932,#63933,#63934,#63935,#63936,#63937,#63938,#63939,#63940,
#63941,#63942,#63943,#63944,#63945,#63946,#63947,#63948,#63949,#63950,#63951,
#63952,#63953,#63954,#63955,#63956),.UNSPECIFIED.,.F.,.F.,(4,3,3,3,3,3,
3,3,3,3,3,3,3,3,4),(-66.8767178087743,-66.672848030886,-66.1752894634913,
-65.6777308960967,-65.180172328702,-64.6826137613073,-64.1850551939127,
-63.687496626518,-63.1899380591233,-62.6923794917286,-62.194820924334,-61.6972623569393,
-61.1997037895446,-60.70214522215,-60.5935325015948),.UNSPECIFIED.);
#703=B_SPLINE_CURVE_WITH_KNOTS('',3,(#63957,#63958,#63959,#63960,#63961,
#63962,#63963,#63964,#63965,#63966,#63967,#63968,#63969,#63970,#63971,#63972,
#63973,#63974,#63975,#63976,#63977,#63978,#63979,#63980,#63981,#63982,#63983,
#63984,#63985,#63986,#63987,#63988,#63989,#63990,#63991,#63992,#63993,#63994,
#63995,#63996,#63997,#63998,#63999),.UNSPECIFIED.,.F.,.F.,(4,3,3,3,3,3,
3,3,3,3,3,3,3,3,4),(57.6587129755277,57.7167938177819,58.2143523851766,
58.7119109525713,59.2094695199659,59.7070280873606,60.2045866547553,60.70214522215,
61.1997037895446,61.6972623569393,62.194820924334,62.6923794917287,63.1899380591233,
63.687496626518,63.9418982827073),.UNSPECIFIED.);
#704=B_SPLINE_CURVE_WITH_KNOTS('',3,(#64004,#64005,#64006,#64007,#64008,
#64009,#64010,#64011,#64012,#64013,#64014,#64015,#64016,#64017,#64018,#64019,
#64020,#64021,#64022,#64023,#64024,#64025,#64026,#64027,#64028,#64029,#64030,
#64031,#64032,#64033,#64034,#64035,#64036,#64037,#64038,#64039,#64040,#64041,
#64042,#64043,#64044,#64045,#64046),.UNSPECIFIED.,.F.,.F.,(4,3,3,3,3,3,
3,3,3,3,3,3,3,3,4),(-73.1599031159539,-73.1411094070167,-72.6435508396221,
-72.1459922722274,-71.6484337048327,-71.150875137438,-70.6533165700434,
-70.1557580026487,-69.658199435254,-69.1606408678594,-68.6630823004647,
-68.16552373307,-67.6679651656754,-67.1704065982807,-66.8767178087743),
 .UNSPECIFIED.);
#705=B_SPLINE_CURVE_WITH_KNOTS('',3,(#64047,#64048,#64049,#64050,#64051,
#64052,#64053,#64054,#64055,#64056,#64057,#64058,#64059,#64060,#64061,#64062,
#64063,#64064,#64065,#64066,#64067,#64068,#64069,#64070,#64071,#64072,#64073,
#64074,#64075,#64076,#64077,#64078,#64079,#64080,#64081,#64082,#64083,#64084,
#64085,#64086,#64087,#64088,#64089),.UNSPECIFIED.,.F.,.F.,(4,3,3,3,3,3,
3,3,3,3,3,3,3,3,4),(63.9418982827073,64.1850551939127,64.6826137613073,
65.180172328702,65.6777308960967,66.1752894634914,66.672848030886,67.1704065982807,
67.6679651656754,68.16552373307,68.6630823004647,69.1606408678594,69.6581994352541,
70.1557580026487,70.2250835898869),.UNSPECIFIED.);
#706=B_SPLINE_CURVE_WITH_KNOTS('',3,(#64094,#64095,#64096,#64097,#64098,
#64099,#64100,#64101,#64102,#64103,#64104,#64105,#64106,#64107,#64108,#64109,
#64110,#64111,#64112,#64113,#64114,#64115,#64116,#64117,#64118,#64119,#64120,
#64121,#64122,#64123,#64124,#64125,#64126,#64127,#64128,#64129,#64130,#64131,
#64132,#64133),.UNSPECIFIED.,.F.,.F.,(4,3,3,3,3,3,3,3,3,3,3,3,3,4),(-79.4430884231335,
-79.1118122157528,-78.6142536483581,-78.1166950809635,-77.6191365135688,
-77.1215779461741,-76.6240193787795,-76.1264608113848,-75.6289022439901,
-75.1313436765954,-74.6337851092008,-74.1362265418061,-73.6386679744114,
-73.1599031159539),.UNSPECIFIED.);
#707=B_SPLINE_CURVE_WITH_KNOTS('',3,(#64134,#64135,#64136,#64137,#64138,
#64139,#64140,#64141,#64142,#64143,#64144,#64145,#64146,#64147,#64148,#64149,
#64150,#64151,#64152,#64153,#64154,#64155,#64156,#64157,#64158,#64159,#64160,
#64161,#64162,#64163,#64164,#64165,#64166,#64167,#64168,#64169,#64170,#64171,
#64172,#64173),.UNSPECIFIED.,.F.,.F.,(4,3,3,3,3,3,3,3,3,3,3,3,3,4),(70.2250835898869,
70.6533165700434,71.1508751374381,71.6484337048327,72.1459922722274,72.6435508396221,
73.1411094070168,73.6386679744114,74.1362265418061,74.6337851092008,75.1313436765954,
75.6289022439901,76.1264608113848,76.5082688970665),.UNSPECIFIED.);
#708=B_SPLINE_CURVE_WITH_KNOTS('',3,(#64178,#64179,#64180,#64181,#64182,
#64183,#64184,#64185,#64186,#64187,#64188,#64189,#64190,#64191,#64192,#64193,
#64194,#64195,#64196,#64197,#64198,#64199,#64200,#64201,#64202,#64203,#64204,
#64205,#64206,#64207,#64208,#64209,#64210,#64211,#64212,#64213,#64214,#64215,
#64216,#64217,#64218,#64219,#64220),.UNSPECIFIED.,.F.,.F.,(4,3,3,3,3,3,
3,3,3,3,3,3,3,3,4),(-85.7262737303131,-85.5800735918835,-85.0825150244889,
-84.5849564570942,-84.0873978896995,-83.5898393223049,-83.0922807549102,
-82.5947221875155,-82.0971636201208,-81.5996050527262,-81.1020464853315,
-80.6044879179368,-80.1069293505422,-79.6093707831475,-79.4430884231335),
 .UNSPECIFIED.);
#709=B_SPLINE_CURVE_WITH_KNOTS('',3,(#64221,#64222,#64223,#64224,#64225,
#64226,#64227,#64228,#64229,#64230,#64231,#64232,#64233,#64234,#64235,#64236,
#64237,#64238,#64239,#64240,#64241,#64242,#64243,#64244,#64245,#64246,#64247,
#64248,#64249,#64250,#64251,#64252,#64253,#64254,#64255,#64256,#64257,#64258,
#64259,#64260,#64261,#64262,#64263),.UNSPECIFIED.,.F.,.F.,(4,3,3,3,3,3,
3,3,3,3,3,3,3,3,4),(76.5082688970665,76.6240193787795,77.1215779461741,
77.6191365135688,78.1166950809635,78.6142536483582,79.1118122157528,79.6093707831475,
80.1069293505422,80.6044879179368,81.1020464853315,81.5996050527262,82.0971636201209,
82.5947221875155,82.7914542042461),.UNSPECIFIED.);
#710=B_SPLINE_CURVE_WITH_KNOTS('',3,(#64268,#64269,#64270,#64271,#64272,
#64273,#64274,#64275,#64276,#64277,#64278,#64279,#64280,#64281,#64282,#64283,
#64284,#64285,#64286,#64287,#64288,#64289,#64290,#64291,#64292,#64293,#64294,
#64295,#64296,#64297,#64298,#64299,#64300,#64301,#64302,#64303,#64304,#64305,
#64306,#64307),.UNSPECIFIED.,.F.,.F.,(4,3,3,3,3,3,3,3,3,3,3,3,3,4),(-92.0094590374927,
-91.5507764006196,-91.0532178332249,-90.5556592658303,-90.0581006984356,
-89.5605421310409,-89.0629835636462,-88.5654249962516,-88.0678664288569,
-87.5703078614622,-87.0727492940676,-86.5751907266729,-86.0776321592782,
-85.7262737303131),.UNSPECIFIED.);
#711=B_SPLINE_CURVE_WITH_KNOTS('',3,(#64308,#64309,#64310,#64311,#64312,
#64313,#64314,#64315,#64316,#64317,#64318,#64319,#64320,#64321,#64322,#64323,
#64324,#64325,#64326,#64327,#64328,#64329,#64330,#64331,#64332,#64333,#64334,
#64335,#64336,#64337,#64338,#64339,#64340,#64341,#64342,#64343,#64344,#64345,
#64346,#64347,#64348,#64349,#64350),.UNSPECIFIED.,.F.,.F.,(4,3,3,3,3,3,
3,3,3,3,3,3,3,3,4),(82.7914542042461,83.0922807549102,83.5898393223049,
84.0873978896996,84.5849564570942,85.0825150244889,85.5800735918836,86.0776321592782,
86.5751907266729,87.0727492940676,87.5703078614623,88.0678664288569,88.5654249962516,
89.0629835636463,89.0746395114257),.UNSPECIFIED.);
#712=B_SPLINE_CURVE_WITH_KNOTS('',3,(#64355,#64356,#64357,#64358,#64359,
#64360,#64361,#64362,#64363,#64364,#64365,#64366,#64367,#64368,#64369,#64370,
#64371,#64372,#64373,#64374,#64375,#64376,#64377,#64378,#64379,#64380,#64381,
#64382,#64383,#64384,#64385,#64386,#64387,#64388,#64389,#64390,#64391,#64392,
#64393,#64394,#64395,#64396,#64397),.UNSPECIFIED.,.F.,.F.,(4,3,3,3,3,3,
3,3,3,3,3,3,3,3,4),(-98.2926443446723,-98.0190377767503,-97.5214792093557,
-97.023920641961,-96.5263620745663,-96.0288035071717,-95.531244939777,-95.0336863723823,
-94.5361278049876,-94.038569237593,-93.5410106701983,-93.0434521028036,
-92.5458935354089,-92.0483349680143,-92.0094590374927),.UNSPECIFIED.);
#713=B_SPLINE_CURVE_WITH_KNOTS('',3,(#64398,#64399,#64400,#64401,#64402,
#64403,#64404,#64405,#64406,#64407,#64408,#64409,#64410,#64411,#64412,#64413,
#64414,#64415,#64416,#64417,#64418,#64419,#64420,#64421,#64422,#64423,#64424,
#64425,#64426,#64427,#64428,#64429,#64430,#64431,#64432,#64433,#64434,#64435,
#64436,#64437),.UNSPECIFIED.,.F.,.F.,(4,3,3,3,3,3,3,3,3,3,3,3,3,4),(89.0746395114257,
89.5605421310409,90.0581006984356,90.5556592658303,91.0532178332249,91.5507764006196,
92.0483349680143,92.545893535409,93.0434521028036,93.5410106701983,94.038569237593,
94.5361278049877,95.0336863723823,95.3578248186053),.UNSPECIFIED.);
#714=B_SPLINE_CURVE_WITH_KNOTS('',3,(#64442,#64443,#64444,#64445,#64446,
#64447,#64448,#64449,#64450,#64451,#64452,#64453,#64454,#64455,#64456,#64457,
#64458,#64459,#64460,#64461,#64462,#64463,#64464,#64465,#64466,#64467,#64468,
#64469,#64470,#64471,#64472,#64473,#64474,#64475,#64476,#64477,#64478,#64479,
#64480,#64481,#64482,#64483,#64484),.UNSPECIFIED.,.F.,.F.,(4,3,3,3,3,3,
3,3,3,3,3,3,3,3,4),(-104.575829651852,-104.487299152881,-103.989740585486,
-103.492182018092,-102.994623450697,-102.497064883302,-101.999506315908,
-101.501947748513,-101.004389181118,-100.506830613724,-100.009272046329,
-99.5117134789344,-99.0141549115397,-98.516596344145,-98.2926443446723),
 .UNSPECIFIED.);
#715=B_SPLINE_CURVE_WITH_KNOTS('',3,(#64485,#64486,#64487,#64488,#64489,
#64490,#64491,#64492,#64493,#64494,#64495,#64496,#64497,#64498,#64499,#64500,
#64501,#64502,#64503,#64504,#64505,#64506,#64507,#64508,#64509,#64510,#64511,
#64512,#64513,#64514,#64515,#64516,#64517,#64518,#64519,#64520,#64521,#64522,
#64523,#64524,#64525,#64526,#64527),.UNSPECIFIED.,.F.,.F.,(4,3,3,3,3,3,
3,3,3,3,3,3,3,3,4),(95.3578248186053,95.531244939777,96.0288035071717,96.5263620745663,
97.023920641961,97.5214792093557,98.0190377767504,98.516596344145,99.0141549115397,
99.5117134789344,100.009272046329,100.506830613724,101.004389181118,101.501947748513,
101.641010125785),.UNSPECIFIED.);
#716=B_SPLINE_CURVE_WITH_KNOTS('',3,(#64532,#64533,#64534,#64535,#64536,
#64537,#64538,#64539,#64540,#64541,#64542,#64543,#64544,#64545,#64546,#64547,
#64548,#64549,#64550,#64551,#64552,#64553,#64554,#64555,#64556,#64557,#64558,
#64559,#64560,#64561,#64562,#64563,#64564,#64565,#64566,#64567,#64568,#64569,
#64570,#64571),.UNSPECIFIED.,.F.,.F.,(4,3,3,3,3,3,3,3,3,3,3,3,3,4),(-110.859014959031,
-110.458001961617,-109.960443394222,-109.462884826828,-108.965326259433,
-108.467767692038,-107.970209124644,-107.472650557249,-106.975091989854,
-106.47753342246,-105.979974855065,-105.48241628767,-104.984857720276,-104.575829651852),
 .UNSPECIFIED.);
#717=B_SPLINE_CURVE_WITH_KNOTS('',3,(#64572,#64573,#64574,#64575,#64576,
#64577,#64578,#64579,#64580,#64581,#64582,#64583,#64584,#64585,#64586,#64587,
#64588,#64589,#64590,#64591,#64592,#64593,#64594,#64595,#64596,#64597,#64598,
#64599,#64600,#64601,#64602,#64603,#64604,#64605,#64606,#64607,#64608,#64609,
#64610,#64611),.UNSPECIFIED.,.F.,.F.,(4,3,3,3,3,3,3,3,3,3,3,3,3,4),(101.641010125785,
101.999506315908,102.497064883302,102.994623450697,103.492182018092,103.989740585486,
104.487299152881,104.984857720276,105.48241628767,105.979974855065,106.47753342246,
106.975091989854,107.472650557249,107.924195432964),.UNSPECIFIED.);
#718=B_SPLINE_CURVE_WITH_KNOTS('',3,(#64616,#64617,#64618,#64619,#64620,
#64621,#64622,#64623,#64624,#64625,#64626,#64627,#64628,#64629,#64630,#64631,
#64632,#64633,#64634,#64635,#64636,#64637,#64638,#64639,#64640,#64641,#64642,
#64643,#64644,#64645,#64646,#64647,#64648,#64649,#64650,#64651,#64652,#64653,
#64654,#64655,#64656,#64657,#64658),.UNSPECIFIED.,.F.,.F.,(4,3,3,3,3,3,
3,3,3,3,3,3,3,3,4),(-117.142200266211,-116.926263337748,-116.428704770353,
-115.931146202959,-115.433587635564,-114.936029068169,-114.438470500775,
-113.94091193338,-113.443353365985,-112.94579479859,-112.448236231196,-111.950677663801,
-111.453119096406,-110.955560529012,-110.859014959031),.UNSPECIFIED.);
#719=B_SPLINE_CURVE_WITH_KNOTS('',3,(#64659,#64660,#64661,#64662,#64663,
#64664,#64665,#64666,#64667,#64668,#64669,#64670,#64671,#64672,#64673,#64674,
#64675,#64676,#64677,#64678,#64679,#64680,#64681,#64682,#64683,#64684,#64685,
#64686,#64687,#64688,#64689,#64690,#64691,#64692,#64693,#64694,#64695,#64696,
#64697,#64698,#64699,#64700,#64701),.UNSPECIFIED.,.F.,.F.,(4,3,3,3,3,3,
3,3,3,3,3,3,3,3,4),(107.924195432964,107.970209124644,108.467767692038,
108.965326259433,109.462884826828,109.960443394222,110.458001961617,110.955560529012,
111.453119096406,111.950677663801,112.448236231196,112.945794798591,113.443353365985,
113.94091193338,114.207380740144),.UNSPECIFIED.);
#720=B_SPLINE_CURVE_WITH_KNOTS('',3,(#64706,#64707,#64708,#64709,#64710,
#64711,#64712,#64713,#64714,#64715,#64716,#64717,#64718,#64719,#64720,#64721,
#64722,#64723,#64724,#64725,#64726,#64727,#64728,#64729,#64730,#64731,#64732,
#64733,#64734,#64735,#64736,#64737,#64738,#64739,#64740,#64741,#64742,#64743,
#64744,#64745,#64746,#64747,#64748),.UNSPECIFIED.,.F.,.F.,(4,3,3,3,3,3,
3,3,3,3,3,3,3,3,4),(-123.425385573391,-123.394524713879,-122.896966146484,
-122.399407579089,-121.901849011695,-121.4042904443,-120.906731876905,-120.409173309511,
-119.911614742116,-119.414056174721,-118.916497607327,-118.418939039932,
-117.921380472537,-117.423821905143,-117.142200266211),.UNSPECIFIED.);
#721=B_SPLINE_CURVE_WITH_KNOTS('',3,(#64749,#64750,#64751,#64752,#64753,
#64754,#64755,#64756,#64757,#64758,#64759,#64760,#64761,#64762,#64763,#64764,
#64765,#64766,#64767,#64768,#64769,#64770,#64771,#64772,#64773,#64774,#64775,
#64776,#64777,#64778,#64779,#64780,#64781,#64782,#64783,#64784,#64785,#64786,
#64787,#64788,#64789,#64790,#64791),.UNSPECIFIED.,.F.,.F.,(4,3,3,3,3,3,
3,3,3,3,3,3,3,3,4),(114.207380740144,114.438470500775,114.936029068169,
115.433587635564,115.931146202959,116.428704770353,116.926263337748,117.423821905143,
117.921380472537,118.418939039932,118.916497607327,119.414056174721,119.911614742116,
120.409173309511,120.490566047324),.UNSPECIFIED.);
#722=B_SPLINE_CURVE_WITH_KNOTS('',3,(#64796,#64797,#64798,#64799,#64800,
#64801,#64802,#64803,#64804,#64805,#64806,#64807,#64808,#64809,#64810,#64811,
#64812,#64813,#64814,#64815,#64816,#64817,#64818,#64819,#64820,#64821,#64822,
#64823,#64824,#64825,#64826,#64827,#64828,#64829,#64830,#64831,#64832,#64833,
#64834,#64835),.UNSPECIFIED.,.F.,.F.,(4,3,3,3,3,3,3,3,3,3,3,3,3,4),(-129.70857088057,
-129.365227522615,-128.86766895522,-128.370110387825,-127.872551820431,
-127.374993253036,-126.877434685641,-126.379876118247,-125.882317550852,
-125.384758983457,-124.887200416063,-124.389641848668,-123.892083281273,
-123.425385573391),.UNSPECIFIED.);
#723=B_SPLINE_CURVE_WITH_KNOTS('',3,(#64836,#64837,#64838,#64839,#64840,
#64841,#64842,#64843,#64844,#64845,#64846,#64847,#64848,#64849,#64850,#64851,
#64852,#64853,#64854,#64855,#64856,#64857,#64858,#64859,#64860,#64861,#64862,
#64863,#64864,#64865,#64866,#64867,#64868,#64869,#64870,#64871,#64872,#64873,
#64874,#64875),.UNSPECIFIED.,.F.,.F.,(4,3,3,3,3,3,3,3,3,3,3,3,3,4),(120.490566047324,
120.906731876905,121.4042904443,121.901849011695,122.399407579089,122.896966146484,
123.394524713879,123.892083281273,124.389641848668,124.887200416063,125.384758983457,
125.882317550852,126.379876118247,126.773751354503),.UNSPECIFIED.);
#724=B_SPLINE_CURVE_WITH_KNOTS('',3,(#64880,#64881,#64882,#64883,#64884,
#64885,#64886,#64887,#64888,#64889,#64890,#64891,#64892,#64893,#64894,#64895,
#64896,#64897,#64898,#64899,#64900,#64901,#64902,#64903,#64904,#64905,#64906,
#64907,#64908,#64909,#64910,#64911,#64912,#64913,#64914,#64915,#64916,#64917,
#64918,#64919,#64920,#64921,#64922),.UNSPECIFIED.,.F.,.F.,(4,3,3,3,3,3,
3,3,3,3,3,3,3,3,4),(-135.99175618775,-135.833488898745,-135.335930331351,
-134.838371763956,-134.340813196561,-133.843254629167,-133.345696061772,
-132.848137494377,-132.350578926983,-131.853020359588,-131.355461792193,
-130.857903224799,-130.360344657404,-129.862786090009,-129.70857088057),
 .UNSPECIFIED.);
#725=B_SPLINE_CURVE_WITH_KNOTS('',3,(#64923,#64924,#64925,#64926,#64927,
#64928,#64929,#64930,#64931,#64932,#64933,#64934,#64935,#64936,#64937,#64938,
#64939,#64940,#64941,#64942,#64943,#64944,#64945,#64946,#64947,#64948,#64949,
#64950,#64951,#64952,#64953,#64954,#64955,#64956,#64957,#64958,#64959,#64960,
#64961,#64962,#64963,#64964,#64965),.UNSPECIFIED.,.F.,.F.,(4,3,3,3,3,3,
3,3,3,3,3,3,3,3,4),(126.773751354503,126.877434685641,127.374993253036,
127.872551820431,128.370110387825,128.86766895522,129.365227522615,129.862786090009,
130.360344657404,130.857903224799,131.355461792193,131.853020359588,132.350578926983,
132.848137494377,133.056936661683),.UNSPECIFIED.);
#726=B_SPLINE_CURVE_WITH_KNOTS('',3,(#64970,#64971,#64972,#64973,#64974,
#64975,#64976,#64977,#64978,#64979,#64980,#64981,#64982,#64983,#64984,#64985,
#64986,#64987,#64988,#64989,#64990,#64991,#64992,#64993,#64994,#64995,#64996,
#64997,#64998,#64999,#65000,#65001,#65002,#65003,#65004,#65005,#65006,#65007,
#65008,#65009),.UNSPECIFIED.,.F.,.F.,(4,3,3,3,3,3,3,3,3,3,3,3,3,4),(-142.274941494929,
-141.804191707481,-141.306633140087,-140.809074572692,-140.311516005297,
-139.813957437903,-139.316398870508,-138.818840303113,-138.321281735719,
-137.823723168324,-137.326164600929,-136.828606033535,-136.33104746614,
-135.99175618775),.UNSPECIFIED.);
#727=B_SPLINE_CURVE_WITH_KNOTS('',3,(#65010,#65011,#65012,#65013,#65014,
#65015,#65016,#65017,#65018,#65019,#65020,#65021,#65022,#65023,#65024,#65025,
#65026,#65027,#65028,#65029,#65030,#65031,#65032,#65033,#65034,#65035,#65036,
#65037,#65038,#65039,#65040,#65041,#65042,#65043,#65044,#65045,#65046,#65047,
#65048,#65049,#65050,#65051,#65052),.UNSPECIFIED.,.F.,.F.,(4,3,3,3,3,3,
3,3,3,3,3,3,3,3,4),(133.056936661683,133.345696061772,133.843254629167,
134.340813196561,134.838371763956,135.335930331351,135.833488898745,136.33104746614,
136.828606033535,137.326164600929,137.823723168324,138.321281735719,138.818840303113,
139.316398870508,139.340121968862),.UNSPECIFIED.);
#728=B_SPLINE_CURVE_WITH_KNOTS('',3,(#65057,#65058,#65059,#65060,#65061,
#65062,#65063,#65064,#65065,#65066,#65067,#65068,#65069,#65070,#65071,#65072,
#65073,#65074,#65075,#65076,#65077,#65078,#65079,#65080,#65081,#65082,#65083,
#65084,#65085,#65086,#65087,#65088,#65089,#65090,#65091,#65092,#65093,#65094,
#65095,#65096,#65097,#65098,#65099),.UNSPECIFIED.,.F.,.F.,(4,3,3,3,3,3,
3,3,3,3,3,3,3,3,4),(-148.558126802109,-148.272453083612,-147.774894516218,
-147.277335948823,-146.779777381428,-146.282218814033,-145.784660246639,
-145.287101679244,-144.789543111849,-144.291984544455,-143.79442597706,
-143.296867409665,-142.799308842271,-142.301750274876,-142.274941494929),
 .UNSPECIFIED.);
#729=B_SPLINE_CURVE_WITH_KNOTS('',3,(#65100,#65101,#65102,#65103,#65104,
#65105,#65106,#65107,#65108,#65109,#65110,#65111,#65112,#65113,#65114,#65115,
#65116,#65117,#65118,#65119,#65120,#65121,#65122,#65123,#65124,#65125,#65126,
#65127,#65128,#65129,#65130,#65131,#65132,#65133,#65134,#65135,#65136,#65137,
#65138,#65139),.UNSPECIFIED.,.F.,.F.,(4,3,3,3,3,3,3,3,3,3,3,3,3,4),(139.340121968862,
139.813957437903,140.311516005297,140.809074572692,141.306633140087,141.804191707481,
142.301750274876,142.799308842271,143.296867409665,143.79442597706,144.291984544455,
144.789543111849,145.287101679244,145.623307276042),.UNSPECIFIED.);
#730=B_SPLINE_CURVE_WITH_KNOTS('',3,(#65144,#65145,#65146,#65147,#65148,
#65149,#65150,#65151,#65152,#65153,#65154,#65155,#65156,#65157,#65158,#65159,
#65160,#65161,#65162,#65163,#65164,#65165,#65166,#65167,#65168,#65169,#65170,
#65171,#65172,#65173,#65174,#65175,#65176,#65177,#65178,#65179,#65180,#65181,
#65182,#65183,#65184,#65185,#65186),.UNSPECIFIED.,.F.,.F.,(4,3,3,3,3,3,
3,3,3,3,3,3,3,3,4),(-154.841312109289,-154.740714459743,-154.243155892348,
-153.745597324954,-153.248038757559,-152.750480190164,-152.25292162277,
-151.755363055375,-151.25780448798,-150.760245920586,-150.262687353191,
-149.765128785796,-149.267570218402,-148.770011651007,-148.558126802109),
 .UNSPECIFIED.);
#731=B_SPLINE_CURVE_WITH_KNOTS('',3,(#65187,#65188,#65189,#65190,#65191,
#65192,#65193,#65194,#65195,#65196,#65197,#65198,#65199,#65200,#65201,#65202,
#65203,#65204,#65205,#65206,#65207,#65208,#65209,#65210,#65211,#65212,#65213,
#65214,#65215,#65216,#65217,#65218,#65219,#65220,#65221,#65222,#65223,#65224,
#65225,#65226,#65227,#65228,#65229),.UNSPECIFIED.,.F.,.F.,(4,3,3,3,3,3,
3,3,3,3,3,3,3,3,4),(145.623307276042,145.784660246639,146.282218814034,
146.779777381428,147.277335948823,147.774894516218,148.272453083612,148.770011651007,
149.267570218402,149.765128785796,150.262687353191,150.760245920586,151.25780448798,
151.755363055375,151.906492583222),.UNSPECIFIED.);
#732=B_SPLINE_CURVE_WITH_KNOTS('',3,(#65234,#65235,#65236,#65237,#65238,
#65239,#65240,#65241,#65242,#65243,#65244,#65245,#65246,#65247,#65248,#65249,
#65250,#65251,#65252,#65253,#65254,#65255,#65256,#65257,#65258,#65259,#65260,
#65261,#65262,#65263,#65264,#65265,#65266,#65267,#65268,#65269,#65270,#65271,
#65272,#65273),.UNSPECIFIED.,.F.,.F.,(4,3,3,3,3,3,3,3,3,3,3,3,3,4),(-161.124497416468,
-160.711417268479,-160.213858701084,-159.71630013369,-159.218741566295,
-158.7211829989,-158.223624431506,-157.726065864111,-157.228507296716,-156.730948729322,
-156.233390161927,-155.735831594532,-155.238273027138,-154.841312109289),
 .UNSPECIFIED.);
#733=B_SPLINE_CURVE_WITH_KNOTS('',3,(#65274,#65275,#65276,#65277,#65278,
#65279,#65280,#65281,#65282,#65283,#65284,#65285,#65286,#65287,#65288,#65289,
#65290,#65291,#65292,#65293,#65294,#65295,#65296,#65297,#65298,#65299,#65300,
#65301,#65302,#65303,#65304,#65305,#65306,#65307,#65308,#65309,#65310,#65311,
#65312,#65313),.UNSPECIFIED.,.F.,.F.,(4,3,3,3,3,3,3,3,3,3,3,3,3,4),(151.906492583222,
152.25292162277,152.750480190164,153.248038757559,153.745597324954,154.243155892348,
154.740714459743,155.238273027138,155.735831594532,156.233390161927,156.730948729322,
157.228507296716,157.726065864111,158.189677890401),.UNSPECIFIED.);
#734=B_SPLINE_CURVE_WITH_KNOTS('',3,(#65318,#65319,#65320,#65321,#65322,
#65323,#65324,#65325,#65326,#65327,#65328,#65329,#65330,#65331,#65332,#65333,
#65334,#65335,#65336,#65337,#65338,#65339,#65340,#65341,#65342,#65343,#65344,
#65345,#65346,#65347,#65348,#65349,#65350,#65351,#65352,#65353,#65354,#65355,
#65356,#65357,#65358,#65359,#65360),.UNSPECIFIED.,.F.,.F.,(4,3,3,3,3,3,
3,3,3,3,3,3,3,3,4),(-167.407682723648,-167.17967864461,-166.682120077215,
-166.18456150982,-165.687002942426,-165.189444375031,-164.691885807636,
-164.194327240242,-163.696768672847,-163.199210105452,-162.701651538058,
-162.204092970663,-161.706534403268,-161.208975835874,-161.124497416468),
 .UNSPECIFIED.);
#735=B_SPLINE_CURVE_WITH_KNOTS('',3,(#65361,#65362,#65363,#65364,#65365,
#65366,#65367,#65368,#65369,#65370,#65371,#65372,#65373,#65374,#65375,#65376,
#65377,#65378,#65379,#65380,#65381,#65382,#65383,#65384,#65385,#65386,#65387,
#65388,#65389,#65390,#65391,#65392,#65393,#65394,#65395,#65396,#65397,#65398,
#65399,#65400,#65401,#65402,#65403),.UNSPECIFIED.,.F.,.F.,(4,3,3,3,3,3,
3,3,3,3,3,3,3,3,4),(158.189677890401,158.223624431506,158.7211829989,159.218741566295,
159.71630013369,160.213858701084,160.711417268479,161.208975835874,161.706534403268,
162.204092970663,162.701651538058,163.199210105452,163.696768672847,164.194327240242,
164.472863197581),.UNSPECIFIED.);
#736=B_SPLINE_CURVE_WITH_KNOTS('',3,(#65408,#65409,#65410,#65411,#65412,
#65413,#65414,#65415,#65416,#65417,#65418,#65419,#65420,#65421,#65422,#65423,
#65424,#65425,#65426,#65427,#65428,#65429,#65430,#65431,#65432,#65433,#65434,
#65435,#65436,#65437,#65438,#65439,#65440,#65441,#65442,#65443,#65444,#65445,
#65446,#65447,#65448,#65449,#65450),.UNSPECIFIED.,.F.,.F.,(4,3,3,3,3,3,
3,3,3,3,3,3,3,3,4),(-173.690868030827,-173.64794002074,-173.150381453346,
-172.652822885951,-172.155264318556,-171.657705751162,-171.160147183767,
-170.662588616372,-170.165030048978,-169.667471481583,-169.169912914188,
-168.672354346794,-168.174795779399,-167.677237212004,-167.407682723648),
 .UNSPECIFIED.);
#737=B_SPLINE_CURVE_WITH_KNOTS('',3,(#65451,#65452,#65453,#65454,#65455,
#65456,#65457,#65458,#65459,#65460,#65461,#65462,#65463,#65464,#65465,#65466,
#65467,#65468,#65469,#65470,#65471,#65472,#65473,#65474,#65475,#65476,#65477,
#65478,#65479,#65480,#65481,#65482,#65483,#65484,#65485,#65486,#65487,#65488,
#65489,#65490,#65491,#65492,#65493),.UNSPECIFIED.,.F.,.F.,(4,3,3,3,3,3,
3,3,3,3,3,3,3,3,4),(164.472863197581,164.691885807636,165.189444375031,
165.687002942426,166.18456150982,166.682120077215,167.17967864461,167.677237212004,
168.174795779399,168.672354346794,169.169912914188,169.667471481583,170.165030048978,
170.662588616372,170.75604850476),.UNSPECIFIED.);
#738=B_SPLINE_CURVE_WITH_KNOTS('',3,(#65498,#65499,#65500,#65501,#65502,
#65503,#65504,#65505,#65506,#65507,#65508,#65509,#65510,#65511,#65512,#65513,
#65514,#65515,#65516,#65517,#65518,#65519,#65520,#65521,#65522,#65523,#65524,
#65525,#65526,#65527,#65528,#65529,#65530,#65531,#65532,#65533,#65534,#65535,
#65536,#65537),.UNSPECIFIED.,.F.,.F.,(4,3,3,3,3,3,3,3,3,3,3,3,3,4),(-179.974053338007,
-179.618642829476,-179.121084262082,-178.623525694687,-178.125967127293,
-177.628408559898,-177.130849992503,-176.633291425108,-176.135732857714,
-175.638174290319,-175.140615722924,-174.64305715553,-174.145498588135,
-173.690868030827),.UNSPECIFIED.);
#739=B_SPLINE_CURVE_WITH_KNOTS('',3,(#65538,#65539,#65540,#65541,#65542,
#65543,#65544,#65545,#65546,#65547,#65548,#65549,#65550,#65551,#65552,#65553,
#65554,#65555,#65556,#65557,#65558,#65559,#65560,#65561,#65562,#65563,#65564,
#65565,#65566,#65567,#65568,#65569,#65570,#65571,#65572,#65573,#65574,#65575,
#65576,#65577),.UNSPECIFIED.,.F.,.F.,(4,3,3,3,3,3,3,3,3,3,3,3,3,4),(170.75604850476,
171.160147183767,171.657705751162,172.155264318556,172.652822885951,173.150381453346,
173.64794002074,174.145498588135,174.64305715553,175.140615722925,175.638174290319,
176.135732857714,176.633291425109,177.03923381194),.UNSPECIFIED.);
#740=B_SPLINE_CURVE_WITH_KNOTS('',3,(#65583,#65584,#65585,#65586),
 .UNSPECIFIED.,.F.,.F.,(4,4),(191.637151868977,191.75621690312),
 .UNSPECIFIED.);
#741=B_SPLINE_CURVE_WITH_KNOTS('',3,(#65592,#65593,#65594,#65595,#65596,
#65597,#65598,#65599,#65600,#65601,#65602,#65603,#65604,#65605,#65606,#65607),
 .UNSPECIFIED.,.F.,.F.,(4,1,1,1,1,1,1,1,1,1,1,1,1,4),(185.353966561798,
185.808597119106,186.3061556865,186.803714253895,187.30127282129,187.798831388684,
188.296389956079,188.793948523474,189.291507090868,189.789065658263,190.286624225658,
190.784182793052,191.281741360447,191.637151868977),.UNSPECIFIED.);
#742=B_SPLINE_CURVE_WITH_KNOTS('',3,(#65610,#65611,#65612,#65613,#65614,
#65615,#65616,#65617,#65618,#65619,#65620,#65621,#65622,#65623),
 .UNSPECIFIED.,.F.,.F.,(4,1,1,1,1,1,1,1,1,1,1,4),(185.353966561798,185.445582742361,
185.943141309756,186.440699877151,186.938258444545,187.43581701194,187.933375579335,
188.430934146729,188.928492714124,189.426051281519,189.923609848913,190.421168416308),
 .UNSPECIFIED.);
#743=B_SPLINE_CURVE_WITH_KNOTS('',3,(#65628,#65629,#65630,#65631,#65632,
#65633,#65634,#65635,#65636,#65637,#65638,#65639,#65640,#65641,#65642,#65643,
#65644),.UNSPECIFIED.,.F.,.F.,(4,1,1,1,1,1,1,1,1,1,1,1,1,1,4),(179.070781254618,
179.340335742975,179.83789431037,180.335452877764,180.833011445159,181.330570012554,
181.828128579948,182.325687147343,182.823245714738,183.320804282132,183.818362849527,
184.315921416922,184.813479984316,185.311038551711,185.353966561798),
 .UNSPECIFIED.);
#744=B_SPLINE_CURVE_WITH_KNOTS('',3,(#65645,#65646,#65647,#65648,#65649,
#65650,#65651,#65652,#65653,#65654,#65655,#65656,#65657,#65658,#65659,#65660),
 .UNSPECIFIED.,.F.,.F.,(4,1,1,1,1,1,1,1,1,1,1,1,1,4),(179.070781254618,
179.474879933625,179.97243850102,180.469997068415,180.967555635809,181.465114203204,
181.962672770599,182.460231337993,182.957789905388,183.455348472783,183.952907040177,
184.450465607572,184.948024174967,185.353966561798),.UNSPECIFIED.);
#745=B_SPLINE_CURVE_WITH_KNOTS('',3,(#65665,#65666,#65667,#65668,#65669,
#65670,#65671,#65672,#65673,#65674,#65675,#65676,#65677,#65678,#65679,#65680,
#65681),.UNSPECIFIED.,.F.,.F.,(4,1,1,1,1,1,1,1,1,1,1,1,1,1,4),(172.787595947439,
172.872074366844,173.369632934239,173.867191501634,174.364750069028,174.862308636423,
175.359867203818,175.857425771212,176.354984338607,176.852542906002,177.350101473396,
177.847660040791,178.345218608186,178.84277717558,179.070781254618),
 .UNSPECIFIED.);
#746=B_SPLINE_CURVE_WITH_KNOTS('',3,(#65682,#65683,#65684,#65685,#65686,
#65687,#65688,#65689,#65690,#65691,#65692,#65693,#65694,#65695,#65696,#65697,
#65698),.UNSPECIFIED.,.F.,.F.,(4,1,1,1,1,1,1,1,1,1,1,1,1,1,4),(172.787595947439,
173.006618557495,173.504177124889,174.001735692284,174.499294259679,174.996852827073,
175.494411394468,175.991969961863,176.489528529257,176.987087096652,177.484645664047,
177.982204231441,178.479762798836,178.977321366231,179.070781254618),
 .UNSPECIFIED.);
#747=B_SPLINE_CURVE_WITH_KNOTS('',3,(#65703,#65704,#65705,#65706,#65707,
#65708,#65709,#65710,#65711,#65712,#65713,#65714,#65715,#65716,#65717,#65718),
 .UNSPECIFIED.,.F.,.F.,(4,1,1,1,1,1,1,1,1,1,1,1,1,4),(166.504410640259,
166.901371558108,167.398930125503,167.896488692898,168.394047260292,168.891605827687,
169.389164395082,169.886722962476,170.384281529871,170.881840097266,171.37939866466,
171.876957232055,172.37451579945,172.787595947439),.UNSPECIFIED.);
#748=B_SPLINE_CURVE_WITH_KNOTS('',3,(#65719,#65720,#65721,#65722,#65723,
#65724,#65725,#65726,#65727,#65728,#65729,#65730,#65731,#65732,#65733,#65734,
#65735),.UNSPECIFIED.,.F.,.F.,(4,1,1,1,1,1,1,1,1,1,1,1,1,1,4),(166.504410640259,
166.538357181364,167.035915748758,167.533474316153,168.031032883548,168.528591450942,
169.026150018337,169.523708585732,170.021267153126,170.518825720521,171.016384287916,
171.51394285531,172.011501422705,172.5090599901,172.787595947439),
 .UNSPECIFIED.);
#749=B_SPLINE_CURVE_WITH_KNOTS('',3,(#65740,#65741,#65742,#65743,#65744,
#65745,#65746,#65747,#65748,#65749,#65750,#65751,#65752,#65753,#65754,#65755,
#65756),.UNSPECIFIED.,.F.,.F.,(4,1,1,1,1,1,1,1,1,1,1,1,1,1,4),(160.22122533308,
160.433110181977,160.930668749372,161.428227316767,161.925785884161,162.423344451556,
162.920903018951,163.418461586346,163.91602015374,164.413578721135,164.91113728853,
165.408695855924,165.906254423319,166.403812990714,166.504410640259),
 .UNSPECIFIED.);
#750=B_SPLINE_CURVE_WITH_KNOTS('',3,(#65757,#65758,#65759,#65760,#65761,
#65762,#65763,#65764,#65765,#65766,#65767,#65768,#65769,#65770,#65771,#65772),
 .UNSPECIFIED.,.F.,.F.,(4,1,1,1,1,1,1,1,1,1,1,1,1,4),(160.22122533308,160.567654372628,
161.065212940022,161.562771507417,162.060330074812,162.557888642206,163.055447209601,
163.553005776996,164.05056434439,164.548122911785,165.04568147918,165.543240046574,
166.040798613969,166.504410640259),.UNSPECIFIED.);
#751=B_SPLINE_CURVE_WITH_KNOTS('',3,(#65777,#65778,#65779,#65780,#65781,
#65782,#65783,#65784,#65785,#65786,#65787,#65788,#65789,#65790,#65791,#65792,
#65793),.UNSPECIFIED.,.F.,.F.,(4,1,1,1,1,1,1,1,1,1,1,1,1,1,4),(153.9380400259,
153.964848805847,154.462407373241,154.959965940636,155.457524508031,155.955083075425,
156.45264164282,156.950200210215,157.447758777609,157.945317345004,158.442875912399,
158.940434479793,159.437993047188,159.935551614583,160.22122533308),
 .UNSPECIFIED.);
#752=B_SPLINE_CURVE_WITH_KNOTS('',3,(#65794,#65795,#65796,#65797,#65798,
#65799,#65800,#65801,#65802,#65803,#65804,#65805,#65806,#65807,#65808,#65809,
#65810),.UNSPECIFIED.,.F.,.F.,(4,1,1,1,1,1,1,1,1,1,1,1,1,1,4),(153.9380400259,
154.099392996497,154.596951563892,155.094510131286,155.592068698681,156.089627266076,
156.58718583347,157.084744400865,157.58230296826,158.079861535654,158.577420103049,
159.074978670444,159.572537237838,160.070095805233,160.22122533308),
 .UNSPECIFIED.);
#753=B_SPLINE_CURVE_WITH_KNOTS('',3,(#65815,#65816,#65817,#65818,#65819,
#65820,#65821,#65822,#65823,#65824,#65825,#65826,#65827,#65828,#65829,#65830),
 .UNSPECIFIED.,.F.,.F.,(4,1,1,1,1,1,1,1,1,1,1,1,1,4),(147.65485471872,147.994145997111,
148.491704564505,148.9892631319,149.486821699295,149.984380266689,150.481938834084,
150.979497401479,151.477055968873,151.974614536268,152.472173103663,152.969731671057,
153.467290238452,153.9380400259),.UNSPECIFIED.);
#754=B_SPLINE_CURVE_WITH_KNOTS('',3,(#65831,#65832,#65833,#65834,#65835,
#65836,#65837,#65838,#65839,#65840,#65841,#65842,#65843,#65844,#65845,#65846),
 .UNSPECIFIED.,.F.,.F.,(4,1,1,1,1,1,1,1,1,1,1,1,1,4),(147.65485471872,148.128690187761,
148.626248755156,149.12380732255,149.621365889945,150.11892445734,150.616483024734,
151.114041592129,151.611600159524,152.109158726918,152.606717294313,153.104275861708,
153.601834429102,153.9380400259),.UNSPECIFIED.);
#755=B_SPLINE_CURVE_WITH_KNOTS('',3,(#65851,#65852,#65853,#65854,#65855,
#65856,#65857,#65858,#65859,#65860,#65861,#65862,#65863,#65864,#65865,#65866,
#65867),.UNSPECIFIED.,.F.,.F.,(4,1,1,1,1,1,1,1,1,1,1,1,1,1,4),(141.371669411541,
141.52588462098,142.023443188375,142.521001755769,143.018560323164,143.516118890559,
144.013677457953,144.511236025348,145.008794592743,145.506353160137,146.003911727532,
146.501470294927,146.999028862321,147.496587429716,147.65485471872),
 .UNSPECIFIED.);
#756=B_SPLINE_CURVE_WITH_KNOTS('',3,(#65868,#65869,#65870,#65871,#65872,
#65873,#65874,#65875,#65876,#65877,#65878,#65879,#65880,#65881,#65882,#65883,
#65884),.UNSPECIFIED.,.F.,.F.,(4,1,1,1,1,1,1,1,1,1,1,1,1,1,4),(141.371669411541,
141.66042881163,142.157987379025,142.65554594642,143.153104513814,143.650663081209,
144.148221648604,144.645780215998,145.143338783393,145.640897350788,146.138455918182,
146.636014485577,147.133573052972,147.631131620366,147.65485471872),
 .UNSPECIFIED.);
#757=B_SPLINE_CURVE_WITH_KNOTS('',3,(#65889,#65890,#65891,#65892,#65893,
#65894,#65895,#65896,#65897,#65898,#65899,#65900,#65901,#65902,#65903,#65904),
 .UNSPECIFIED.,.F.,.F.,(4,1,1,1,1,1,1,1,1,1,1,1,1,4),(135.088484104361,
135.555181812244,136.052740379639,136.550298947033,137.047857514428,137.545416081823,
138.042974649217,138.540533216612,139.038091784007,139.535650351401,140.033208918796,
140.530767486191,141.028326053585,141.371669411541),.UNSPECIFIED.);
#758=B_SPLINE_CURVE_WITH_KNOTS('',3,(#65905,#65906,#65907,#65908,#65909,
#65910,#65911,#65912,#65913,#65914,#65915,#65916,#65917,#65918,#65919,#65920,
#65921),.UNSPECIFIED.,.F.,.F.,(4,1,1,1,1,1,1,1,1,1,1,1,1,1,4),(135.088484104361,
135.192167435499,135.689726002894,136.187284570289,136.684843137683,137.182401705078,
137.679960272473,138.177518839867,138.675077407262,139.172635974657,139.670194542051,
140.167753109446,140.665311676841,141.162870244235,141.371669411541),
 .UNSPECIFIED.);
#759=B_SPLINE_CURVE_WITH_KNOTS('',3,(#65926,#65927,#65928,#65929,#65930,
#65931,#65932,#65933,#65934,#65935,#65936,#65937,#65938,#65939,#65940,#65941,
#65942),.UNSPECIFIED.,.F.,.F.,(4,1,1,1,1,1,1,1,1,1,1,1,1,1,4),(128.805298797182,
129.086920436113,129.584479003508,130.082037570902,130.579596138297,131.077154705692,
131.574713273087,132.072271840481,132.569830407876,133.067388975271,133.564947542665,
134.06250611006,134.560064677455,135.057623244849,135.088484104361),
 .UNSPECIFIED.);
#760=B_SPLINE_CURVE_WITH_KNOTS('',3,(#65943,#65944,#65945,#65946,#65947,
#65948,#65949,#65950,#65951,#65952,#65953,#65954,#65955,#65956,#65957,#65958),
 .UNSPECIFIED.,.F.,.F.,(4,1,1,1,1,1,1,1,1,1,1,1,1,4),(128.805298797182,
129.221464626763,129.719023194158,130.216581761553,130.714140328947,131.211698896342,
131.709257463737,132.206816031131,132.704374598526,133.201933165921,133.699491733315,
134.19705030071,134.694608868105,135.088484104361),.UNSPECIFIED.);
#761=B_SPLINE_CURVE_WITH_KNOTS('',3,(#65963,#65964,#65965,#65966,#65967,
#65968,#65969,#65970,#65971,#65972,#65973,#65974,#65975,#65976,#65977,#65978,
#65979),.UNSPECIFIED.,.F.,.F.,(4,1,1,1,1,1,1,1,1,1,1,1,1,1,4),(122.522113490002,
122.618659059982,123.116217627377,123.613776194772,124.111334762166,124.608893329561,
125.106451896956,125.60401046435,126.101569031745,126.59912759914,127.096686166534,
127.594244733929,128.091803301324,128.589361868718,128.805298797182),
 .UNSPECIFIED.);
#762=B_SPLINE_CURVE_WITH_KNOTS('',3,(#65980,#65981,#65982,#65983,#65984,
#65985,#65986,#65987,#65988,#65989,#65990,#65991,#65992,#65993,#65994,#65995,
#65996),.UNSPECIFIED.,.F.,.F.,(4,1,1,1,1,1,1,1,1,1,1,1,1,1,4),(122.522113490002,
122.753203250633,123.250761818027,123.748320385422,124.245878952817,124.743437520211,
125.240996087606,125.738554655001,126.236113222395,126.73367178979,127.231230357185,
127.728788924579,128.226347491974,128.723906059369,128.805298797182),
 .UNSPECIFIED.);
#763=B_SPLINE_CURVE_WITH_KNOTS('',3,(#66001,#66002,#66003,#66004,#66005,
#66006,#66007,#66008,#66009,#66010,#66011,#66012,#66013,#66014,#66015,#66016),
 .UNSPECIFIED.,.F.,.F.,(4,1,1,1,1,1,1,1,1,1,1,1,1,4),(116.238928182823,
116.647956251246,117.145514818641,117.643073386036,118.14063195343,118.638190520825,
119.13574908822,119.633307655614,120.130866223009,120.628424790404,121.125983357798,
121.623541925193,122.121100492588,122.522113490002),.UNSPECIFIED.);
#764=B_SPLINE_CURVE_WITH_KNOTS('',3,(#66017,#66018,#66019,#66020,#66021,
#66022,#66023,#66024,#66025,#66026,#66027,#66028,#66029,#66030,#66031,#66032,
#66033),.UNSPECIFIED.,.F.,.F.,(4,1,1,1,1,1,1,1,1,1,1,1,1,1,4),(116.238928182823,
116.284941874502,116.782500441897,117.280059009291,117.777617576686,118.275176144081,
118.772734711475,119.27029327887,119.767851846265,120.265410413659,120.762968981054,
121.260527548449,121.758086115843,122.255644683238,122.522113490002),
 .UNSPECIFIED.);
#765=B_SPLINE_CURVE_WITH_KNOTS('',3,(#66038,#66039,#66040,#66041,#66042,
#66043,#66044,#66045,#66046,#66047,#66048,#66049,#66050,#66051,#66052,#66053,
#66054),.UNSPECIFIED.,.F.,.F.,(4,1,1,1,1,1,1,1,1,1,1,1,1,1,4),(109.955742875643,
110.179694875116,110.67725344251,111.174812009905,111.6723705773,112.169929144694,
112.667487712089,113.165046279484,113.662604846878,114.160163414273,114.657721981668,
115.155280549062,115.652839116457,116.150397683852,116.238928182823),
 .UNSPECIFIED.);
#766=B_SPLINE_CURVE_WITH_KNOTS('',3,(#66055,#66056,#66057,#66058,#66059,
#66060,#66061,#66062,#66063,#66064,#66065,#66066,#66067,#66068,#66069,#66070),
 .UNSPECIFIED.,.F.,.F.,(4,1,1,1,1,1,1,1,1,1,1,1,1,4),(109.955742875643,
110.314239065766,110.811797633161,111.309356200555,111.80691476795,112.304473335345,
112.802031902739,113.299590470134,113.797149037529,114.294707604923,114.792266172318,
115.289824739713,115.787383307107,116.238928182823),.UNSPECIFIED.);
#767=B_SPLINE_CURVE_WITH_KNOTS('',3,(#66075,#66076,#66077,#66078,#66079,
#66080,#66081,#66082,#66083,#66084,#66085,#66086,#66087,#66088,#66089,#66090,
#66091),.UNSPECIFIED.,.F.,.F.,(4,1,1,1,1,1,1,1,1,1,1,1,1,1,4),(103.672557568463,
103.711433498985,104.20899206638,104.706550633774,105.204109201169,105.701667768564,
106.199226335958,106.696784903353,107.194343470748,107.691902038142,108.189460605537,
108.687019172932,109.184577740326,109.682136307721,109.955742875643),
 .UNSPECIFIED.);
#768=B_SPLINE_CURVE_WITH_KNOTS('',3,(#66092,#66093,#66094,#66095,#66096,
#66097,#66098,#66099,#66100,#66101,#66102,#66103,#66104,#66105,#66106,#66107,
#66108),.UNSPECIFIED.,.F.,.F.,(4,1,1,1,1,1,1,1,1,1,1,1,1,1,4),(103.672557568463,
103.845977689635,104.34353625703,104.841094824424,105.338653391819,105.836211959214,
106.333770526608,106.831329094003,107.328887661398,107.826446228792,108.324004796187,
108.821563363582,109.319121930977,109.816680498371,109.955742875643),
 .UNSPECIFIED.);
#769=B_SPLINE_CURVE_WITH_KNOTS('',3,(#66113,#66114,#66115,#66116,#66117,
#66118,#66119,#66120,#66121,#66122,#66123,#66124,#66125,#66126,#66127,#66128),
 .UNSPECIFIED.,.F.,.F.,(4,1,1,1,1,1,1,1,1,1,1,1,1,4),(97.3893722612838,
97.7407306902488,98.2382892576435,98.7358478250382,99.2334063924328,99.7309649598275,
100.228523527222,100.726082094617,101.223640662012,101.721199229406,102.218757796801,
102.716316364196,103.21387493159,103.672557568463),.UNSPECIFIED.);
#770=B_SPLINE_CURVE_WITH_KNOTS('',3,(#66129,#66130,#66131,#66132,#66133,
#66134,#66135,#66136,#66137,#66138,#66139,#66140,#66141,#66142,#66143,#66144),
 .UNSPECIFIED.,.F.,.F.,(4,1,1,1,1,1,1,1,1,1,1,1,1,4),(97.3893722612838,
97.875274880899,98.3728334482937,98.8703920156884,99.3679505830831,99.8655091504777,
100.363067717872,100.860626285267,101.358184852662,101.855743420056,102.353301987451,
102.850860554846,103.34841912224,103.672557568463),.UNSPECIFIED.);
#771=B_SPLINE_CURVE_WITH_KNOTS('',3,(#66149,#66150,#66151,#66152,#66153,
#66154,#66155,#66156,#66157,#66158,#66159,#66160,#66161,#66162,#66163,#66164,
#66165),.UNSPECIFIED.,.F.,.F.,(4,1,1,1,1,1,1,1,1,1,1,1,1,1,4),(91.1061869541042,
91.2724693141181,91.7700278815128,92.2675864489074,92.7651450163021,93.2627035836968,
93.7602621510915,94.2578207184861,94.7553792858808,95.2529378532755,95.7504964206701,
96.2480549880648,96.7456135554595,97.2431721228542,97.3893722612838),
 .UNSPECIFIED.);
#772=B_SPLINE_CURVE_WITH_KNOTS('',3,(#66166,#66167,#66168,#66169,#66170,
#66171,#66172,#66173,#66174,#66175,#66176,#66177,#66178,#66179,#66180,#66181,
#66182),.UNSPECIFIED.,.F.,.F.,(4,1,1,1,1,1,1,1,1,1,1,1,1,1,4),(91.1061869541041,
91.4070135047683,91.904572072163,92.4021306395577,92.8996892069523,93.397247774347,
93.8948063417417,94.3923649091363,94.889923476531,95.3874820439257,95.8850406113204,
96.382599178715,96.8801577461097,97.3777163135044,97.3893722612838),
 .UNSPECIFIED.);
#773=B_SPLINE_CURVE_WITH_KNOTS('',3,(#66187,#66188,#66189,#66190,#66191,
#66192,#66193,#66194,#66195,#66196,#66197,#66198,#66199,#66200,#66201,#66202),
 .UNSPECIFIED.,.F.,.F.,(4,1,1,1,1,1,1,1,1,1,1,1,1,4),(84.8230016469246,
85.301766505382,85.7993250727767,86.2968836401714,86.794442207566,87.2920007749607,
87.7895593423554,88.2871179097501,88.7846764771447,89.2822350445394,89.7797936119341,
90.2773521793287,90.7749107467234,91.1061869541042),.UNSPECIFIED.);
#774=B_SPLINE_CURVE_WITH_KNOTS('',3,(#66203,#66204,#66205,#66206,#66207,
#66208,#66209,#66210,#66211,#66212,#66213,#66214,#66215,#66216,#66217,#66218,
#66219),.UNSPECIFIED.,.F.,.F.,(4,1,1,1,1,1,1,1,1,1,1,1,1,1,4),(84.8230016469245,
84.9387521286376,85.4363106960323,85.9338692634269,86.4314278308216,86.9289863982163,
87.4265449656109,87.9241035330056,88.4216621004003,88.9192206677949,89.4167792351896,
89.9143378025843,90.411896369979,90.9094549373736,91.1061869541041),
 .UNSPECIFIED.);
#775=B_SPLINE_CURVE_WITH_KNOTS('',3,(#66224,#66225,#66226,#66227,#66228,
#66229,#66230,#66231,#66232,#66233,#66234,#66235,#66236,#66237,#66238,#66239,
#66240),.UNSPECIFIED.,.F.,.F.,(4,1,1,1,1,1,1,1,1,1,1,1,1,1,4),(78.539816339745,
78.8335051292513,79.331063696646,79.8286222640406,80.3261808314353,80.82373939883,
81.3212979662247,81.8188565336193,82.316415101014,82.8139736684087,83.3115322358033,
83.809090803198,84.3066493705927,84.8042079379874,84.8230016469246),
 .UNSPECIFIED.);
#776=B_SPLINE_CURVE_WITH_KNOTS('',3,(#66241,#66242,#66243,#66244,#66245,
#66246,#66247,#66248,#66249,#66250,#66251,#66252,#66253,#66254,#66255,#66256),
 .UNSPECIFIED.,.F.,.F.,(4,1,1,1,1,1,1,1,1,1,1,1,1,4),(78.539816339745,78.9680493199015,
79.4656078872962,79.9631664546908,80.4607250220855,80.9582835894802,81.4558421568749,
81.9534007242695,82.4509592916642,82.9485178590589,83.4460764264536,83.9436349938482,
84.4411935612429,84.8230016469245),.UNSPECIFIED.);
#777=B_SPLINE_CURVE_WITH_KNOTS('',3,(#66261,#66262,#66263,#66264,#66265,
#66266,#66267,#66268,#66269,#66270,#66271,#66272,#66273,#66274,#66275,#66276,
#66277),.UNSPECIFIED.,.F.,.F.,(4,1,1,1,1,1,1,1,1,1,1,1,1,1,4),(72.2566310325654,
72.3652437531206,72.8628023205152,73.3603608879099,73.8579194553046,74.3554780226992,
74.8530365900939,75.3505951574886,75.8481537248833,76.3457122922779,76.8432708596726,
77.3408294270673,77.838387994462,78.3359465618566,78.539816339745),
 .UNSPECIFIED.);
#778=B_SPLINE_CURVE_WITH_KNOTS('',3,(#66278,#66279,#66280,#66281,#66282,
#66283,#66284,#66285,#66286,#66287,#66288,#66289,#66290,#66291,#66292,#66293,
#66294),.UNSPECIFIED.,.F.,.F.,(4,1,1,1,1,1,1,1,1,1,1,1,1,1,4),(72.2566310325654,
72.4997879437708,72.9973465111654,73.4949050785601,73.9924636459548,74.4900222133495,
74.9875807807441,75.4851393481388,75.9826979155335,76.4802564829282,76.9778150503228,
77.4753736177175,77.9729321851122,78.4704907525068,78.539816339745),
 .UNSPECIFIED.);
#779=B_SPLINE_CURVE_WITH_KNOTS('',3,(#66299,#66300,#66301,#66302,#66303,
#66304,#66305,#66306,#66307,#66308,#66309,#66310,#66311,#66312,#66313,#66314),
 .UNSPECIFIED.,.F.,.F.,(4,1,1,1,1,1,1,1,1,1,1,1,1,4),(65.9734457253858,
66.3945409443845,66.8920995117792,67.3896580791738,67.8872166465685,68.3847752139632,
68.8823337813579,69.3798923487525,69.8774509161472,70.3750094835419,70.8725680509366,
71.3701266183312,71.8676851857259,72.2566310325654),.UNSPECIFIED.);
#780=B_SPLINE_CURVE_WITH_KNOTS('',3,(#66315,#66316,#66317,#66318,#66319,
#66320,#66321,#66322,#66323,#66324,#66325,#66326,#66327,#66328,#66329,#66330,
#66331),.UNSPECIFIED.,.F.,.F.,(4,1,1,1,1,1,1,1,1,1,1,1,1,1,4),(65.9734457253858,
66.03152656764,66.5290851350347,67.0266437024294,67.5242022698241,68.0217608372187,
68.5193194046134,69.0168779720081,69.5144365394028,70.0119951067974,70.5095536741921,
71.0071122415868,71.5046708089814,72.0022293763761,72.2566310325654),
 .UNSPECIFIED.);
#781=B_SPLINE_CURVE_WITH_KNOTS('',3,(#66336,#66337,#66338,#66339,#66340,
#66341,#66342,#66343,#66344,#66345,#66346,#66347,#66348,#66349,#66350,#66351,
#66352),.UNSPECIFIED.,.F.,.F.,(4,1,1,1,1,1,1,1,1,1,1,1,1,1,4),(59.6902604182062,
59.9262795682538,60.4238381356484,60.9213967030431,61.4189552704378,61.9165138378325,
62.4140724052271,62.9116309726218,63.4091895400165,63.9067481074111,64.4043066748058,
64.9018652422005,65.3994238095952,65.8969823769898,65.9734457253858),
 .UNSPECIFIED.);
#782=B_SPLINE_CURVE_WITH_KNOTS('',3,(#66353,#66354,#66355,#66356,#66357,
#66358,#66359,#66360,#66361,#66362,#66363,#66364,#66365,#66366,#66367,#66368),
 .UNSPECIFIED.,.F.,.F.,(4,1,1,1,1,1,1,1,1,1,1,1,1,4),(59.6902604182062,
60.060823758904,60.5583823262987,61.0559408936933,61.553499461088,62.0510580284827,
62.5486165958773,63.046175163272,63.5437337306667,64.0412922980614,64.538850865456,
65.0364094328507,65.5339680002454,65.9734457253858),.UNSPECIFIED.);
#783=B_SPLINE_CURVE_WITH_KNOTS('',3,(#66373,#66374,#66375,#66376,#66377,
#66378,#66379,#66380,#66381,#66382,#66383,#66384,#66385,#66386,#66387,#66388,
#66389),.UNSPECIFIED.,.F.,.F.,(4,1,1,1,1,1,1,1,1,1,1,1,1,1,4),(53.4070751110266,
53.458018192123,53.9555767595177,54.4531353269124,54.9506938943071,55.4482524617017,
55.9458110290964,56.4433695964911,56.9409281638857,57.4384867312804,57.9360452986751,
58.4336038660698,58.9311624334644,59.4287210008591,59.6902604182062),
 .UNSPECIFIED.);
#784=B_SPLINE_CURVE_WITH_KNOTS('',3,(#66390,#66391,#66392,#66393,#66394,
#66395,#66396,#66397,#66398,#66399,#66400,#66401,#66402,#66403,#66404,#66405,
#66406),.UNSPECIFIED.,.F.,.F.,(4,1,1,1,1,1,1,1,1,1,1,1,1,1,4),(53.4070751110266,
53.5925623827733,54.0901209501679,54.5876795175626,55.0852380849573,55.5827966523519,
56.0803552197466,56.5779137871413,57.075472354536,57.5730309219306,58.0705894893253,
58.56814805672,59.0657066241146,59.5632651915093,59.6902604182062),
 .UNSPECIFIED.);
#785=B_SPLINE_CURVE_WITH_KNOTS('',3,(#66411,#66412,#66413,#66414,#66415,
#66416,#66417,#66418,#66419,#66420,#66421,#66422,#66423,#66424,#66425,#66426),
 .UNSPECIFIED.,.F.,.F.,(4,1,1,1,1,1,1,1,1,1,1,1,1,4),(47.123889803847,47.487315383387,
47.9848739507816,48.4824325181763,48.979991085571,49.4775496529657,49.9751082203603,
50.472666787755,50.9702253551497,51.4677839225444,51.965342489939,52.4629010573337,
52.9604596247284,53.4070751110266),.UNSPECIFIED.);
#786=B_SPLINE_CURVE_WITH_KNOTS('',3,(#66427,#66428,#66429,#66430,#66431,
#66432,#66433,#66434,#66435,#66436,#66437,#66438,#66439,#66440,#66441,#66442,
#66443),.UNSPECIFIED.,.F.,.F.,(4,1,1,1,1,1,1,1,1,1,1,1,1,1,4),(47.123889803847,
47.1243010066425,47.6218595740372,48.1194181414319,48.6169767088265,49.1145352762212,
49.6120938436159,50.1096524110105,50.6072109784052,51.1047695457999,51.6023281131946,
52.0998866805892,52.5974452479839,53.0950038153786,53.4070751110266),
 .UNSPECIFIED.);
#787=B_SPLINE_CURVE_WITH_KNOTS('',3,(#66448,#66449,#66450,#66451,#66452,
#66453,#66454,#66455,#66456,#66457,#66458,#66459,#66460,#66461,#66462,#66463,
#66464),.UNSPECIFIED.,.F.,.F.,(4,1,1,1,1,1,1,1,1,1,1,1,1,1,4),(40.8407044966674,
41.0190540072562,41.5166125746509,42.0141711420456,42.5117297094403,43.0092882768349,
43.5068468442296,44.0044054116243,44.501963979019,44.9995225464136,45.4970811138083,
45.994639681203,46.4921982485976,46.9897568159923,47.123889803847),
 .UNSPECIFIED.);
#788=B_SPLINE_CURVE_WITH_KNOTS('',3,(#66465,#66466,#66467,#66468,#66469,
#66470,#66471,#66472,#66473,#66474,#66475,#66476,#66477,#66478,#66479,#66480),
 .UNSPECIFIED.,.F.,.F.,(4,1,1,1,1,1,1,1,1,1,1,1,1,4),(40.8407044966674,
41.1535981979065,41.6511567653011,42.1487153326958,42.6462739000905,43.1438324674851,
43.6413910348798,44.1389496022745,44.6365081696692,45.1340667370638,45.6316253044585,
46.1291838718532,46.6267424392478,47.123889803847),.UNSPECIFIED.);
#789=B_SPLINE_CURVE_WITH_KNOTS('',3,(#66485,#66486,#66487,#66488,#66489,
#66490,#66491,#66492,#66493,#66494,#66495,#66496,#66497,#66498,#66499,#66500),
 .UNSPECIFIED.,.F.,.F.,(4,1,1,1,1,1,1,1,1,1,1,1,1,4),(34.5575191894878,
35.0483511985202,35.5459097659149,36.0434683333095,36.5410269007042,37.0385854680989,
37.5361440354935,38.0337026028882,38.5312611702829,39.0288197376776,39.5263783050722,
40.0239368724669,40.5214954398616,40.8407044966674),.UNSPECIFIED.);
#790=B_SPLINE_CURVE_WITH_KNOTS('',3,(#66501,#66502,#66503,#66504,#66505,
#66506,#66507,#66508,#66509,#66510,#66511,#66512,#66513,#66514,#66515,#66516,
#66517),.UNSPECIFIED.,.F.,.F.,(4,1,1,1,1,1,1,1,1,1,1,1,1,1,4),(34.5575191894878,
34.6853368217757,35.1828953891704,35.6804539565651,36.1780125239597,36.6755710913544,
37.1731296587491,37.6706882261438,38.1682467935384,38.6658053609331,39.1633639283278,
39.6609224957224,40.1584810631171,40.6560396305118,40.8407044966674),
 .UNSPECIFIED.);
#791=B_SPLINE_CURVE_WITH_KNOTS('',3,(#66522,#66523,#66524,#66525,#66526,
#66527,#66528,#66529,#66530,#66531,#66532,#66533,#66534,#66535,#66536,#66537,
#66538),.UNSPECIFIED.,.F.,.F.,(4,1,1,1,1,1,1,1,1,1,1,1,1,1,4),(28.2743338823083,
28.5800898223895,29.0776483897841,29.5752069571788,30.0727655245735,30.5703240919681,
31.0678826593628,31.5654412267575,32.0629997941522,32.5605583615468,33.0581169289415,
33.5556754963362,34.0532340637308,34.5507926311255,34.5575191894878),
 .UNSPECIFIED.);
#792=B_SPLINE_CURVE_WITH_KNOTS('',3,(#66539,#66540,#66541,#66542,#66543,
#66544,#66545,#66546,#66547,#66548,#66549,#66550,#66551,#66552,#66553,#66554),
 .UNSPECIFIED.,.F.,.F.,(4,1,1,1,1,1,1,1,1,1,1,1,1,4),(28.2743338823082,
28.7146340130397,29.2121925804343,29.709751147829,30.2073097152237,30.7048682826183,
31.202426850013,31.6999854174077,32.1975439848024,32.695102552197,33.1926611195917,
33.6902196869864,34.187778254381,34.5575191894878),.UNSPECIFIED.);
#793=B_SPLINE_CURVE_WITH_KNOTS('',3,(#66559,#66560,#66561,#66562,#66563,
#66564,#66565,#66566,#66567,#66568,#66569,#66570,#66571,#66572,#66573,#66574,
#66575),.UNSPECIFIED.,.F.,.F.,(4,1,1,1,1,1,1,1,1,1,1,1,1,1,4),(21.9911485751287,
22.1118284462587,22.6093870136534,23.1069455810481,23.6045041484427,24.1020627158374,
24.5996212832321,25.0971798506268,25.5947384180214,26.0922969854161,26.5898555528108,
27.0874141202054,27.5849726876001,28.0825312549948,28.2743338823083),
 .UNSPECIFIED.);
#794=B_SPLINE_CURVE_WITH_KNOTS('',3,(#66576,#66577,#66578,#66579,#66580,
#66581,#66582,#66583,#66584,#66585,#66586,#66587,#66588,#66589,#66590,#66591,
#66592),.UNSPECIFIED.,.F.,.F.,(4,1,1,1,1,1,1,1,1,1,1,1,1,1,4),(21.9911485751286,
22.2463726369089,22.7439312043036,23.2414897716983,23.7390483390929,24.2366069064876,
24.7341654738823,25.231724041277,25.7292826086716,26.2268411760663,26.724399743461,
27.2219583108556,27.7195168782503,28.217075445645,28.2743338823082),
 .UNSPECIFIED.);
#795=B_SPLINE_CURVE_WITH_KNOTS('',3,(#66597,#66598,#66599,#66600,#66601,
#66602,#66603,#66604,#66605,#66606,#66607,#66608,#66609,#66610,#66611,#66612),
 .UNSPECIFIED.,.F.,.F.,(4,1,1,1,1,1,1,1,1,1,1,1,1,4),(15.7079632679491,
16.1411256375227,16.6386842049173,17.136242772312,17.6338013397067,18.1313599071013,
18.628918474496,19.1264770418907,19.6240356092854,20.12159417668,20.6191527440747,
21.1167113114694,21.6142698788641,21.9911485751287),.UNSPECIFIED.);
#796=B_SPLINE_CURVE_WITH_KNOTS('',3,(#66613,#66614,#66615,#66616,#66617,
#66618,#66619,#66620,#66621,#66622,#66623,#66624,#66625,#66626,#66627,#66628,
#66629),.UNSPECIFIED.,.F.,.F.,(4,1,1,1,1,1,1,1,1,1,1,1,1,1,4),(15.707963267949,
15.7781112607782,16.2756698281729,16.7732283955675,17.2707869629622,17.7683455303569,
18.2659040977515,18.7634626651462,19.2610212325409,19.7585797999356,20.2561383673302,
20.7536969347249,21.2512555021196,21.7488140695142,21.9911485751286),
 .UNSPECIFIED.);
#797=B_SPLINE_CURVE_WITH_KNOTS('',3,(#66716,#66717,#66718,#66719,#66720,
#66721,#66722,#66723,#66724,#66725,#66726,#66727,#66728,#66729,#66730,#66731,
#66732,#66733,#66734,#66735,#66736,#66737,#66738,#66739,#66740,#66741,#66742,
#66743,#66744,#66745,#66746,#66747,#66748,#66749,#66750,#66751,#66752,#66753,
#66754,#66755,#66756,#66757,#66758,#66759,#66760,#66761,#66762,#66763,#66764,
#66765,#66766,#66767,#66768,#66769,#66770,#66771,#66772,#66773,#66774,#66775,
#66776,#66777,#66778,#66779,#66780,#66781,#66782,#66783,#66784,#66785,#66786,
#66787,#66788,#66789,#66790,#66791,#66792,#66793,#66794,#66795,#66796,#66797,
#66798,#66799,#66800,#66801,#66802,#66803,#66804,#66805,#66806,#66807,#66808,
#66809,#66810,#66811,#66812,#66813,#66814,#66815,#66816,#66817,#66818,#66819,
#66820,#66821,#66822,#66823,#66824),.UNSPECIFIED.,.F.,.F.,(4,3,3,3,3,3,
3,3,3,3,3,3,3,3,3,3,3,3,3,3,3,3,3,3,3,3,3,3,3,3,3,3,3,3,3,3,4),(-1.20073064134858,
-1.18778889510928,-1.1398809107738,-1.09143646705355,-1.07167907036071,
-1.06368126609984,-1.01465795392427,-0.965525826915534,-0.949331916808721,
-0.939879021382713,-0.9328302901472,-0.904080313500865,-0.855201229579345,
-0.805662558038644,-0.75704812329517,-0.720587297237565,-0.712370775609727,
-0.705760795802535,-0.65517935802383,-0.611204819064748,-0.560866233442363,
-0.510236856742273,-0.485178941357645,-0.478744674077057,-0.427679530002635,
-0.376207397355228,-0.324773909996537,-0.309773533665251,-0.271051841957094,
-0.254111101834776,-0.243588941900348,-0.237182702864077,-0.18584215881788,
-0.133559100291154,-0.0811710356345407,-0.0293189969567095,0.),
 .UNSPECIFIED.);
#798=B_SPLINE_CURVE_WITH_KNOTS('',3,(#66825,#66826,#66827,#66828,#66829,
#66830,#66831,#66832,#66833,#66834,#66835,#66836,#66837,#66838,#66839,#66840,
#66841,#66842,#66843,#66844,#66845,#66846,#66847,#66848,#66849,#66850,#66851,
#66852,#66853,#66854,#66855,#66856,#66857,#66858,#66859,#66860,#66861,#66862,
#66863,#66864,#66865,#66866,#66867,#66868,#66869,#66870,#66871,#66872,#66873,
#66874,#66875,#66876,#66877,#66878,#66879,#66880,#66881,#66882,#66883,#66884,
#66885,#66886,#66887,#66888,#66889,#66890,#66891,#66892,#66893,#66894,#66895,
#66896,#66897,#66898,#66899,#66900,#66901,#66902,#66903,#66904,#66905,#66906,
#66907,#66908,#66909,#66910,#66911,#66912,#66913,#66914,#66915,#66916,#66917,
#66918,#66919,#66920,#66921,#66922,#66923,#66924,#66925,#66926,#66927,#66928,
#66929,#66930,#66931,#66932,#66933,#66934,#66935,#66936),.UNSPECIFIED.,
 .F.,.F.,(4,3,3,3,3,3,3,3,3,3,3,3,3,3,3,3,3,3,3,3,3,3,3,3,3,3,3,3,3,3,3,
3,3,3,3,3,3,4),(-1.19772932745414,-1.18324084153904,-1.13092606054596,-1.07854075486302,
-1.06423152128911,-1.05378540339643,-1.0457165976122,-0.993876688902704,
-0.942396624118497,-0.92423148604273,-0.913627519080255,-0.906671232415686,
-0.875156121752095,-0.824147097148111,-0.772884353583531,-0.723395591317534,
-0.686279019618035,-0.677622815735757,-0.671424748299867,-0.621152038487914,
-0.57492930451954,-0.524525823920772,-0.474360645599062,-0.450422408151564,
-0.444347114400611,-0.394859071579653,-0.345423983708049,-0.29661796726323,
-0.283145695127838,-0.247752483236858,-0.232267953034554,-0.222024799734449,
-0.215891342040097,-0.167475083764442,-0.1188340990637,-0.0705281081382581,
-0.0231956473791646,0.),.UNSPECIFIED.);
#799=B_SPLINE_CURVE_WITH_KNOTS('',3,(#68413,#68414,#68415,#68416,#68417,
#68418,#68419,#68420,#68421,#68422,#68423,#68424,#68425,#68426,#68427,#68428,
#68429,#68430,#68431,#68432,#68433,#68434),.UNSPECIFIED.,.F.,.F.,(4,3,3,
3,3,3,3,4),(177.03923381194,177.130849992503,177.628408559898,178.125967127293,
178.623525694687,179.121084262082,179.618642829477,180.09311837215),
 .UNSPECIFIED.);
#800=B_SPLINE_CURVE_WITH_KNOTS('',3,(#68436,#68437,#68438,#68439,#68440,
#68441,#68442,#68443,#68444,#68445,#68446,#68447,#68448,#68449,#68450,#68451,
#68452,#68453,#68454,#68455,#68456,#68457,#68458,#68459,#68460,#68461,#68462,
#68463,#68464,#68465,#68466,#68467,#68468,#68469,#68470,#68471,#68472,#68473,
#68474,#68475,#68476,#68477,#68478,#68479,#68480,#68481,#68482,#68483,#68484,
#68485,#68486,#68487,#68488,#68489,#68490,#68491,#68492,#68493,#68494,#68495,
#68496,#68497,#68498,#68499,#68500,#68501,#68502,#68503,#68504,#68505,#68506,
#68507,#68508,#68509,#68510,#68511,#68512,#68513,#68514,#68515,#68516,#68517,
#68518,#68519,#68520,#68521,#68522,#68523,#68524,#68525,#68526,#68527,#68528,
#68529,#68530,#68531,#68532,#68533,#68534,#68535,#68536,#68537,#68538,#68539,
#68540,#68541,#68542,#68543,#68544),.UNSPECIFIED.,.F.,.F.,(4,3,3,3,3,3,
3,3,3,3,3,3,3,3,3,3,3,3,3,3,3,3,3,3,3,3,3,3,3,3,3,3,3,3,3,3,4),(-1.2007306413486,
-1.18778889510928,-1.13988090885874,-1.09143646452528,-1.0716790710066,
-1.06368126691445,-1.01465795435031,-0.965525827699372,-0.949331916721051,
-0.939879020937942,-0.932830289337633,-0.904080313500891,-0.855201231210953,
-0.805662560079378,-0.75704812482572,-0.720587298385477,-0.712370780336783,
-0.705760796757552,-0.655179359089079,-0.611204819064748,-0.560866235739618,
-0.510236859441321,-0.485178943719314,-0.478744677456852,-0.42767953585913,
-0.376207404286961,-0.324773913556237,-0.309773533665262,-0.271051841957104,
-0.254111101834785,-0.243588942121311,-0.23718270326285,-0.185842150821897,
-0.133559088665273,-0.0811710250067116,-0.0293189950592701,0.),
 .UNSPECIFIED.);
#801=B_SPLINE_CURVE_WITH_KNOTS('',3,(#68545,#68546,#68547,#68548,#68549,
#68550,#68551,#68552,#68553,#68554,#68555,#68556,#68557,#68558),
 .UNSPECIFIED.,.F.,.F.,(4,1,1,1,1,1,1,1,1,1,1,4),(10.3280500441581,10.8025255868315,
11.3000841542261,11.7976427216208,12.2952012890155,12.7927598564102,13.2903184238048,
13.7878769911995,14.2854355585942,14.7829941259888,15.2805526933835,15.707963267949),
 .UNSPECIFIED.);
#802=B_SPLINE_CURVE_WITH_KNOTS('',3,(#68564,#68565,#68566,#68567,#68568,
#68569,#68570,#68571,#68572,#68573,#68574,#68575,#68576,#68577,#68578,#68579,
#68580,#68581,#68582,#68583,#68584,#68585,#68586,#68587,#68588,#68589,#68590,
#68591,#68592,#68593,#68594,#68595,#68596,#68597,#68598,#68599,#68600,#68601,
#68602,#68603,#68604,#68605,#68606,#68607,#68608,#68609,#68610,#68611,#68612,
#68613,#68614,#68615,#68616,#68617,#68618,#68619,#68620,#68621,#68622,#68623,
#68624,#68625,#68626,#68627,#68628,#68629,#68630,#68631,#68632,#68633,#68634,
#68635,#68636,#68637,#68638,#68639,#68640,#68641,#68642,#68643,#68644,#68645,
#68646,#68647,#68648,#68649,#68650,#68651,#68652,#68653,#68654,#68655,#68656,
#68657,#68658,#68659,#68660,#68661,#68662,#68663,#68664,#68665,#68666,#68667,
#68668,#68669,#68670,#68671,#68672,#68673,#68674,#68675),.UNSPECIFIED.,
 .F.,.F.,(4,3,3,3,3,3,3,3,3,3,3,3,3,3,3,3,3,3,3,3,3,3,3,3,3,3,3,3,3,3,3,
3,3,3,3,3,3,4),(-1.19772932745415,-1.18324084153908,-1.13092606079167,-1.07854075497836,
-1.06423152144802,-1.05378540334809,-1.04571659768592,-0.993876688885037,
-0.942396624390617,-0.92423148651965,-0.91362752205776,-0.90667123366724,
-0.875156121752115,-0.824147097414577,-0.772884353235954,-0.723395591056853,
-0.686279019422527,-0.677622814824214,-0.671424747566094,-0.621152035937331,
-0.574929304519549,-0.524525824283539,-0.474360650973971,-0.450422418698554,
-0.444347128932818,-0.394859086211904,-0.345424002104565,-0.296617994979428,
-0.283145695127844,-0.247752483236863,-0.23226795303456,-0.222024799667534,
-0.215891341869747,-0.167475088741914,-0.118834100956772,-0.0705281023105065,
-0.0231956289141124,0.),.UNSPECIFIED.);
#803=B_SPLINE_CURVE_WITH_KNOTS('',3,(#68678,#68679,#68680,#68681,#68682,
#68683,#68684,#68685,#68686,#68687,#68688,#68689),.UNSPECIFIED.,.F.,.F.,
(4,1,1,1,1,1,1,1,1,4),(11.6630985309706,12.1606570983653,12.65821566576,
13.1557742331546,13.6533328005493,14.150891367944,14.6484499353386,15.1460085027333,
15.643567070128,15.7079632679491),.UNSPECIFIED.);
#804=B_SPLINE_CURVE_WITH_KNOTS('',3,(#70166,#70167,#70168,#70169,#70170,
#70171,#70172,#70173,#70174,#70175,#70176,#70177,#70178,#70179,#70180,#70181),
 .UNSPECIFIED.,.F.,.F.,(4,3,3,3,3,4),(-182.10643566645,-181.608877099055,
-181.111318531661,-180.613759964266,-180.116201396871,-179.974053338007),
 .UNSPECIFIED.);
#805=B_SPLINE_CURVE_WITH_KNOTS('',3,(#70885,#70886,#70887,#70888,#70889,
#70890,#70891,#70892,#70893,#70894,#70895,#70896,#70897,#70898,#70899,#70900,
#70901,#70902,#70903),.UNSPECIFIED.,.F.,.F.,(4,3,3,3,3,3,4),(-0.229761503419508,
-0.206166571473124,-0.159724811114511,-0.12550437800065,-0.0807834581112385,
-0.0377756277020877,0.),.UNSPECIFIED.);
#806=B_SPLINE_CURVE_WITH_KNOTS('',3,(#70907,#70908,#70909,#70910,#70911,
#70912,#70913,#70914,#70915,#70916,#70917,#70918,#70919,#70920,#70921,#70922,
#70923,#70924,#70925,#70926,#70927,#70928,#70929,#70930,#70931,#70932,#70933,
#70934,#70935,#70936,#70937,#70938,#70939,#70940,#70941,#70942,#70943),
 .UNSPECIFIED.,.F.,.F.,(4,3,3,3,3,3,3,3,3,3,3,3,4),(-0.459480514361734,
-0.443345601466461,-0.398418086430754,-0.369143093793813,-0.320534667577263,
-0.278580845736582,-0.221174845679046,-0.206166571473069,-0.159724811114448,
-0.125504378000605,-0.0807878344312463,-0.037784169760125,0.),
 .UNSPECIFIED.);
#807=B_SPLINE_CURVE_WITH_KNOTS('',3,(#70947,#70948,#70949,#70950,#70951,
#70952,#70953,#70954,#70955,#70956,#70957,#70958,#70959,#70960,#70961,#70962,
#70963,#70964,#70965,#70966,#70967,#70968,#70969,#70970,#70971,#70972,#70973,
#70974,#70975,#70976,#70977,#70978,#70979,#70980,#70981,#70982,#70983,#70984,
#70985,#70986,#70987,#70988,#70989),.UNSPECIFIED.,.F.,.F.,(4,3,3,3,3,3,
3,3,3,3,3,3,3,3,4),(-0.459480514361606,-0.416804016852846,-0.373075117462449,
-0.369143093793734,-0.322563532475183,-0.299796705045319,-0.27858084573658,
-0.220296138014231,-0.206166571473084,-0.154844056501134,-0.125504378000612,
-0.0790936974906717,-0.0343817313041713,-0.0161363994082055,0.),
 .UNSPECIFIED.);
#808=B_SPLINE_CURVE_WITH_KNOTS('',3,(#70993,#70994,#70995,#70996,#70997,
#70998,#70999,#71000,#71001,#71002,#71003,#71004,#71005,#71006,#71007,#71008,
#71009,#71010,#71011,#71012,#71013,#71014,#71015,#71016,#71017,#71018,#71019,
#71020,#71021,#71022,#71023,#71024,#71025,#71026,#71027,#71028,#71029),
 .UNSPECIFIED.,.F.,.F.,(4,3,3,3,3,3,3,3,3,3,3,3,4),(-0.459480514362015,
-0.443345601466716,-0.398421538221141,-0.369143093793975,-0.320538018706025,
-0.278580845736683,-0.221183542332208,-0.206166571473132,-0.159724811114509,
-0.125504378000635,-0.0807834581110674,-0.0377756277020226,0.),
 .UNSPECIFIED.);
#809=B_SPLINE_CURVE_WITH_KNOTS('',3,(#71033,#71034,#71035,#71036,#71037,
#71038,#71039,#71040,#71041,#71042,#71043,#71044,#71045,#71046,#71047,#71048,
#71049,#71050,#71051,#71052,#71053,#71054,#71055,#71056,#71057,#71058,#71059,
#71060,#71061,#71062,#71063,#71064,#71065,#71066,#71067,#71068,#71069),
 .UNSPECIFIED.,.F.,.F.,(4,3,3,3,3,3,3,3,3,3,3,3,4),(-0.459480514361764,
-0.443345601466454,-0.398418086430042,-0.369143093793749,-0.320534667578597,
-0.278580845736547,-0.221174845680044,-0.206166571473085,-0.159724811114519,
-0.12550437800065,-0.0807878344311111,-0.0377841697597962,0.),
 .UNSPECIFIED.);
#810=B_SPLINE_CURVE_WITH_KNOTS('',3,(#71073,#71074,#71075,#71076,#71077,
#71078,#71079,#71080,#71081,#71082,#71083,#71084,#71085,#71086,#71087,#71088,
#71089,#71090,#71091,#71092,#71093,#71094,#71095,#71096,#71097,#71098,#71099,
#71100,#71101,#71102,#71103,#71104,#71105,#71106,#71107,#71108,#71109,#71110,
#71111,#71112,#71113,#71114,#71115),.UNSPECIFIED.,.F.,.F.,(4,3,3,3,3,3,
3,3,3,3,3,3,3,3,4),(-0.45948051436171,-0.416804016851814,-0.373075117460496,
-0.369143093793726,-0.322563532475871,-0.299796705045298,-0.278580845736541,
-0.22029613801833,-0.206166571473066,-0.154844056502094,-0.125504378000622,
-0.0790936974907238,-0.0343817313044943,-0.0161363994082399,0.),
 .UNSPECIFIED.);
#811=B_SPLINE_CURVE_WITH_KNOTS('',3,(#71118,#71119,#71120,#71121,#71122,
#71123,#71124,#71125,#71126,#71127,#71128,#71129,#71130,#71131,#71132,#71133,
#71134,#71135,#71136),.UNSPECIFIED.,.F.,.F.,(4,3,3,3,3,3,4),(-0.459480514361756,
-0.443345601466462,-0.398421538221248,-0.369143093793824,-0.320538018705387,
-0.278580845736626,-0.229761503419508),.UNSPECIFIED.);
#812=B_SPLINE_CURVE_WITH_KNOTS('',3,(#71162,#71163,#71164,#71165),
 .UNSPECIFIED.,.F.,.F.,(4,4),(0.906486097601391,1.2005720772214),
 .UNSPECIFIED.);
#813=B_SPLINE_CURVE_WITH_KNOTS('',3,(#71167,#71168,#71169,#71170,#71171,
#71172),.UNSPECIFIED.,.F.,.F.,(4,2,4),(-0.0856551294938672,-0.0428224901510306,
0.),.UNSPECIFIED.);
#814=B_SPLINE_CURVE_WITH_KNOTS('',3,(#71174,#71175,#71176,#71177,#71178,
#71179),.UNSPECIFIED.,.F.,.F.,(4,1,1,4),(-1.19740918080757,-0.889549641576921,
-0.578527205932438,-0.115156448879797),.UNSPECIFIED.);
#815=B_SPLINE_CURVE_WITH_KNOTS('',3,(#71181,#71182,#71183,#71184,#71185,
#71186),.UNSPECIFIED.,.F.,.F.,(4,2,4),(-0.0856551215567144,-0.0428321834459229,
0.),.UNSPECIFIED.);
#816=B_SPLINE_CURVE_WITH_KNOTS('',3,(#71187,#71188,#71189,#71190),
 .UNSPECIFIED.,.F.,.F.,(4,4),(0.111993552465714,0.406079532085727),
 .UNSPECIFIED.);
#817=B_SPLINE_CURVE_WITH_KNOTS('',3,(#71216,#71217,#71218,#71219),
 .UNSPECIFIED.,.F.,.F.,(4,4),(0.90648609760139,1.2005720772214),
 .UNSPECIFIED.);
#818=B_SPLINE_CURVE_WITH_KNOTS('',3,(#71221,#71222,#71223,#71224,#71225,
#71226),.UNSPECIFIED.,.F.,.F.,(4,2,4),(-0.0856551294979727,-0.0428224901518006,
0.),.UNSPECIFIED.);
#819=B_SPLINE_CURVE_WITH_KNOTS('',3,(#71228,#71229,#71230,#71231,#71232,
#71233),.UNSPECIFIED.,.F.,.F.,(4,1,1,4),(-1.19740918080757,-0.889549641576921,
-0.578527205932438,-0.115156448879797),.UNSPECIFIED.);
#820=B_SPLINE_CURVE_WITH_KNOTS('',3,(#71234,#71235,#71236,#71237,#71238,
#71239),.UNSPECIFIED.,.F.,.F.,(4,2,4),(-0.0856551215544335,-0.0428321834456351,
0.),.UNSPECIFIED.);
#821=B_SPLINE_CURVE_WITH_KNOTS('',3,(#71240,#71241,#71242,#71243),
 .UNSPECIFIED.,.F.,.F.,(4,4),(0.111993552465714,0.406079532085726),
 .UNSPECIFIED.);
#822=B_SPLINE_CURVE_WITH_KNOTS('',3,(#71246,#71247,#71248,#71249),
 .UNSPECIFIED.,.F.,.F.,(4,4),(0.111993552465713,0.406079532085725),
 .UNSPECIFIED.);
#823=B_SPLINE_CURVE_WITH_KNOTS('',3,(#71252,#71253,#71254,#71255),
 .UNSPECIFIED.,.F.,.F.,(4,4),(0.111993552465714,0.406079532085727),
 .UNSPECIFIED.);
#824=B_SPLINE_CURVE_WITH_KNOTS('',3,(#71256,#71257,#71258,#71259),
 .UNSPECIFIED.,.F.,.F.,(4,4),(0.906486097601392,1.2005720772214),
 .UNSPECIFIED.);
#825=B_SPLINE_CURVE_WITH_KNOTS('',3,(#71262,#71263,#71264,#71265),
 .UNSPECIFIED.,.F.,.F.,(4,4),(0.111993552465714,0.406079532085725),
 .UNSPECIFIED.);
#826=B_SPLINE_CURVE_WITH_KNOTS('',3,(#71266,#71267,#71268,#71269),
 .UNSPECIFIED.,.F.,.F.,(4,4),(0.906486097601392,1.2005720772214),
 .UNSPECIFIED.);
#827=B_SPLINE_CURVE_WITH_KNOTS('',3,(#71272,#71273,#71274,#71275),
 .UNSPECIFIED.,.F.,.F.,(4,4),(0.111993552465714,0.406079532085727),
 .UNSPECIFIED.);
#828=B_SPLINE_CURVE_WITH_KNOTS('',3,(#71276,#71277,#71278,#71279),
 .UNSPECIFIED.,.F.,.F.,(4,4),(0.906486097601392,1.20057207722141),
 .UNSPECIFIED.);
#829=B_SPLINE_CURVE_WITH_KNOTS('',3,(#71281,#71282,#71283,#71284),
 .UNSPECIFIED.,.F.,.F.,(4,4),(0.906486097601391,1.2005720772214),
 .UNSPECIFIED.);
#830=B_SPLINE_CURVE_WITH_KNOTS('',3,(#71310,#71311,#71312,#71313,#71314,
#71315),.UNSPECIFIED.,.F.,.F.,(4,2,4),(-0.0856551294832383,-0.0428224901484855,
0.),.UNSPECIFIED.);
#831=B_SPLINE_CURVE_WITH_KNOTS('',3,(#71317,#71318,#71319,#71320,#71321,
#71322),.UNSPECIFIED.,.F.,.F.,(4,1,1,4),(-1.19740918080757,-0.734038423754679,
-0.423015988110196,-0.115156448879796),.UNSPECIFIED.);
#832=B_SPLINE_CURVE_WITH_KNOTS('',3,(#71323,#71324,#71325,#71326,#71327,
#71328),.UNSPECIFIED.,.F.,.F.,(4,2,4),(-0.0856551215544496,-0.0428321834445534,
0.),.UNSPECIFIED.);
#833=B_SPLINE_CURVE_WITH_KNOTS('',3,(#71367,#71368,#71369,#71370,#71371,
#71372),.UNSPECIFIED.,.F.,.F.,(4,2,4),(-0.0856551215520138,-0.042832183445196,
0.),.UNSPECIFIED.);
#834=B_SPLINE_CURVE_WITH_KNOTS('',3,(#71398,#71399,#71400,#71401,#71402,
#71403),.UNSPECIFIED.,.F.,.F.,(4,2,4),(-0.0856551294860877,-0.0428224901488512,
0.),.UNSPECIFIED.);
#835=B_SPLINE_CURVE_WITH_KNOTS('',3,(#71405,#71406,#71407,#71408,#71409,
#71410),.UNSPECIFIED.,.F.,.F.,(4,2,4),(-0.0856551215570029,-0.0428321834468217,
0.),.UNSPECIFIED.);
#836=B_SPLINE_CURVE_WITH_KNOTS('',3,(#71415,#71416,#71417,#71418,#71419,
#71420),.UNSPECIFIED.,.F.,.F.,(4,2,4),(-0.0856551294977852,-0.0428224901521715,
0.),.UNSPECIFIED.);
#837=B_SPLINE_CURVE_WITH_KNOTS('',3,(#71423,#71424,#71425,#71426,#71427,
#71428),.UNSPECIFIED.,.F.,.F.,(4,2,4),(-0.085655129500155,-0.0428224901528902,
0.),.UNSPECIFIED.);
#838=B_SPLINE_CURVE_WITH_KNOTS('',3,(#71430,#71431,#71432,#71433,#71434,
#71435),.UNSPECIFIED.,.F.,.F.,(4,2,4),(-0.0856551215531883,-0.0428321834438049,
0.),.UNSPECIFIED.);
#839=B_SPLINE_CURVE_WITH_KNOTS('',3,(#71461,#71462,#71463,#71464,#71465,
#71466),.UNSPECIFIED.,.F.,.F.,(4,1,1,4),(-1.19740918080757,-0.73403842375468,
-0.423015988110197,-0.115156448879797),.UNSPECIFIED.);
#840=B_SPLINE_CURVE_WITH_KNOTS('',3,(#71494,#71495,#71496,#71497,#71498,
#71499),.UNSPECIFIED.,.F.,.F.,(4,1,1,4),(-1.19740918080757,-0.889549641576922,
-0.578527205932439,-0.115156448879796),.UNSPECIFIED.);
#841=B_SPLINE_CURVE_WITH_KNOTS('',3,(#71530,#71531,#71532,#71533,#71534,
#71535),.UNSPECIFIED.,.F.,.F.,(4,1,1,4),(-1.19740918080757,-0.889549641576921,
-0.578527205932438,-0.115156448879797),.UNSPECIFIED.);
#842=ELLIPSE('',#34430,192.333044482741,136.);
#843=ELLIPSE('',#34431,192.333044482741,136.);
#844=ELLIPSE('',#34435,192.333044482741,136.);
#845=ELLIPSE('',#34436,192.333044482741,136.);
#846=ELLIPSE('',#34438,192.333044482741,136.);
#847=ELLIPSE('',#34440,192.333044482741,136.);
#848=ELLIPSE('',#34441,192.333044482741,136.);
#849=ELLIPSE('',#34443,192.333044482741,136.);
#850=ELLIPSE('',#34444,192.333044482741,136.);
#851=ELLIPSE('',#34446,192.333044482741,136.);
#852=ELLIPSE('',#34447,192.33304448274,136.);
#853=ELLIPSE('',#34449,192.33304448274,136.);
#854=ELLIPSE('',#34450,192.333044482742,136.);
#855=ELLIPSE('',#34452,192.333044482743,136.);
#856=ELLIPSE('',#34453,192.333044482742,136.);
#857=ELLIPSE('',#34455,192.33304448274,136.);
#858=ELLIPSE('',#34456,192.33304448274,136.);
#859=ELLIPSE('',#34458,192.333044482743,136.);
#860=ELLIPSE('',#34459,192.333044482742,136.);
#861=ELLIPSE('',#34461,192.33304448274,136.);
#862=ELLIPSE('',#34462,192.333044482743,136.);
#863=ELLIPSE('',#34464,192.333044482739,136.);
#864=ELLIPSE('',#34465,192.333044482741,136.);
#865=ELLIPSE('',#34467,192.333044482745,136.);
#866=ELLIPSE('',#34468,192.333044482737,136.);
#867=ELLIPSE('',#34470,192.333044482741,136.);
#868=ELLIPSE('',#34471,192.333044482739,136.);
#869=ELLIPSE('',#34473,192.333044482738,136.);
#870=ELLIPSE('',#34474,192.333044482739,136.);
#871=ELLIPSE('',#34476,192.333044482743,136.);
#872=ELLIPSE('',#34477,192.333044482742,136.);
#873=ELLIPSE('',#34479,192.333044482738,136.);
#874=ELLIPSE('',#34480,192.333044482743,136.);
#875=ELLIPSE('',#34482,192.333044482741,136.);
#876=ELLIPSE('',#34483,192.333044482741,136.);
#877=ELLIPSE('',#34485,192.333044482741,136.);
#878=ELLIPSE('',#34486,192.333044482743,136.);
#879=ELLIPSE('',#34488,192.333044482743,136.);
#880=ELLIPSE('',#34489,192.33304448274,136.);
#881=ELLIPSE('',#34491,192.333044482743,136.);
#882=ELLIPSE('',#34492,192.33304448274,136.);
#883=ELLIPSE('',#34494,192.33304448274,136.);
#884=ELLIPSE('',#34495,192.33304448274,136.);
#885=ELLIPSE('',#34497,192.33304448274,136.);
#886=ELLIPSE('',#34498,192.333044482738,136.);
#887=ELLIPSE('',#34500,192.333044482741,136.);
#888=ELLIPSE('',#34501,192.333044482741,136.);
#889=ELLIPSE('',#34503,192.33304448274,136.);
#890=ELLIPSE('',#34504,192.33304448274,136.);
#891=ELLIPSE('',#34506,192.333044482742,136.);
#892=ELLIPSE('',#34507,192.333044482741,136.);
#893=ELLIPSE('',#34509,192.33304448274,136.);
#894=ELLIPSE('',#34510,192.333044482743,136.);
#895=ELLIPSE('',#34512,192.33304448274,136.);
#896=ELLIPSE('',#34513,192.33304448274,136.);
#897=ELLIPSE('',#34515,192.333044482739,136.);
#898=ELLIPSE('',#34516,192.33304448274,136.);
#899=ELLIPSE('',#34518,192.33304448274,136.);
#900=ELLIPSE('',#34519,192.33304448274,136.);
#901=ELLIPSE('',#34521,192.333044482739,136.);
#902=ELLIPSE('',#34522,192.333044482741,136.);
#903=ELLIPSE('',#34524,192.333044482743,136.);
#904=ELLIPSE('',#34525,192.333044482743,136.);
#905=ELLIPSE('',#34527,192.333044482741,136.);
#906=ELLIPSE('',#34528,192.333044482742,136.);
#907=ELLIPSE('',#34530,192.333044482741,136.);
#908=ELLIPSE('',#34531,192.333044482741,136.);
#909=ELLIPSE('',#34533,192.333044482742,136.);
#910=ELLIPSE('',#34534,192.333044482742,136.);
#911=ELLIPSE('',#34536,192.333044482742,136.);
#912=ELLIPSE('',#34537,192.333044482741,136.);
#913=ELLIPSE('',#34539,192.333044482741,136.);
#914=ELLIPSE('',#34540,192.333044482742,136.);
#915=ELLIPSE('',#34542,192.333044482741,136.);
#916=ELLIPSE('',#34543,192.33304448274,136.);
#917=ELLIPSE('',#34545,192.333044482742,136.);
#918=ELLIPSE('',#34546,192.333044482741,136.);
#919=ELLIPSE('',#34548,192.333044482741,136.);
#920=ELLIPSE('',#34549,192.33304448274,136.);
#921=ELLIPSE('',#34551,192.33304448274,136.);
#922=ELLIPSE('',#34552,192.333044482741,136.);
#923=ELLIPSE('',#34554,192.333044482743,136.);
#924=ELLIPSE('',#34555,192.333044482741,136.);
#925=ELLIPSE('',#34557,192.33304448274,136.);
#926=ELLIPSE('',#34558,192.33304448274,136.);
#927=ELLIPSE('',#34560,192.333044482742,136.);
#928=ELLIPSE('',#34561,192.333044482742,136.);
#929=ELLIPSE('',#34563,192.333044482742,136.);
#930=ELLIPSE('',#34564,192.333044482743,136.);
#931=ELLIPSE('',#34566,192.33304448274,136.);
#932=ELLIPSE('',#34567,192.333044482741,136.);
#933=ELLIPSE('',#34569,192.333044482745,136.);
#934=ELLIPSE('',#34570,192.33304448274,136.);
#935=ELLIPSE('',#34572,192.333044482743,136.);
#936=ELLIPSE('',#34573,192.333044482741,136.);
#937=ELLIPSE('',#34575,192.33304448274,136.);
#938=ELLIPSE('',#34576,192.33304448274,136.);
#939=ELLIPSE('',#34578,192.333044482743,136.);
#940=ELLIPSE('',#34579,192.333044482742,136.);
#941=ELLIPSE('',#34581,192.33304448274,136.);
#942=ELLIPSE('',#34582,192.333044482742,136.);
#943=ELLIPSE('',#34584,192.333044482741,136.);
#944=ELLIPSE('',#34585,192.333044482741,136.);
#945=ELLIPSE('',#34587,192.333044482741,136.);
#946=ELLIPSE('',#34588,192.333044482743,136.);
#947=ELLIPSE('',#34590,192.333044482741,136.);
#948=ELLIPSE('',#34591,192.33304448274,136.);
#949=ELLIPSE('',#34593,192.333044482743,136.);
#950=ELLIPSE('',#34594,192.33304448274,136.);
#951=ELLIPSE('',#34596,192.33304448274,136.);
#952=ELLIPSE('',#34597,192.33304448274,136.);
#953=ELLIPSE('',#34599,192.33304448274,136.);
#954=ELLIPSE('',#34600,192.333044482738,136.);
#955=ELLIPSE('',#34602,192.333044482741,136.);
#956=ELLIPSE('',#34603,192.333044482741,136.);
#957=ELLIPSE('',#34605,192.333044482738,136.);
#958=ELLIPSE('',#34606,192.333044482743,136.);
#959=ELLIPSE('',#34608,192.333044482742,136.);
#960=ELLIPSE('',#34609,192.333044482741,136.);
#961=ELLIPSE('',#34611,192.33304448274,136.);
#962=ELLIPSE('',#34612,192.333044482741,136.);
#963=ELLIPSE('',#34614,192.333044482739,136.);
#964=ELLIPSE('',#34615,192.33304448274,136.);
#965=ELLIPSE('',#34617,192.333044482741,136.);
#966=ELLIPSE('',#34618,192.333044482741,136.);
#967=ELLIPSE('',#34620,192.333044482739,136.);
#968=ELLIPSE('',#34621,192.333044482738,136.);
#969=ELLIPSE('',#34623,192.333044482741,136.);
#970=ELLIPSE('',#34624,192.333044482743,136.);
#971=ELLIPSE('',#34626,192.333044482743,136.);
#972=ELLIPSE('',#34627,192.333044482743,136.);
#973=ELLIPSE('',#34629,192.333044482741,136.);
#974=ELLIPSE('',#34630,192.333044482741,136.);
#975=ELLIPSE('',#34632,192.333044482741,136.);
#976=ELLIPSE('',#34633,192.333044482741,136.);
#977=ELLIPSE('',#34635,192.333044482742,136.);
#978=ELLIPSE('',#34636,192.333044482743,136.);
#979=ELLIPSE('',#34638,192.33304448274,136.);
#980=ELLIPSE('',#34639,192.333044482739,136.);
#981=ELLIPSE('',#34641,192.333044482742,136.);
#982=ELLIPSE('',#34642,192.333044482741,136.);
#983=ELLIPSE('',#34644,192.33304448274,136.);
#984=ELLIPSE('',#34645,192.33304448274,136.);
#985=ELLIPSE('',#34647,192.333044482741,136.);
#986=ELLIPSE('',#34648,192.333044482741,136.);
#987=ELLIPSE('',#34650,192.333044482741,136.);
#988=ELLIPSE('',#34651,192.33304448274,136.);
#989=ELLIPSE('',#34653,192.333044482741,136.);
#990=ELLIPSE('',#34654,192.333044482741,136.);
#991=ELLIPSE('',#34656,192.333044482741,136.);
#992=ELLIPSE('',#34657,192.33304448274,136.);
#993=ELLIPSE('',#34659,192.33304448274,136.);
#994=ELLIPSE('',#34660,192.333044482742,136.);
#995=ELLIPSE('',#34662,192.333044482743,136.);
#996=ELLIPSE('',#34663,192.333044482742,136.);
#997=ELLIPSE('',#34665,192.33304448274,136.);
#998=ELLIPSE('',#34666,192.333044482741,136.);
#999=ELLIPSE('',#34668,192.333044482742,136.);
#1000=ELLIPSE('',#34669,192.333044482742,136.);
#1001=ELLIPSE('',#34671,192.33304448274,136.);
#1002=ELLIPSE('',#34672,192.333044482745,136.);
#1003=ELLIPSE('',#34674,192.333044482739,136.);
#1004=ELLIPSE('',#34675,192.333044482741,136.);
#1005=ELLIPSE('',#34677,192.333044482745,136.);
#1006=ELLIPSE('',#34678,192.333044482739,136.);
#1007=ELLIPSE('',#34680,192.333044482741,136.);
#1008=ELLIPSE('',#34681,192.333044482741,136.);
#1009=ELLIPSE('',#34683,192.333044482738,136.);
#1010=ELLIPSE('',#34684,192.33304448274,136.);
#1011=ELLIPSE('',#34686,192.333044482743,136.);
#1012=ELLIPSE('',#34687,192.333044482742,136.);
#1013=ELLIPSE('',#34689,192.33304448274,136.);
#1014=ELLIPSE('',#34690,192.333044482742,136.);
#1015=ELLIPSE('',#34692,192.333044482741,136.);
#1016=ELLIPSE('',#34693,192.333044482741,136.);
#1017=ELLIPSE('',#34695,192.333044482741,136.);
#1018=ELLIPSE('',#34696,192.333044482743,136.);
#1019=ELLIPSE('',#34698,192.333044482743,136.);
#1020=ELLIPSE('',#34699,192.33304448274,136.);
#1021=ELLIPSE('',#34701,192.333044482743,136.);
#1022=ELLIPSE('',#34702,192.333044482738,136.);
#1023=ELLIPSE('',#34704,192.33304448274,136.);
#1024=ELLIPSE('',#34705,192.33304448274,136.);
#1025=ELLIPSE('',#34707,192.33304448274,136.);
#1026=ELLIPSE('',#34708,192.333044482738,136.);
#1027=ELLIPSE('',#34710,192.333044482741,136.);
#1028=ELLIPSE('',#34711,192.333044482741,136.);
#1029=ELLIPSE('',#34713,192.333044482738,136.);
#1030=ELLIPSE('',#34714,192.333044482743,136.);
#1031=ELLIPSE('',#34716,192.333044482742,136.);
#1032=ELLIPSE('',#34717,192.333044482741,136.);
#1033=ELLIPSE('',#34719,192.33304448274,136.);
#1034=ELLIPSE('',#34720,192.333044482744,136.);
#1035=ELLIPSE('',#34722,192.33304448274,136.);
#1036=ELLIPSE('',#34723,192.33304448274,136.);
#1037=ELLIPSE('',#34725,192.333044482741,136.);
#1038=ELLIPSE('',#34726,192.333044482741,136.);
#1039=ELLIPSE('',#34728,192.33304448274,136.);
#1040=ELLIPSE('',#34729,192.33304448274,136.);
#1041=ELLIPSE('',#34731,192.333044482741,136.);
#1042=ELLIPSE('',#34732,192.333044482741,136.);
#1043=ELLIPSE('',#34734,192.333044482742,136.);
#1044=ELLIPSE('',#34735,192.333044482741,136.);
#1045=ELLIPSE('',#34737,192.333044482741,136.);
#1046=ELLIPSE('',#34738,192.333044482741,136.);
#1047=ELLIPSE('',#34740,192.33304448274,136.);
#1048=ELLIPSE('',#34741,192.333044482742,136.);
#1049=ELLIPSE('',#34743,192.333044482742,136.);
#1050=ELLIPSE('',#34744,192.333044482743,136.);
#1051=ELLIPSE('',#34746,192.333044482742,136.);
#1052=ELLIPSE('',#34747,192.333044482741,136.);
#1053=ELLIPSE('',#34749,192.333044482741,136.);
#1054=ELLIPSE('',#34750,192.333044482742,136.);
#1055=ELLIPSE('',#34752,192.333044482741,136.);
#1056=ELLIPSE('',#34753,192.33304448274,136.);
#1057=ELLIPSE('',#34755,192.333044482741,136.);
#1058=ELLIPSE('',#34756,192.333044482741,136.);
#1059=ELLIPSE('',#34758,192.333044482741,136.);
#1060=ELLIPSE('',#34759,192.33304448274,136.);
#1061=ELLIPSE('',#34761,192.333044482741,136.);
#1062=ELLIPSE('',#34762,192.333044482741,136.);
#1063=ELLIPSE('',#34764,192.333044482741,136.);
#1064=ELLIPSE('',#34765,192.333044482741,136.);
#1065=ELLIPSE('',#34767,192.33304448274,136.);
#1066=ELLIPSE('',#34768,192.333044482742,136.);
#1067=ELLIPSE('',#34770,192.333044482742,136.);
#1068=ELLIPSE('',#34771,192.333044482741,136.);
#1069=ELLIPSE('',#34773,192.33304448274,136.);
#1070=ELLIPSE('',#34774,192.33304448274,136.);
#1071=ELLIPSE('',#34776,192.333044482742,136.);
#1072=ELLIPSE('',#34777,192.333044482742,136.);
#1073=ELLIPSE('',#34779,192.33304448274,136.);
#1074=ELLIPSE('',#34780,192.333044482742,136.);
#1075=ELLIPSE('',#34782,192.333044482741,136.);
#1076=ELLIPSE('',#34783,192.333044482741,136.);
#1077=ELLIPSE('',#34785,192.333044482743,136.);
#1078=ELLIPSE('',#34786,192.33304448274,136.);
#1079=ELLIPSE('',#34788,192.333044482743,136.);
#1080=ELLIPSE('',#34789,192.333044482742,136.);
#1081=ELLIPSE('',#34791,192.33304448274,136.);
#1082=ELLIPSE('',#34792,192.333044482739,136.);
#1083=ELLIPSE('',#34794,192.333044482741,136.);
#1084=ELLIPSE('',#34795,192.333044482741,136.);
#1085=ELLIPSE('',#34797,192.333044482738,136.);
#1086=ELLIPSE('',#34798,192.333044482743,136.);
#1087=ELLIPSE('',#34800,192.333044482741,136.);
#1088=ELLIPSE('',#34801,192.333044482741,136.);
#1089=ELLIPSE('',#34803,192.333044482741,136.);
#1090=ELLIPSE('',#34804,192.333044482743,136.);
#1091=ELLIPSE('',#34806,192.333044482741,136.);
#1092=ELLIPSE('',#34807,192.33304448274,136.);
#1093=ELLIPSE('',#34809,192.333044482743,136.);
#1094=ELLIPSE('',#34810,192.33304448274,136.);
#1095=ELLIPSE('',#34812,192.33304448274,136.);
#1096=ELLIPSE('',#34813,192.33304448274,136.);
#1097=ELLIPSE('',#34815,192.33304448274,136.);
#1098=ELLIPSE('',#34816,192.333044482738,136.);
#1099=ELLIPSE('',#34818,192.333044482738,136.);
#1100=ELLIPSE('',#34819,192.333044482743,136.);
#1101=ELLIPSE('',#34821,192.333044482738,136.);
#1102=ELLIPSE('',#34822,192.333044482743,136.);
#1103=ELLIPSE('',#34824,192.33304448274,136.);
#1104=ELLIPSE('',#34825,192.33304448274,136.);
#1105=ELLIPSE('',#34827,192.33304448274,136.);
#1106=ELLIPSE('',#34828,192.333044482744,136.);
#1107=ELLIPSE('',#34830,192.33304448274,136.);
#1108=ELLIPSE('',#34831,192.33304448274,136.);
#1109=ELLIPSE('',#34833,192.333044482741,136.);
#1110=ELLIPSE('',#34834,192.333044482741,136.);
#1111=ELLIPSE('',#34836,192.33304448274,136.);
#1112=ELLIPSE('',#34837,192.33304448274,136.);
#1113=ELLIPSE('',#34839,192.333044482741,136.);
#1114=ELLIPSE('',#34840,192.333044482743,136.);
#1115=ELLIPSE('',#34842,192.333044482743,136.);
#1116=ELLIPSE('',#34843,192.33304448274,136.);
#1117=ELLIPSE('',#34845,192.333044482742,136.);
#1118=ELLIPSE('',#34846,192.333044482742,136.);
#1119=ELLIPSE('',#34848,192.333044482741,136.);
#1120=ELLIPSE('',#34849,192.333044482741,136.);
#1121=ELLIPSE('',#34851,192.333044482742,136.);
#1122=ELLIPSE('',#34852,192.333044482743,136.);
#1123=ELLIPSE('',#34854,192.333044482742,136.);
#1124=ELLIPSE('',#34855,192.333044482741,136.);
#1125=ELLIPSE('',#34857,192.333044482741,136.);
#1126=ELLIPSE('',#34858,192.333044482742,136.);
#1127=ELLIPSE('',#34860,192.333044482741,136.);
#1128=ELLIPSE('',#34861,192.33304448274,136.);
#1129=ELLIPSE('',#34863,192.333044482741,136.);
#1130=FACE_BOUND('',#5239,.T.);
#1131=FACE_BOUND('',#5243,.T.);
#1132=FACE_BOUND('',#5247,.T.);
#1133=FACE_BOUND('',#5259,.T.);
#1134=FACE_BOUND('',#5260,.T.);
#1135=FACE_BOUND('',#5261,.T.);
#1136=FACE_BOUND('',#5262,.T.);
#1137=FACE_BOUND('',#5263,.T.);
#1138=FACE_BOUND('',#5264,.T.);
#1139=FACE_BOUND('',#5265,.T.);
#1140=FACE_BOUND('',#5266,.T.);
#1141=FACE_BOUND('',#5267,.T.);
#1142=FACE_BOUND('',#5268,.T.);
#1143=FACE_BOUND('',#5269,.T.);
#1144=FACE_BOUND('',#5270,.T.);
#1145=FACE_BOUND('',#5271,.T.);
#1146=FACE_BOUND('',#5272,.T.);
#1147=FACE_BOUND('',#5273,.T.);
#1148=FACE_BOUND('',#5274,.T.);
#1149=FACE_BOUND('',#5275,.T.);
#1150=FACE_BOUND('',#5276,.T.);
#1151=FACE_BOUND('',#5277,.T.);
#1152=FACE_BOUND('',#5278,.T.);
#1153=FACE_BOUND('',#5279,.T.);
#1154=FACE_BOUND('',#5280,.T.);
#1155=FACE_BOUND('',#5281,.T.);
#1156=FACE_BOUND('',#5282,.T.);
#1157=FACE_BOUND('',#5283,.T.);
#1158=FACE_BOUND('',#5284,.T.);
#1159=FACE_BOUND('',#5285,.T.);
#1160=FACE_BOUND('',#5286,.T.);
#1161=FACE_BOUND('',#5287,.T.);
#1162=FACE_BOUND('',#5288,.T.);
#1163=FACE_BOUND('',#5289,.T.);
#1164=FACE_BOUND('',#5290,.T.);
#1165=FACE_BOUND('',#5291,.T.);
#1166=FACE_BOUND('',#5292,.T.);
#1167=FACE_BOUND('',#5293,.T.);
#1168=FACE_BOUND('',#5294,.T.);
#1169=FACE_BOUND('',#5295,.T.);
#1170=FACE_BOUND('',#5296,.T.);
#1171=FACE_BOUND('',#5297,.T.);
#1172=FACE_BOUND('',#5298,.T.);
#1173=FACE_BOUND('',#5299,.T.);
#1174=FACE_BOUND('',#5300,.T.);
#1175=FACE_BOUND('',#5301,.T.);
#1176=FACE_BOUND('',#5302,.T.);
#1177=FACE_BOUND('',#5303,.T.);
#1178=FACE_BOUND('',#5304,.T.);
#1179=FACE_BOUND('',#5305,.T.);
#1180=FACE_BOUND('',#5306,.T.);
#1181=FACE_BOUND('',#5307,.T.);
#1182=FACE_BOUND('',#5308,.T.);
#1183=FACE_BOUND('',#5309,.T.);
#1184=FACE_BOUND('',#5310,.T.);
#1185=FACE_BOUND('',#5311,.T.);
#1186=FACE_BOUND('',#5312,.T.);
#1187=FACE_BOUND('',#5313,.T.);
#1188=FACE_BOUND('',#5314,.T.);
#1189=FACE_BOUND('',#5315,.T.);
#1190=FACE_BOUND('',#5316,.T.);
#1191=FACE_BOUND('',#5317,.T.);
#1192=FACE_BOUND('',#5318,.T.);
#1193=FACE_BOUND('',#5319,.T.);
#1194=FACE_BOUND('',#5320,.T.);
#1195=FACE_BOUND('',#5321,.T.);
#1196=FACE_BOUND('',#5322,.T.);
#1197=FACE_BOUND('',#5323,.T.);
#1198=FACE_BOUND('',#5324,.T.);
#1199=FACE_BOUND('',#5325,.T.);
#1200=FACE_BOUND('',#5326,.T.);
#1201=FACE_BOUND('',#5327,.T.);
#1202=FACE_BOUND('',#5328,.T.);
#1203=FACE_BOUND('',#5329,.T.);
#1204=FACE_BOUND('',#5347,.T.);
#1205=FACE_BOUND('',#5348,.T.);
#1206=FACE_BOUND('',#5349,.T.);
#1207=FACE_BOUND('',#5350,.T.);
#1208=FACE_BOUND('',#5351,.T.);
#1209=FACE_BOUND('',#5352,.T.);
#1210=FACE_BOUND('',#6399,.T.);
#1211=FACE_BOUND('',#6559,.T.);
#1212=FACE_BOUND('',#6562,.T.);
#1213=FACE_BOUND('',#6565,.T.);
#1214=FACE_BOUND('',#6568,.T.);
#1215=FACE_BOUND('',#6573,.T.);
#1216=FACE_BOUND('',#6574,.T.);
#1217=FACE_BOUND('',#6575,.T.);
#1218=FACE_BOUND('',#6576,.T.);
#1219=FACE_BOUND('',#6577,.T.);
#1220=FACE_BOUND('',#6578,.T.);
#1221=FACE_BOUND('',#6593,.T.);
#1222=FACE_BOUND('',#6631,.T.);
#1223=FACE_BOUND('',#6632,.T.);
#1224=FACE_BOUND('',#6633,.T.);
#1225=FACE_BOUND('',#6634,.T.);
#1226=FACE_BOUND('',#6635,.T.);
#1227=FACE_BOUND('',#6645,.T.);
#1228=FACE_BOUND('',#6646,.T.);
#1229=FACE_BOUND('',#6647,.T.);
#1230=FACE_BOUND('',#6648,.T.);
#1231=FACE_BOUND('',#6649,.T.);
#1232=FACE_BOUND('',#6712,.T.);
#1233=FACE_BOUND('',#6722,.T.);
#1234=FACE_BOUND('',#6730,.T.);
#1235=FACE_BOUND('',#6734,.T.);
#1236=FACE_BOUND('',#6738,.T.);
#1237=FACE_BOUND('',#6747,.T.);
#1238=FACE_BOUND('',#6752,.T.);
#1239=FACE_BOUND('',#6757,.T.);
#1240=FACE_BOUND('',#6760,.T.);
#1241=FACE_BOUND('',#6765,.T.);
#1242=FACE_BOUND('',#6878,.T.);
#1243=FACE_BOUND('',#6879,.T.);
#1244=FACE_BOUND('',#6880,.T.);
#1245=FACE_BOUND('',#6881,.T.);
#1246=FACE_BOUND('',#6882,.T.);
#1247=FACE_BOUND('',#6883,.T.);
#1248=FACE_BOUND('',#6884,.T.);
#1249=FACE_BOUND('',#6885,.T.);
#1250=FACE_BOUND('',#6886,.T.);
#1251=FACE_BOUND('',#6887,.T.);
#1252=FACE_BOUND('',#6888,.T.);
#1253=FACE_BOUND('',#6889,.T.);
#1254=FACE_BOUND('',#6890,.T.);
#1255=FACE_BOUND('',#6891,.T.);
#1256=FACE_BOUND('',#6892,.T.);
#1257=FACE_BOUND('',#6893,.T.);
#1258=FACE_BOUND('',#6894,.T.);
#1259=FACE_BOUND('',#6895,.T.);
#1260=FACE_BOUND('',#6896,.T.);
#1261=FACE_BOUND('',#6897,.T.);
#1262=FACE_BOUND('',#6898,.T.);
#1263=FACE_BOUND('',#6901,.T.);
#1264=FACE_BOUND('',#6906,.T.);
#1265=FACE_BOUND('',#6911,.T.);
#1266=FACE_BOUND('',#6916,.T.);
#1267=FACE_BOUND('',#6919,.T.);
#1268=FACE_BOUND('',#6924,.T.);
#1269=FACE_BOUND('',#7027,.T.);
#1270=FACE_BOUND('',#7028,.T.);
#1271=FACE_BOUND('',#7029,.T.);
#1272=FACE_BOUND('',#7030,.T.);
#1273=FACE_BOUND('',#7031,.T.);
#1274=FACE_BOUND('',#7032,.T.);
#1275=FACE_BOUND('',#7033,.T.);
#1276=FACE_BOUND('',#7034,.T.);
#1277=FACE_BOUND('',#7035,.T.);
#1278=FACE_BOUND('',#7036,.T.);
#1279=FACE_BOUND('',#7037,.T.);
#1280=FACE_BOUND('',#7038,.T.);
#1281=FACE_BOUND('',#7039,.T.);
#1282=FACE_BOUND('',#7040,.T.);
#1283=FACE_BOUND('',#7041,.T.);
#1284=FACE_BOUND('',#7042,.T.);
#1285=FACE_BOUND('',#7043,.T.);
#1286=FACE_BOUND('',#7044,.T.);
#1287=FACE_BOUND('',#7045,.T.);
#1288=FACE_BOUND('',#7048,.T.);
#1289=FACE_BOUND('',#7053,.T.);
#1290=FACE_BOUND('',#7060,.T.);
#1291=FACE_BOUND('',#7063,.T.);
#1292=FACE_BOUND('',#7179,.T.);
#1293=FACE_BOUND('',#7196,.T.);
#1294=FACE_BOUND('',#7208,.T.);
#1295=FACE_BOUND('',#7212,.T.);
#1296=FACE_BOUND('',#7286,.T.);
#1297=FACE_BOUND('',#7446,.T.);
#1298=FACE_BOUND('',#7447,.T.);
#1299=FACE_BOUND('',#7448,.T.);
#1300=FACE_BOUND('',#7449,.T.);
#1301=FACE_BOUND('',#7450,.T.);
#1302=FACE_BOUND('',#7451,.T.);
#1303=FACE_BOUND('',#7452,.T.);
#1304=FACE_BOUND('',#7453,.T.);
#1305=FACE_BOUND('',#7454,.T.);
#1306=FACE_BOUND('',#7455,.T.);
#1307=FACE_BOUND('',#7456,.T.);
#1308=FACE_BOUND('',#7457,.T.);
#1309=FACE_BOUND('',#7458,.T.);
#1310=FACE_BOUND('',#7459,.T.);
#1311=FACE_BOUND('',#7460,.T.);
#1312=FACE_BOUND('',#7461,.T.);
#1313=FACE_BOUND('',#7462,.T.);
#1314=FACE_BOUND('',#7463,.T.);
#1315=FACE_BOUND('',#7464,.T.);
#1316=FACE_BOUND('',#7465,.T.);
#1317=FACE_BOUND('',#7466,.T.);
#1318=FACE_BOUND('',#7467,.T.);
#1319=FACE_BOUND('',#7468,.T.);
#1320=FACE_BOUND('',#7469,.T.);
#1321=FACE_BOUND('',#7470,.T.);
#1322=FACE_BOUND('',#7471,.T.);
#1323=FACE_BOUND('',#7472,.T.);
#1324=FACE_BOUND('',#7473,.T.);
#1325=FACE_BOUND('',#7474,.T.);
#1326=FACE_BOUND('',#7475,.T.);
#1327=FACE_BOUND('',#7476,.T.);
#1328=FACE_BOUND('',#7477,.T.);
#1329=FACE_BOUND('',#7478,.T.);
#1330=FACE_BOUND('',#7479,.T.);
#1331=FACE_BOUND('',#7480,.T.);
#1332=FACE_BOUND('',#7493,.T.);
#1333=FACE_BOUND('',#7523,.T.);
#1334=FACE_BOUND('',#7532,.T.);
#1335=PLANE('',#34379);
#1336=PLANE('',#34387);
#1337=PLANE('',#34396);
#1338=PLANE('',#34906);
#1339=PLANE('',#34912);
#1340=PLANE('',#34913);
#1341=PLANE('',#34914);
#1342=PLANE('',#34915);
#1343=PLANE('',#34916);
#1344=PLANE('',#34917);
#1345=PLANE('',#34918);
#1346=PLANE('',#34919);
#1347=PLANE('',#34920);
#1348=PLANE('',#34921);
#1349=PLANE('',#34922);
#1350=PLANE('',#34923);
#1351=PLANE('',#34924);
#1352=PLANE('',#34925);
#1353=PLANE('',#34926);
#1354=PLANE('',#34927);
#1355=PLANE('',#34928);
#1356=PLANE('',#34929);
#1357=PLANE('',#34930);
#1358=PLANE('',#34931);
#1359=PLANE('',#34932);
#1360=PLANE('',#34933);
#1361=PLANE('',#34934);
#1362=PLANE('',#34935);
#1363=PLANE('',#34936);
#1364=PLANE('',#34937);
#1365=PLANE('',#34938);
#1366=PLANE('',#34939);
#1367=PLANE('',#34940);
#1368=PLANE('',#34941);
#1369=PLANE('',#34942);
#1370=PLANE('',#34943);
#1371=PLANE('',#34944);
#1372=PLANE('',#34945);
#1373=PLANE('',#34946);
#1374=PLANE('',#34947);
#1375=PLANE('',#34948);
#1376=PLANE('',#34949);
#1377=PLANE('',#34950);
#1378=PLANE('',#34951);
#1379=PLANE('',#34952);
#1380=PLANE('',#34953);
#1381=PLANE('',#34954);
#1382=PLANE('',#34955);
#1383=PLANE('',#34956);
#1384=PLANE('',#34957);
#1385=PLANE('',#34958);
#1386=PLANE('',#34959);
#1387=PLANE('',#34960);
#1388=PLANE('',#34961);
#1389=PLANE('',#34962);
#1390=PLANE('',#34963);
#1391=PLANE('',#34964);
#1392=PLANE('',#34965);
#1393=PLANE('',#34966);
#1394=PLANE('',#34967);
#1395=PLANE('',#34968);
#1396=PLANE('',#34969);
#1397=PLANE('',#34970);
#1398=PLANE('',#34971);
#1399=PLANE('',#34972);
#1400=PLANE('',#34973);
#1401=PLANE('',#34974);
#1402=PLANE('',#34975);
#1403=PLANE('',#34976);
#1404=PLANE('',#34977);
#1405=PLANE('',#34978);
#1406=PLANE('',#34979);
#1407=PLANE('',#34980);
#1408=PLANE('',#34981);
#1409=PLANE('',#34982);
#1410=PLANE('',#34983);
#1411=PLANE('',#34984);
#1412=PLANE('',#34985);
#1413=PLANE('',#34986);
#1414=PLANE('',#34987);
#1415=PLANE('',#34988);
#1416=PLANE('',#34989);
#1417=PLANE('',#34990);
#1418=PLANE('',#34991);
#1419=PLANE('',#34992);
#1420=PLANE('',#34993);
#1421=PLANE('',#34994);
#1422=PLANE('',#34995);
#1423=PLANE('',#34996);
#1424=PLANE('',#34997);
#1425=PLANE('',#34998);
#1426=PLANE('',#34999);
#1427=PLANE('',#35000);
#1428=PLANE('',#35001);
#1429=PLANE('',#35002);
#1430=PLANE('',#35003);
#1431=PLANE('',#35004);
#1432=PLANE('',#35005);
#1433=PLANE('',#35006);
#1434=PLANE('',#35007);
#1435=PLANE('',#35008);
#1436=PLANE('',#35009);
#1437=PLANE('',#35010);
#1438=PLANE('',#35011);
#1439=PLANE('',#35012);
#1440=PLANE('',#35013);
#1441=PLANE('',#35014);
#1442=PLANE('',#35015);
#1443=PLANE('',#35016);
#1444=PLANE('',#35017);
#1445=PLANE('',#35018);
#1446=PLANE('',#35019);
#1447=PLANE('',#35020);
#1448=PLANE('',#35021);
#1449=PLANE('',#35022);
#1450=PLANE('',#35023);
#1451=PLANE('',#35024);
#1452=PLANE('',#35025);
#1453=PLANE('',#35026);
#1454=PLANE('',#35027);
#1455=PLANE('',#35028);
#1456=PLANE('',#35029);
#1457=PLANE('',#35030);
#1458=PLANE('',#35031);
#1459=PLANE('',#35032);
#1460=PLANE('',#35033);
#1461=PLANE('',#35034);
#1462=PLANE('',#35035);
#1463=PLANE('',#35036);
#1464=PLANE('',#35037);
#1465=PLANE('',#35038);
#1466=PLANE('',#35039);
#1467=PLANE('',#35040);
#1468=PLANE('',#35041);
#1469=PLANE('',#35042);
#1470=PLANE('',#35043);
#1471=PLANE('',#35044);
#1472=PLANE('',#35045);
#1473=PLANE('',#35046);
#1474=PLANE('',#35047);
#1475=PLANE('',#35048);
#1476=PLANE('',#35049);
#1477=PLANE('',#35050);
#1478=PLANE('',#35051);
#1479=PLANE('',#35052);
#1480=PLANE('',#35053);
#1481=PLANE('',#35054);
#1482=PLANE('',#35055);
#1483=PLANE('',#35056);
#1484=PLANE('',#35057);
#1485=PLANE('',#35058);
#1486=PLANE('',#35059);
#1487=PLANE('',#35060);
#1488=PLANE('',#35061);
#1489=PLANE('',#35062);
#1490=PLANE('',#35063);
#1491=PLANE('',#35064);
#1492=PLANE('',#35065);
#1493=PLANE('',#35066);
#1494=PLANE('',#35067);
#1495=PLANE('',#35068);
#1496=PLANE('',#35069);
#1497=PLANE('',#35070);
#1498=PLANE('',#35071);
#1499=PLANE('',#35072);
#1500=PLANE('',#35073);
#1501=PLANE('',#35074);
#1502=PLANE('',#35075);
#1503=PLANE('',#35076);
#1504=PLANE('',#35077);
#1505=PLANE('',#35078);
#1506=PLANE('',#35079);
#1507=PLANE('',#35080);
#1508=PLANE('',#35081);
#1509=PLANE('',#35082);
#1510=PLANE('',#35083);
#1511=PLANE('',#35084);
#1512=PLANE('',#35085);
#1513=PLANE('',#35086);
#1514=PLANE('',#35087);
#1515=PLANE('',#35088);
#1516=PLANE('',#35089);
#1517=PLANE('',#35090);
#1518=PLANE('',#35091);
#1519=PLANE('',#35092);
#1520=PLANE('',#35093);
#1521=PLANE('',#35094);
#1522=PLANE('',#35095);
#1523=PLANE('',#35096);
#1524=PLANE('',#35097);
#1525=PLANE('',#35098);
#1526=PLANE('',#35099);
#1527=PLANE('',#35100);
#1528=PLANE('',#35101);
#1529=PLANE('',#35102);
#1530=PLANE('',#35103);
#1531=PLANE('',#35104);
#1532=PLANE('',#35105);
#1533=PLANE('',#35106);
#1534=PLANE('',#35107);
#1535=PLANE('',#35108);
#1536=PLANE('',#35109);
#1537=PLANE('',#35110);
#1538=PLANE('',#35111);
#1539=PLANE('',#35112);
#1540=PLANE('',#35113);
#1541=PLANE('',#35114);
#1542=PLANE('',#35115);
#1543=PLANE('',#35116);
#1544=PLANE('',#35117);
#1545=PLANE('',#35118);
#1546=PLANE('',#35119);
#1547=PLANE('',#35120);
#1548=PLANE('',#35121);
#1549=PLANE('',#35122);
#1550=PLANE('',#35123);
#1551=PLANE('',#35124);
#1552=PLANE('',#35125);
#1553=PLANE('',#35126);
#1554=PLANE('',#35127);
#1555=PLANE('',#35128);
#1556=PLANE('',#35129);
#1557=PLANE('',#35130);
#1558=PLANE('',#35131);
#1559=PLANE('',#35132);
#1560=PLANE('',#35133);
#1561=PLANE('',#35134);
#1562=PLANE('',#35135);
#1563=PLANE('',#35136);
#1564=PLANE('',#35137);
#1565=PLANE('',#35138);
#1566=PLANE('',#35139);
#1567=PLANE('',#35140);
#1568=PLANE('',#35141);
#1569=PLANE('',#35142);
#1570=PLANE('',#35143);
#1571=PLANE('',#35144);
#1572=PLANE('',#35145);
#1573=PLANE('',#35146);
#1574=PLANE('',#35147);
#1575=PLANE('',#35148);
#1576=PLANE('',#35149);
#1577=PLANE('',#35150);
#1578=PLANE('',#35151);
#1579=PLANE('',#35152);
#1580=PLANE('',#35153);
#1581=PLANE('',#35154);
#1582=PLANE('',#35155);
#1583=PLANE('',#35156);
#1584=PLANE('',#35157);
#1585=PLANE('',#35158);
#1586=PLANE('',#35159);
#1587=PLANE('',#35160);
#1588=PLANE('',#35161);
#1589=PLANE('',#35162);
#1590=PLANE('',#35163);
#1591=PLANE('',#35164);
#1592=PLANE('',#35165);
#1593=PLANE('',#35166);
#1594=PLANE('',#35167);
#1595=PLANE('',#35168);
#1596=PLANE('',#35169);
#1597=PLANE('',#35170);
#1598=PLANE('',#35171);
#1599=PLANE('',#35172);
#1600=PLANE('',#35173);
#1601=PLANE('',#35174);
#1602=PLANE('',#35175);
#1603=PLANE('',#35176);
#1604=PLANE('',#35177);
#1605=PLANE('',#35178);
#1606=PLANE('',#35179);
#1607=PLANE('',#35180);
#1608=PLANE('',#35181);
#1609=PLANE('',#35182);
#1610=PLANE('',#35183);
#1611=PLANE('',#35184);
#1612=PLANE('',#35185);
#1613=PLANE('',#35186);
#1614=PLANE('',#35187);
#1615=PLANE('',#35188);
#1616=PLANE('',#35189);
#1617=PLANE('',#35190);
#1618=PLANE('',#35191);
#1619=PLANE('',#35192);
#1620=PLANE('',#35193);
#1621=PLANE('',#35194);
#1622=PLANE('',#35195);
#1623=PLANE('',#35196);
#1624=PLANE('',#35197);
#1625=PLANE('',#35198);
#1626=PLANE('',#35199);
#1627=PLANE('',#35200);
#1628=PLANE('',#35201);
#1629=PLANE('',#35202);
#1630=PLANE('',#35203);
#1631=PLANE('',#35204);
#1632=PLANE('',#35205);
#1633=PLANE('',#35206);
#1634=PLANE('',#35207);
#1635=PLANE('',#35208);
#1636=PLANE('',#35209);
#1637=PLANE('',#35210);
#1638=PLANE('',#35211);
#1639=PLANE('',#35212);
#1640=PLANE('',#35213);
#1641=PLANE('',#35214);
#1642=PLANE('',#35215);
#1643=PLANE('',#35216);
#1644=PLANE('',#35217);
#1645=PLANE('',#35218);
#1646=PLANE('',#35219);
#1647=PLANE('',#35220);
#1648=PLANE('',#35221);
#1649=PLANE('',#35222);
#1650=PLANE('',#35223);
#1651=PLANE('',#35224);
#1652=PLANE('',#35225);
#1653=PLANE('',#35226);
#1654=PLANE('',#35227);
#1655=PLANE('',#35228);
#1656=PLANE('',#35229);
#1657=PLANE('',#35230);
#1658=PLANE('',#35231);
#1659=PLANE('',#35232);
#1660=PLANE('',#35233);
#1661=PLANE('',#35234);
#1662=PLANE('',#35235);
#1663=PLANE('',#35236);
#1664=PLANE('',#35237);
#1665=PLANE('',#35238);
#1666=PLANE('',#35239);
#1667=PLANE('',#35240);
#1668=PLANE('',#35241);
#1669=PLANE('',#35242);
#1670=PLANE('',#35243);
#1671=PLANE('',#35244);
#1672=PLANE('',#35245);
#1673=PLANE('',#35246);
#1674=PLANE('',#35247);
#1675=PLANE('',#35248);
#1676=PLANE('',#35249);
#1677=PLANE('',#35250);
#1678=PLANE('',#35251);
#1679=PLANE('',#35252);
#1680=PLANE('',#35253);
#1681=PLANE('',#35254);
#1682=PLANE('',#35255);
#1683=PLANE('',#35256);
#1684=PLANE('',#35257);
#1685=PLANE('',#35258);
#1686=PLANE('',#35259);
#1687=PLANE('',#35260);
#1688=PLANE('',#35261);
#1689=PLANE('',#35262);
#1690=PLANE('',#35263);
#1691=PLANE('',#35264);
#1692=PLANE('',#35265);
#1693=PLANE('',#35266);
#1694=PLANE('',#35267);
#1695=PLANE('',#35268);
#1696=PLANE('',#35269);
#1697=PLANE('',#35270);
#1698=PLANE('',#35271);
#1699=PLANE('',#35272);
#1700=PLANE('',#35273);
#1701=PLANE('',#35274);
#1702=PLANE('',#35275);
#1703=PLANE('',#35276);
#1704=PLANE('',#35277);
#1705=PLANE('',#35278);
#1706=PLANE('',#35279);
#1707=PLANE('',#35280);
#1708=PLANE('',#35281);
#1709=PLANE('',#35282);
#1710=PLANE('',#35283);
#1711=PLANE('',#35284);
#1712=PLANE('',#35285);
#1713=PLANE('',#35286);
#1714=PLANE('',#35287);
#1715=PLANE('',#35288);
#1716=PLANE('',#35289);
#1717=PLANE('',#35290);
#1718=PLANE('',#35291);
#1719=PLANE('',#35292);
#1720=PLANE('',#35293);
#1721=PLANE('',#35294);
#1722=PLANE('',#35295);
#1723=PLANE('',#35296);
#1724=PLANE('',#35297);
#1725=PLANE('',#35298);
#1726=PLANE('',#35299);
#1727=PLANE('',#35300);
#1728=PLANE('',#35301);
#1729=PLANE('',#35302);
#1730=PLANE('',#35303);
#1731=PLANE('',#35304);
#1732=PLANE('',#35305);
#1733=PLANE('',#35306);
#1734=PLANE('',#35307);
#1735=PLANE('',#35308);
#1736=PLANE('',#35309);
#1737=PLANE('',#35310);
#1738=PLANE('',#35311);
#1739=PLANE('',#35312);
#1740=PLANE('',#35313);
#1741=PLANE('',#35314);
#1742=PLANE('',#35315);
#1743=PLANE('',#35316);
#1744=PLANE('',#35317);
#1745=PLANE('',#35318);
#1746=PLANE('',#35319);
#1747=PLANE('',#35320);
#1748=PLANE('',#35321);
#1749=PLANE('',#35322);
#1750=PLANE('',#35323);
#1751=PLANE('',#35324);
#1752=PLANE('',#35325);
#1753=PLANE('',#35326);
#1754=PLANE('',#35327);
#1755=PLANE('',#35328);
#1756=PLANE('',#35329);
#1757=PLANE('',#35330);
#1758=PLANE('',#35331);
#1759=PLANE('',#35332);
#1760=PLANE('',#35333);
#1761=PLANE('',#35334);
#1762=PLANE('',#35335);
#1763=PLANE('',#35336);
#1764=PLANE('',#35337);
#1765=PLANE('',#35338);
#1766=PLANE('',#35339);
#1767=PLANE('',#35340);
#1768=PLANE('',#35341);
#1769=PLANE('',#35342);
#1770=PLANE('',#35343);
#1771=PLANE('',#35344);
#1772=PLANE('',#35345);
#1773=PLANE('',#35346);
#1774=PLANE('',#35347);
#1775=PLANE('',#35348);
#1776=PLANE('',#35349);
#1777=PLANE('',#35350);
#1778=PLANE('',#35351);
#1779=PLANE('',#35352);
#1780=PLANE('',#35353);
#1781=PLANE('',#35354);
#1782=PLANE('',#35355);
#1783=PLANE('',#35356);
#1784=PLANE('',#35357);
#1785=PLANE('',#35358);
#1786=PLANE('',#35359);
#1787=PLANE('',#35360);
#1788=PLANE('',#35361);
#1789=PLANE('',#35362);
#1790=PLANE('',#35363);
#1791=PLANE('',#35364);
#1792=PLANE('',#35365);
#1793=PLANE('',#35366);
#1794=PLANE('',#35367);
#1795=PLANE('',#35368);
#1796=PLANE('',#35369);
#1797=PLANE('',#35370);
#1798=PLANE('',#35371);
#1799=PLANE('',#35372);
#1800=PLANE('',#35373);
#1801=PLANE('',#35374);
#1802=PLANE('',#35375);
#1803=PLANE('',#35376);
#1804=PLANE('',#35377);
#1805=PLANE('',#35378);
#1806=PLANE('',#35379);
#1807=PLANE('',#35380);
#1808=PLANE('',#35381);
#1809=PLANE('',#35382);
#1810=PLANE('',#35383);
#1811=PLANE('',#35384);
#1812=PLANE('',#35385);
#1813=PLANE('',#35386);
#1814=PLANE('',#35387);
#1815=PLANE('',#35388);
#1816=PLANE('',#35389);
#1817=PLANE('',#35390);
#1818=PLANE('',#35391);
#1819=PLANE('',#35392);
#1820=PLANE('',#35393);
#1821=PLANE('',#35394);
#1822=PLANE('',#35395);
#1823=PLANE('',#35396);
#1824=PLANE('',#35397);
#1825=PLANE('',#35398);
#1826=PLANE('',#35399);
#1827=PLANE('',#35400);
#1828=PLANE('',#35401);
#1829=PLANE('',#35402);
#1830=PLANE('',#35403);
#1831=PLANE('',#35404);
#1832=PLANE('',#35405);
#1833=PLANE('',#35406);
#1834=PLANE('',#35407);
#1835=PLANE('',#35408);
#1836=PLANE('',#35409);
#1837=PLANE('',#35410);
#1838=PLANE('',#35411);
#1839=PLANE('',#35412);
#1840=PLANE('',#35413);
#1841=PLANE('',#35414);
#1842=PLANE('',#35415);
#1843=PLANE('',#35416);
#1844=PLANE('',#35417);
#1845=PLANE('',#35418);
#1846=PLANE('',#35419);
#1847=PLANE('',#35420);
#1848=PLANE('',#35421);
#1849=PLANE('',#35422);
#1850=PLANE('',#35423);
#1851=PLANE('',#35424);
#1852=PLANE('',#35425);
#1853=PLANE('',#35426);
#1854=PLANE('',#35427);
#1855=PLANE('',#35428);
#1856=PLANE('',#35429);
#1857=PLANE('',#35430);
#1858=PLANE('',#35431);
#1859=PLANE('',#35432);
#1860=PLANE('',#35433);
#1861=PLANE('',#35434);
#1862=PLANE('',#35435);
#1863=PLANE('',#35436);
#1864=PLANE('',#35437);
#1865=PLANE('',#35438);
#1866=PLANE('',#35439);
#1867=PLANE('',#35440);
#1868=PLANE('',#35441);
#1869=PLANE('',#35442);
#1870=PLANE('',#35443);
#1871=PLANE('',#35444);
#1872=PLANE('',#35445);
#1873=PLANE('',#35446);
#1874=PLANE('',#35447);
#1875=PLANE('',#35448);
#1876=PLANE('',#35449);
#1877=PLANE('',#35450);
#1878=PLANE('',#35451);
#1879=PLANE('',#35452);
#1880=PLANE('',#35453);
#1881=PLANE('',#35454);
#1882=PLANE('',#35455);
#1883=PLANE('',#35456);
#1884=PLANE('',#35457);
#1885=PLANE('',#35458);
#1886=PLANE('',#35459);
#1887=PLANE('',#35460);
#1888=PLANE('',#35461);
#1889=PLANE('',#35462);
#1890=PLANE('',#35463);
#1891=PLANE('',#35464);
#1892=PLANE('',#35465);
#1893=PLANE('',#35466);
#1894=PLANE('',#35467);
#1895=PLANE('',#35468);
#1896=PLANE('',#35469);
#1897=PLANE('',#35470);
#1898=PLANE('',#35471);
#1899=PLANE('',#35472);
#1900=PLANE('',#35473);
#1901=PLANE('',#35474);
#1902=PLANE('',#35475);
#1903=PLANE('',#35476);
#1904=PLANE('',#35477);
#1905=PLANE('',#35478);
#1906=PLANE('',#35479);
#1907=PLANE('',#35480);
#1908=PLANE('',#35481);
#1909=PLANE('',#35482);
#1910=PLANE('',#35483);
#1911=PLANE('',#35484);
#1912=PLANE('',#35485);
#1913=PLANE('',#35486);
#1914=PLANE('',#35487);
#1915=PLANE('',#35488);
#1916=PLANE('',#35489);
#1917=PLANE('',#35490);
#1918=PLANE('',#35491);
#1919=PLANE('',#35492);
#1920=PLANE('',#35493);
#1921=PLANE('',#35494);
#1922=PLANE('',#35495);
#1923=PLANE('',#35496);
#1924=PLANE('',#35497);
#1925=PLANE('',#35498);
#1926=PLANE('',#35499);
#1927=PLANE('',#35500);
#1928=PLANE('',#35501);
#1929=PLANE('',#35502);
#1930=PLANE('',#35503);
#1931=PLANE('',#35504);
#1932=PLANE('',#35505);
#1933=PLANE('',#35506);
#1934=PLANE('',#35507);
#1935=PLANE('',#35508);
#1936=PLANE('',#35509);
#1937=PLANE('',#35510);
#1938=PLANE('',#35511);
#1939=PLANE('',#35512);
#1940=PLANE('',#35513);
#1941=PLANE('',#35514);
#1942=PLANE('',#35515);
#1943=PLANE('',#35516);
#1944=PLANE('',#35517);
#1945=PLANE('',#35518);
#1946=PLANE('',#35519);
#1947=PLANE('',#35520);
#1948=PLANE('',#35521);
#1949=PLANE('',#35522);
#1950=PLANE('',#35523);
#1951=PLANE('',#35524);
#1952=PLANE('',#35525);
#1953=PLANE('',#35526);
#1954=PLANE('',#35527);
#1955=PLANE('',#35528);
#1956=PLANE('',#35529);
#1957=PLANE('',#35530);
#1958=PLANE('',#35531);
#1959=PLANE('',#35532);
#1960=PLANE('',#35533);
#1961=PLANE('',#35534);
#1962=PLANE('',#35535);
#1963=PLANE('',#35536);
#1964=PLANE('',#35537);
#1965=PLANE('',#35538);
#1966=PLANE('',#35539);
#1967=PLANE('',#35540);
#1968=PLANE('',#35541);
#1969=PLANE('',#35542);
#1970=PLANE('',#35543);
#1971=PLANE('',#35544);
#1972=PLANE('',#35545);
#1973=PLANE('',#35546);
#1974=PLANE('',#35547);
#1975=PLANE('',#35548);
#1976=PLANE('',#35549);
#1977=PLANE('',#35550);
#1978=PLANE('',#35551);
#1979=PLANE('',#35552);
#1980=PLANE('',#35553);
#1981=PLANE('',#35554);
#1982=PLANE('',#35555);
#1983=PLANE('',#35556);
#1984=PLANE('',#35557);
#1985=PLANE('',#35558);
#1986=PLANE('',#35559);
#1987=PLANE('',#35560);
#1988=PLANE('',#35561);
#1989=PLANE('',#35562);
#1990=PLANE('',#35563);
#1991=PLANE('',#35564);
#1992=PLANE('',#35565);
#1993=PLANE('',#35566);
#1994=PLANE('',#35567);
#1995=PLANE('',#35568);
#1996=PLANE('',#35569);
#1997=PLANE('',#35570);
#1998=PLANE('',#35571);
#1999=PLANE('',#35572);
#2000=PLANE('',#35573);
#2001=PLANE('',#35574);
#2002=PLANE('',#35575);
#2003=PLANE('',#35576);
#2004=PLANE('',#35577);
#2005=PLANE('',#35578);
#2006=PLANE('',#35579);
#2007=PLANE('',#35580);
#2008=PLANE('',#35581);
#2009=PLANE('',#35582);
#2010=PLANE('',#35583);
#2011=PLANE('',#35584);
#2012=PLANE('',#35585);
#2013=PLANE('',#35586);
#2014=PLANE('',#35587);
#2015=PLANE('',#35588);
#2016=PLANE('',#35589);
#2017=PLANE('',#35590);
#2018=PLANE('',#35591);
#2019=PLANE('',#35592);
#2020=PLANE('',#35593);
#2021=PLANE('',#35594);
#2022=PLANE('',#35595);
#2023=PLANE('',#35596);
#2024=PLANE('',#35597);
#2025=PLANE('',#35598);
#2026=PLANE('',#35599);
#2027=PLANE('',#35600);
#2028=PLANE('',#35601);
#2029=PLANE('',#35602);
#2030=PLANE('',#35603);
#2031=PLANE('',#35604);
#2032=PLANE('',#35605);
#2033=PLANE('',#35606);
#2034=PLANE('',#35607);
#2035=PLANE('',#35608);
#2036=PLANE('',#35609);
#2037=PLANE('',#35610);
#2038=PLANE('',#35611);
#2039=PLANE('',#35612);
#2040=PLANE('',#35613);
#2041=PLANE('',#35614);
#2042=PLANE('',#35615);
#2043=PLANE('',#35616);
#2044=PLANE('',#35617);
#2045=PLANE('',#35618);
#2046=PLANE('',#35619);
#2047=PLANE('',#35620);
#2048=PLANE('',#35621);
#2049=PLANE('',#35622);
#2050=PLANE('',#35623);
#2051=PLANE('',#35624);
#2052=PLANE('',#35625);
#2053=PLANE('',#35626);
#2054=PLANE('',#35627);
#2055=PLANE('',#35628);
#2056=PLANE('',#35629);
#2057=PLANE('',#35630);
#2058=PLANE('',#35631);
#2059=PLANE('',#35632);
#2060=PLANE('',#35633);
#2061=PLANE('',#35634);
#2062=PLANE('',#35635);
#2063=PLANE('',#35636);
#2064=PLANE('',#35637);
#2065=PLANE('',#35638);
#2066=PLANE('',#35639);
#2067=PLANE('',#35640);
#2068=PLANE('',#35641);
#2069=PLANE('',#35642);
#2070=PLANE('',#35643);
#2071=PLANE('',#35644);
#2072=PLANE('',#35645);
#2073=PLANE('',#35646);
#2074=PLANE('',#35647);
#2075=PLANE('',#35648);
#2076=PLANE('',#35649);
#2077=PLANE('',#35650);
#2078=PLANE('',#35651);
#2079=PLANE('',#35652);
#2080=PLANE('',#35653);
#2081=PLANE('',#35654);
#2082=PLANE('',#35655);
#2083=PLANE('',#35656);
#2084=PLANE('',#35657);
#2085=PLANE('',#35658);
#2086=PLANE('',#35659);
#2087=PLANE('',#35660);
#2088=PLANE('',#35661);
#2089=PLANE('',#35662);
#2090=PLANE('',#35663);
#2091=PLANE('',#35664);
#2092=PLANE('',#35665);
#2093=PLANE('',#35666);
#2094=PLANE('',#35667);
#2095=PLANE('',#35668);
#2096=PLANE('',#35669);
#2097=PLANE('',#35670);
#2098=PLANE('',#35671);
#2099=PLANE('',#35672);
#2100=PLANE('',#35673);
#2101=PLANE('',#35674);
#2102=PLANE('',#35675);
#2103=PLANE('',#35676);
#2104=PLANE('',#35677);
#2105=PLANE('',#35678);
#2106=PLANE('',#35679);
#2107=PLANE('',#35680);
#2108=PLANE('',#35681);
#2109=PLANE('',#35682);
#2110=PLANE('',#35683);
#2111=PLANE('',#35684);
#2112=PLANE('',#35685);
#2113=PLANE('',#35686);
#2114=PLANE('',#35687);
#2115=PLANE('',#35688);
#2116=PLANE('',#35689);
#2117=PLANE('',#35690);
#2118=PLANE('',#35691);
#2119=PLANE('',#35692);
#2120=PLANE('',#35693);
#2121=PLANE('',#35694);
#2122=PLANE('',#35695);
#2123=PLANE('',#35696);
#2124=PLANE('',#35697);
#2125=PLANE('',#35698);
#2126=PLANE('',#35699);
#2127=PLANE('',#35700);
#2128=PLANE('',#35701);
#2129=PLANE('',#35702);
#2130=PLANE('',#35703);
#2131=PLANE('',#35704);
#2132=PLANE('',#35705);
#2133=PLANE('',#35706);
#2134=PLANE('',#35707);
#2135=PLANE('',#35708);
#2136=PLANE('',#35709);
#2137=PLANE('',#35710);
#2138=PLANE('',#35711);
#2139=PLANE('',#35712);
#2140=PLANE('',#35713);
#2141=PLANE('',#35714);
#2142=PLANE('',#35715);
#2143=PLANE('',#35716);
#2144=PLANE('',#35717);
#2145=PLANE('',#35718);
#2146=PLANE('',#35719);
#2147=PLANE('',#35720);
#2148=PLANE('',#35721);
#2149=PLANE('',#35722);
#2150=PLANE('',#35723);
#2151=PLANE('',#35724);
#2152=PLANE('',#35725);
#2153=PLANE('',#35726);
#2154=PLANE('',#35727);
#2155=PLANE('',#35728);
#2156=PLANE('',#35729);
#2157=PLANE('',#35730);
#2158=PLANE('',#35731);
#2159=PLANE('',#35732);
#2160=PLANE('',#35733);
#2161=PLANE('',#35734);
#2162=PLANE('',#35735);
#2163=PLANE('',#35736);
#2164=PLANE('',#35737);
#2165=PLANE('',#35738);
#2166=PLANE('',#35739);
#2167=PLANE('',#35740);
#2168=PLANE('',#35741);
#2169=PLANE('',#35742);
#2170=PLANE('',#35743);
#2171=PLANE('',#35744);
#2172=PLANE('',#35745);
#2173=PLANE('',#35746);
#2174=PLANE('',#35747);
#2175=PLANE('',#35748);
#2176=PLANE('',#35749);
#2177=PLANE('',#35750);
#2178=PLANE('',#35751);
#2179=PLANE('',#35752);
#2180=PLANE('',#35753);
#2181=PLANE('',#35754);
#2182=PLANE('',#35755);
#2183=PLANE('',#35756);
#2184=PLANE('',#35757);
#2185=PLANE('',#35758);
#2186=PLANE('',#35759);
#2187=PLANE('',#35760);
#2188=PLANE('',#35761);
#2189=PLANE('',#35762);
#2190=PLANE('',#35763);
#2191=PLANE('',#35764);
#2192=PLANE('',#35765);
#2193=PLANE('',#35766);
#2194=PLANE('',#35767);
#2195=PLANE('',#35768);
#2196=PLANE('',#35769);
#2197=PLANE('',#35770);
#2198=PLANE('',#35771);
#2199=PLANE('',#35772);
#2200=PLANE('',#35773);
#2201=PLANE('',#35774);
#2202=PLANE('',#35775);
#2203=PLANE('',#35776);
#2204=PLANE('',#35777);
#2205=PLANE('',#35778);
#2206=PLANE('',#35779);
#2207=PLANE('',#35780);
#2208=PLANE('',#35781);
#2209=PLANE('',#35782);
#2210=PLANE('',#35783);
#2211=PLANE('',#35784);
#2212=PLANE('',#35785);
#2213=PLANE('',#35786);
#2214=PLANE('',#35787);
#2215=PLANE('',#35788);
#2216=PLANE('',#35789);
#2217=PLANE('',#35790);
#2218=PLANE('',#35791);
#2219=PLANE('',#35792);
#2220=PLANE('',#35793);
#2221=PLANE('',#35794);
#2222=PLANE('',#35795);
#2223=PLANE('',#35796);
#2224=PLANE('',#35797);
#2225=PLANE('',#35798);
#2226=PLANE('',#35799);
#2227=PLANE('',#35800);
#2228=PLANE('',#35801);
#2229=PLANE('',#35802);
#2230=PLANE('',#35803);
#2231=PLANE('',#35804);
#2232=PLANE('',#35805);
#2233=PLANE('',#35806);
#2234=PLANE('',#35807);
#2235=PLANE('',#35808);
#2236=PLANE('',#35809);
#2237=PLANE('',#35810);
#2238=PLANE('',#35811);
#2239=PLANE('',#35812);
#2240=PLANE('',#35813);
#2241=PLANE('',#35814);
#2242=PLANE('',#35815);
#2243=PLANE('',#35816);
#2244=PLANE('',#35817);
#2245=PLANE('',#35818);
#2246=PLANE('',#35819);
#2247=PLANE('',#35820);
#2248=PLANE('',#35821);
#2249=PLANE('',#35822);
#2250=PLANE('',#35823);
#2251=PLANE('',#35824);
#2252=PLANE('',#35825);
#2253=PLANE('',#35826);
#2254=PLANE('',#35827);
#2255=PLANE('',#35828);
#2256=PLANE('',#35829);
#2257=PLANE('',#35830);
#2258=PLANE('',#35831);
#2259=PLANE('',#35832);
#2260=PLANE('',#35833);
#2261=PLANE('',#35834);
#2262=PLANE('',#35835);
#2263=PLANE('',#35836);
#2264=PLANE('',#35837);
#2265=PLANE('',#35838);
#2266=PLANE('',#35839);
#2267=PLANE('',#35840);
#2268=PLANE('',#35841);
#2269=PLANE('',#35842);
#2270=PLANE('',#35843);
#2271=PLANE('',#35844);
#2272=PLANE('',#35845);
#2273=PLANE('',#35846);
#2274=PLANE('',#35847);
#2275=PLANE('',#35848);
#2276=PLANE('',#35849);
#2277=PLANE('',#35850);
#2278=PLANE('',#35851);
#2279=PLANE('',#35852);
#2280=PLANE('',#35853);
#2281=PLANE('',#35854);
#2282=PLANE('',#35855);
#2283=PLANE('',#35856);
#2284=PLANE('',#35857);
#2285=PLANE('',#35858);
#2286=PLANE('',#35859);
#2287=PLANE('',#35860);
#2288=PLANE('',#35861);
#2289=PLANE('',#35862);
#2290=PLANE('',#35863);
#2291=PLANE('',#35864);
#2292=PLANE('',#35865);
#2293=PLANE('',#35866);
#2294=PLANE('',#35867);
#2295=PLANE('',#35868);
#2296=PLANE('',#35869);
#2297=PLANE('',#35870);
#2298=PLANE('',#35871);
#2299=PLANE('',#35872);
#2300=PLANE('',#35873);
#2301=PLANE('',#35874);
#2302=PLANE('',#35875);
#2303=PLANE('',#35876);
#2304=PLANE('',#35877);
#2305=PLANE('',#35878);
#2306=PLANE('',#35879);
#2307=PLANE('',#35880);
#2308=PLANE('',#35881);
#2309=PLANE('',#35882);
#2310=PLANE('',#35883);
#2311=PLANE('',#35884);
#2312=PLANE('',#35885);
#2313=PLANE('',#35886);
#2314=PLANE('',#35887);
#2315=PLANE('',#35888);
#2316=PLANE('',#35889);
#2317=PLANE('',#35890);
#2318=PLANE('',#35891);
#2319=PLANE('',#35892);
#2320=PLANE('',#35893);
#2321=PLANE('',#35894);
#2322=PLANE('',#35895);
#2323=PLANE('',#35896);
#2324=PLANE('',#35897);
#2325=PLANE('',#35898);
#2326=PLANE('',#35899);
#2327=PLANE('',#35900);
#2328=PLANE('',#35901);
#2329=PLANE('',#35902);
#2330=PLANE('',#35903);
#2331=PLANE('',#35904);
#2332=PLANE('',#35905);
#2333=PLANE('',#35906);
#2334=PLANE('',#35907);
#2335=PLANE('',#35908);
#2336=PLANE('',#35909);
#2337=PLANE('',#35910);
#2338=PLANE('',#35911);
#2339=PLANE('',#35912);
#2340=PLANE('',#35913);
#2341=PLANE('',#35914);
#2342=PLANE('',#35915);
#2343=PLANE('',#35916);
#2344=PLANE('',#35917);
#2345=PLANE('',#35918);
#2346=PLANE('',#35919);
#2347=PLANE('',#35930);
#2348=PLANE('',#35931);
#2349=PLANE('',#35932);
#2350=PLANE('',#35933);
#2351=PLANE('',#35934);
#2352=PLANE('',#35935);
#2353=PLANE('',#35936);
#2354=PLANE('',#35937);
#2355=PLANE('',#35938);
#2356=PLANE('',#35939);
#2357=PLANE('',#35940);
#2358=PLANE('',#35941);
#2359=PLANE('',#35942);
#2360=PLANE('',#35943);
#2361=PLANE('',#35944);
#2362=PLANE('',#35945);
#2363=PLANE('',#35946);
#2364=PLANE('',#35947);
#2365=PLANE('',#35948);
#2366=PLANE('',#35949);
#2367=PLANE('',#35950);
#2368=PLANE('',#35951);
#2369=PLANE('',#35952);
#2370=PLANE('',#35953);
#2371=PLANE('',#35954);
#2372=PLANE('',#35955);
#2373=PLANE('',#35956);
#2374=PLANE('',#35957);
#2375=PLANE('',#35958);
#2376=PLANE('',#35959);
#2377=PLANE('',#35971);
#2378=PLANE('',#35978);
#2379=PLANE('',#35979);
#2380=PLANE('',#35980);
#2381=PLANE('',#35981);
#2382=PLANE('',#35982);
#2383=PLANE('',#35983);
#2384=PLANE('',#35984);
#2385=PLANE('',#35985);
#2386=PLANE('',#35986);
#2387=PLANE('',#35987);
#2388=PLANE('',#35988);
#2389=PLANE('',#35989);
#2390=PLANE('',#35990);
#2391=PLANE('',#35991);
#2392=PLANE('',#35992);
#2393=PLANE('',#35993);
#2394=PLANE('',#35994);
#2395=PLANE('',#35995);
#2396=PLANE('',#35996);
#2397=PLANE('',#35997);
#2398=PLANE('',#35998);
#2399=PLANE('',#35999);
#2400=PLANE('',#36000);
#2401=PLANE('',#36001);
#2402=PLANE('',#36002);
#2403=PLANE('',#36003);
#2404=PLANE('',#36004);
#2405=PLANE('',#36005);
#2406=PLANE('',#36006);
#2407=PLANE('',#36007);
#2408=PLANE('',#36008);
#2409=PLANE('',#36009);
#2410=PLANE('',#36010);
#2411=PLANE('',#36011);
#2412=PLANE('',#36012);
#2413=PLANE('',#36013);
#2414=PLANE('',#36014);
#2415=PLANE('',#36015);
#2416=PLANE('',#36016);
#2417=PLANE('',#36017);
#2418=PLANE('',#36018);
#2419=PLANE('',#36019);
#2420=PLANE('',#36020);
#2421=PLANE('',#36021);
#2422=PLANE('',#36022);
#2423=PLANE('',#36023);
#2424=PLANE('',#36024);
#2425=PLANE('',#36025);
#2426=PLANE('',#36026);
#2427=PLANE('',#36027);
#2428=PLANE('',#36028);
#2429=PLANE('',#36029);
#2430=PLANE('',#36030);
#2431=PLANE('',#36031);
#2432=PLANE('',#36032);
#2433=PLANE('',#36033);
#2434=PLANE('',#36034);
#2435=PLANE('',#36035);
#2436=PLANE('',#36036);
#2437=PLANE('',#36037);
#2438=PLANE('',#36038);
#2439=PLANE('',#36039);
#2440=PLANE('',#36040);
#2441=PLANE('',#36041);
#2442=PLANE('',#36042);
#2443=PLANE('',#36043);
#2444=PLANE('',#36044);
#2445=PLANE('',#36045);
#2446=PLANE('',#36046);
#2447=PLANE('',#36047);
#2448=PLANE('',#36048);
#2449=PLANE('',#36049);
#2450=PLANE('',#36050);
#2451=PLANE('',#36051);
#2452=PLANE('',#36052);
#2453=PLANE('',#36053);
#2454=PLANE('',#36054);
#2455=PLANE('',#36055);
#2456=PLANE('',#36056);
#2457=PLANE('',#36057);
#2458=PLANE('',#36058);
#2459=PLANE('',#36059);
#2460=PLANE('',#36060);
#2461=PLANE('',#36061);
#2462=PLANE('',#36062);
#2463=PLANE('',#36063);
#2464=PLANE('',#36064);
#2465=PLANE('',#36065);
#2466=PLANE('',#36066);
#2467=PLANE('',#36067);
#2468=PLANE('',#36068);
#2469=PLANE('',#36069);
#2470=PLANE('',#36070);
#2471=PLANE('',#36071);
#2472=PLANE('',#36072);
#2473=PLANE('',#36073);
#2474=PLANE('',#36074);
#2475=PLANE('',#36075);
#2476=PLANE('',#36076);
#2477=PLANE('',#36077);
#2478=PLANE('',#36078);
#2479=PLANE('',#36079);
#2480=PLANE('',#36080);
#2481=PLANE('',#36081);
#2482=PLANE('',#36082);
#2483=PLANE('',#36083);
#2484=PLANE('',#36084);
#2485=PLANE('',#36085);
#2486=PLANE('',#36086);
#2487=PLANE('',#36087);
#2488=PLANE('',#36088);
#2489=PLANE('',#36089);
#2490=PLANE('',#36090);
#2491=PLANE('',#36091);
#2492=PLANE('',#36092);
#2493=PLANE('',#36093);
#2494=PLANE('',#36094);
#2495=PLANE('',#36095);
#2496=PLANE('',#36096);
#2497=PLANE('',#36097);
#2498=PLANE('',#36098);
#2499=PLANE('',#36099);
#2500=PLANE('',#36100);
#2501=PLANE('',#36101);
#2502=PLANE('',#36102);
#2503=PLANE('',#36103);
#2504=PLANE('',#36104);
#2505=PLANE('',#36105);
#2506=PLANE('',#36106);
#2507=PLANE('',#36107);
#2508=PLANE('',#36108);
#2509=PLANE('',#36109);
#2510=PLANE('',#36110);
#2511=PLANE('',#36111);
#2512=PLANE('',#36112);
#2513=PLANE('',#36113);
#2514=PLANE('',#36114);
#2515=PLANE('',#36115);
#2516=PLANE('',#36116);
#2517=PLANE('',#36117);
#2518=PLANE('',#36118);
#2519=PLANE('',#36119);
#2520=PLANE('',#36120);
#2521=PLANE('',#36121);
#2522=PLANE('',#36145);
#2523=PLANE('',#36148);
#2524=PLANE('',#36151);
#2525=PLANE('',#36154);
#2526=PLANE('',#36161);
#2527=PLANE('',#36181);
#2528=PLANE('',#36183);
#2529=PLANE('',#36184);
#2530=PLANE('',#36185);
#2531=PLANE('',#36186);
#2532=PLANE('',#36187);
#2533=PLANE('',#36188);
#2534=PLANE('',#36189);
#2535=PLANE('',#36190);
#2536=PLANE('',#36191);
#2537=PLANE('',#36192);
#2538=PLANE('',#36193);
#2539=PLANE('',#36194);
#2540=PLANE('',#36195);
#2541=PLANE('',#36196);
#2542=PLANE('',#36197);
#2543=PLANE('',#36198);
#2544=PLANE('',#36199);
#2545=PLANE('',#36200);
#2546=PLANE('',#36201);
#2547=PLANE('',#36202);
#2548=PLANE('',#36203);
#2549=PLANE('',#36204);
#2550=PLANE('',#36205);
#2551=PLANE('',#36206);
#2552=PLANE('',#36207);
#2553=PLANE('',#36208);
#2554=PLANE('',#36209);
#2555=PLANE('',#36210);
#2556=PLANE('',#36211);
#2557=PLANE('',#36212);
#2558=PLANE('',#36213);
#2559=PLANE('',#36214);
#2560=PLANE('',#36215);
#2561=PLANE('',#36216);
#2562=PLANE('',#36217);
#2563=PLANE('',#36221);
#2564=PLANE('',#36242);
#2565=PLANE('',#36250);
#2566=PLANE('',#36251);
#2567=PLANE('',#36252);
#2568=PLANE('',#36253);
#2569=PLANE('',#36254);
#2570=PLANE('',#36255);
#2571=PLANE('',#36267);
#2572=PLANE('',#36274);
#2573=PLANE('',#36277);
#2574=PLANE('',#36281);
#2575=PLANE('',#36283);
#2576=PLANE('',#36284);
#2577=PLANE('',#36285);
#2578=PLANE('',#36286);
#2579=PLANE('',#36287);
#2580=PLANE('',#36288);
#2581=PLANE('',#36289);
#2582=PLANE('',#36290);
#2583=PLANE('',#36291);
#2584=PLANE('',#36292);
#2585=PLANE('',#36316);
#2586=PLANE('',#36326);
#2587=PLANE('',#36328);
#2588=PLANE('',#36332);
#2589=PLANE('',#36333);
#2590=PLANE('',#36339);
#2591=PLANE('',#36346);
#2592=PLANE('',#36354);
#2593=PLANE('',#36362);
#2594=PLANE('',#36376);
#2595=PLANE('',#36385);
#2596=PLANE('',#36393);
#2597=PLANE('',#36399);
#2598=PLANE('',#36409);
#2599=PLANE('',#36422);
#2600=PLANE('',#36423);
#2601=PLANE('',#36435);
#2602=PLANE('',#36436);
#2603=PLANE('',#36448);
#2604=PLANE('',#36449);
#2605=PLANE('',#36461);
#2606=PLANE('',#36462);
#2607=PLANE('',#36474);
#2608=PLANE('',#36475);
#2609=PLANE('',#36487);
#2610=PLANE('',#36488);
#2611=PLANE('',#36500);
#2612=PLANE('',#36501);
#2613=PLANE('',#36513);
#2614=PLANE('',#36514);
#2615=PLANE('',#36526);
#2616=PLANE('',#36527);
#2617=PLANE('',#36539);
#2618=PLANE('',#36540);
#2619=PLANE('',#36552);
#2620=PLANE('',#36553);
#2621=PLANE('',#36565);
#2622=PLANE('',#36566);
#2623=PLANE('',#36578);
#2624=PLANE('',#36579);
#2625=PLANE('',#36591);
#2626=PLANE('',#36592);
#2627=PLANE('',#36604);
#2628=PLANE('',#36605);
#2629=PLANE('',#36617);
#2630=PLANE('',#36618);
#2631=PLANE('',#36630);
#2632=PLANE('',#36631);
#2633=PLANE('',#36643);
#2634=PLANE('',#36644);
#2635=PLANE('',#36656);
#2636=PLANE('',#36657);
#2637=PLANE('',#36669);
#2638=PLANE('',#36670);
#2639=PLANE('',#36682);
#2640=PLANE('',#36683);
#2641=PLANE('',#36695);
#2642=PLANE('',#36696);
#2643=PLANE('',#36702);
#2644=PLANE('',#36710);
#2645=PLANE('',#36719);
#2646=PLANE('',#36727);
#2647=PLANE('',#36733);
#2648=PLANE('',#36743);
#2649=PLANE('',#36756);
#2650=PLANE('',#36757);
#2651=PLANE('',#36769);
#2652=PLANE('',#36770);
#2653=PLANE('',#36782);
#2654=PLANE('',#36783);
#2655=PLANE('',#36795);
#2656=PLANE('',#36796);
#2657=PLANE('',#36808);
#2658=PLANE('',#36809);
#2659=PLANE('',#36821);
#2660=PLANE('',#36822);
#2661=PLANE('',#36834);
#2662=PLANE('',#36835);
#2663=PLANE('',#36847);
#2664=PLANE('',#36848);
#2665=PLANE('',#36860);
#2666=PLANE('',#36861);
#2667=PLANE('',#36873);
#2668=PLANE('',#36874);
#2669=PLANE('',#36886);
#2670=PLANE('',#36887);
#2671=PLANE('',#36899);
#2672=PLANE('',#36900);
#2673=PLANE('',#36912);
#2674=PLANE('',#36913);
#2675=PLANE('',#36925);
#2676=PLANE('',#36926);
#2677=PLANE('',#36938);
#2678=PLANE('',#36939);
#2679=PLANE('',#36951);
#2680=PLANE('',#36952);
#2681=PLANE('',#36964);
#2682=PLANE('',#36965);
#2683=PLANE('',#36977);
#2684=PLANE('',#36978);
#2685=PLANE('',#36990);
#2686=PLANE('',#36991);
#2687=PLANE('',#37003);
#2688=PLANE('',#37004);
#2689=PLANE('',#37010);
#2690=PLANE('',#37018);
#2691=PLANE('',#37020);
#2692=PLANE('',#37021);
#2693=PLANE('',#37022);
#2694=PLANE('',#37023);
#2695=PLANE('',#37024);
#2696=PLANE('',#37025);
#2697=PLANE('',#37030);
#2698=PLANE('',#37038);
#2699=PLANE('',#37039);
#2700=PLANE('',#37043);
#2701=PLANE('',#37044);
#2702=PLANE('',#37045);
#2703=PLANE('',#37046);
#2704=PLANE('',#37047);
#2705=PLANE('',#37048);
#2706=PLANE('',#37050);
#2707=PLANE('',#37051);
#2708=PLANE('',#37054);
#2709=PLANE('',#37055);
#2710=PLANE('',#37056);
#2711=PLANE('',#37057);
#2712=PLANE('',#37058);
#2713=PLANE('',#37062);
#2714=PLANE('',#37065);
#2715=PLANE('',#37066);
#2716=PLANE('',#37067);
#2717=PLANE('',#37070);
#2718=PLANE('',#37071);
#2719=PLANE('',#37075);
#2720=PLANE('',#37076);
#2721=PLANE('',#37077);
#2722=PLANE('',#37078);
#2723=PLANE('',#37079);
#2724=PLANE('',#37080);
#2725=PLANE('',#37081);
#2726=PLANE('',#37082);
#2727=PLANE('',#37083);
#2728=PLANE('',#37084);
#2729=PLANE('',#37085);
#2730=PLANE('',#37086);
#2731=PLANE('',#37087);
#2732=PLANE('',#37089);
#2733=PLANE('',#37090);
#2734=PLANE('',#37093);
#2735=PLANE('',#37094);
#2736=PLANE('',#37095);
#2737=PLANE('',#37098);
#2738=PLANE('',#37099);
#2739=PLANE('',#37101);
#2740=PLANE('',#37102);
#2741=PLANE('',#37103);
#2742=PLANE('',#37104);
#2743=PLANE('',#37105);
#2744=PLANE('',#37106);
#2745=PLANE('',#37107);
#2746=PLANE('',#37111);
#2747=PLANE('',#37112);
#2748=PLANE('',#37113);
#2749=PLANE('',#37114);
#2750=PLANE('',#37115);
#2751=PLANE('',#37116);
#2752=PLANE('',#37117);
#2753=PLANE('',#37118);
#2754=PLANE('',#37119);
#2755=PLANE('',#37120);
#2756=PLANE('',#37126);
#2757=PLANE('',#37131);
#2758=PLANE('',#37142);
#2759=PLANE('',#37143);
#2760=PLANE('',#37144);
#2761=PLANE('',#37147);
#2762=PLANE('',#37148);
#2763=PLANE('',#37149);
#2764=PLANE('',#37150);
#2765=PLANE('',#37151);
#2766=PLANE('',#37152);
#2767=PLANE('',#37153);
#2768=PLANE('',#37156);
#2769=PLANE('',#37159);
#2770=PLANE('',#37160);
#2771=PLANE('',#37163);
#2772=PLANE('',#37164);
#2773=PLANE('',#37165);
#2774=PLANE('',#37166);
#2775=PLANE('',#37167);
#2776=PLANE('',#37168);
#2777=PLANE('',#37169);
#2778=PLANE('',#37170);
#2779=PLANE('',#37175);
#2780=PLANE('',#37176);
#2781=PLANE('',#37177);
#2782=PLANE('',#37178);
#2783=PLANE('',#37179);
#2784=PLANE('',#37180);
#2785=PLANE('',#37181);
#2786=PLANE('',#37182);
#2787=PLANE('',#37183);
#2788=PLANE('',#37184);
#2789=PLANE('',#37196);
#2790=PLANE('',#37199);
#2791=PLANE('',#37200);
#2792=PLANE('',#37201);
#2793=PLANE('',#37202);
#2794=PLANE('',#37203);
#2795=PLANE('',#37204);
#2796=PLANE('',#37205);
#2797=PLANE('',#37206);
#2798=PLANE('',#37209);
#2799=PLANE('',#37210);
#2800=PLANE('',#37214);
#2801=PLANE('',#37243);
#2802=PLANE('',#37250);
#2803=PLANE('',#37255);
#2804=PLANE('',#37256);
#2805=PLANE('',#37339);
#2806=PLANE('',#37340);
#2807=PLANE('',#37341);
#2808=PLANE('',#37344);
#2809=PLANE('',#37350);
#2810=PLANE('',#37351);
#2811=PLANE('',#37352);
#2812=PLANE('',#37353);
#2813=PLANE('',#37355);
#2814=PLANE('',#37356);
#2815=PLANE('',#37362);
#2816=PLANE('',#37363);
#2817=PLANE('',#37365);
#2818=PLANE('',#37366);
#2819=PLANE('',#37368);
#2820=PLANE('',#37369);
#2821=PLANE('',#37371);
#2822=PLANE('',#37372);
#2823=PLANE('',#37374);
#2824=PLANE('',#37375);
#2825=PLANE('',#37377);
#2826=PLANE('',#37378);
#2827=PLANE('',#37380);
#2828=PLANE('',#37381);
#2829=PLANE('',#37383);
#2830=PLANE('',#37384);
#2831=PLANE('',#37386);
#2832=PLANE('',#37387);
#2833=PLANE('',#37389);
#2834=PLANE('',#37390);
#2835=PLANE('',#37392);
#2836=PLANE('',#37393);
#2837=PLANE('',#37395);
#2838=PLANE('',#37396);
#2839=PLANE('',#37398);
#2840=PLANE('',#37399);
#2841=PLANE('',#37401);
#2842=PLANE('',#37402);
#2843=PLANE('',#37404);
#2844=PLANE('',#37405);
#2845=PLANE('',#37407);
#2846=PLANE('',#37408);
#2847=PLANE('',#37410);
#2848=PLANE('',#37411);
#2849=PLANE('',#37413);
#2850=PLANE('',#37414);
#2851=PLANE('',#37416);
#2852=PLANE('',#37417);
#2853=PLANE('',#37419);
#2854=PLANE('',#37420);
#2855=PLANE('',#37422);
#2856=PLANE('',#37423);
#2857=PLANE('',#37425);
#2858=PLANE('',#37426);
#2859=PLANE('',#37428);
#2860=PLANE('',#37429);
#2861=PLANE('',#37431);
#2862=PLANE('',#37432);
#2863=PLANE('',#37434);
#2864=PLANE('',#37435);
#2865=PLANE('',#37437);
#2866=PLANE('',#37438);
#2867=PLANE('',#37440);
#2868=PLANE('',#37441);
#2869=PLANE('',#37443);
#2870=PLANE('',#37444);
#2871=PLANE('',#37446);
#2872=PLANE('',#37447);
#2873=PLANE('',#37449);
#2874=PLANE('',#37450);
#2875=PLANE('',#37452);
#2876=PLANE('',#37453);
#2877=PLANE('',#37455);
#2878=PLANE('',#37456);
#2879=PLANE('',#37458);
#2880=PLANE('',#37459);
#2881=PLANE('',#37461);
#2882=PLANE('',#37462);
#2883=PLANE('',#37464);
#2884=PLANE('',#37465);
#2885=PLANE('',#37468);
#2886=PLANE('',#37469);
#2887=PLANE('',#37472);
#2888=PLANE('',#37473);
#2889=PLANE('',#37475);
#2890=PLANE('',#37476);
#2891=PLANE('',#37478);
#2892=PLANE('',#37479);
#2893=PLANE('',#37481);
#2894=PLANE('',#37482);
#2895=PLANE('',#37484);
#2896=PLANE('',#37485);
#2897=PLANE('',#37487);
#2898=PLANE('',#37488);
#2899=PLANE('',#37490);
#2900=PLANE('',#37491);
#2901=PLANE('',#37493);
#2902=PLANE('',#37494);
#2903=PLANE('',#37496);
#2904=PLANE('',#37497);
#2905=PLANE('',#37499);
#2906=PLANE('',#37500);
#2907=PLANE('',#37502);
#2908=PLANE('',#37503);
#2909=PLANE('',#37505);
#2910=PLANE('',#37506);
#2911=PLANE('',#37508);
#2912=PLANE('',#37509);
#2913=PLANE('',#37511);
#2914=PLANE('',#37512);
#2915=PLANE('',#37514);
#2916=PLANE('',#37515);
#2917=PLANE('',#37517);
#2918=PLANE('',#37518);
#2919=PLANE('',#37520);
#2920=PLANE('',#37521);
#2921=PLANE('',#37523);
#2922=PLANE('',#37524);
#2923=PLANE('',#37526);
#2924=PLANE('',#37527);
#2925=PLANE('',#37529);
#2926=PLANE('',#37530);
#2927=PLANE('',#37532);
#2928=PLANE('',#37533);
#2929=PLANE('',#37535);
#2930=PLANE('',#37536);
#2931=PLANE('',#37538);
#2932=PLANE('',#37539);
#2933=PLANE('',#37541);
#2934=PLANE('',#37542);
#2935=PLANE('',#37544);
#2936=PLANE('',#37545);
#2937=PLANE('',#37547);
#2938=PLANE('',#37548);
#2939=PLANE('',#37550);
#2940=PLANE('',#37551);
#2941=PLANE('',#37553);
#2942=PLANE('',#37554);
#2943=PLANE('',#37556);
#2944=PLANE('',#37557);
#2945=PLANE('',#37559);
#2946=PLANE('',#37560);
#2947=PLANE('',#37562);
#2948=PLANE('',#37563);
#2949=PLANE('',#37565);
#2950=PLANE('',#37566);
#2951=PLANE('',#37568);
#2952=PLANE('',#37569);
#2953=PLANE('',#37571);
#2954=PLANE('',#37572);
#2955=PLANE('',#37574);
#2956=PLANE('',#37575);
#2957=PLANE('',#37577);
#2958=PLANE('',#37578);
#2959=PLANE('',#37598);
#2960=PLANE('',#37600);
#2961=PLANE('',#37601);
#2962=PLANE('',#37602);
#2963=PLANE('',#37603);
#2964=PLANE('',#37604);
#2965=PLANE('',#37605);
#2966=PLANE('',#37606);
#2967=PLANE('',#37607);
#2968=PLANE('',#37608);
#2969=PLANE('',#37609);
#2970=PLANE('',#37610);
#2971=PLANE('',#37611);
#2972=PLANE('',#37612);
#2973=PLANE('',#37613);
#2974=PLANE('',#37614);
#2975=PLANE('',#37615);
#2976=PLANE('',#37616);
#2977=PLANE('',#37617);
#2978=PLANE('',#37618);
#2979=PLANE('',#37619);
#2980=PLANE('',#37620);
#2981=PLANE('',#37621);
#2982=PLANE('',#37622);
#2983=PLANE('',#37623);
#2984=PLANE('',#37624);
#2985=PLANE('',#37625);
#2986=PLANE('',#37627);
#2987=PLANE('',#37628);
#2988=PLANE('',#37629);
#2989=PLANE('',#37630);
#2990=PLANE('',#37631);
#2991=PLANE('',#37637);
#2992=CYLINDRICAL_SURFACE('',#34375,40.);
#2993=CYLINDRICAL_SURFACE('',#34385,26.);
#2994=CYLINDRICAL_SURFACE('',#34428,136.);
#2995=CYLINDRICAL_SURFACE('',#34894,15.);
#2996=CYLINDRICAL_SURFACE('',#34896,52.);
#2997=CYLINDRICAL_SURFACE('',#34898,15.);
#2998=CYLINDRICAL_SURFACE('',#34900,52.);
#2999=CYLINDRICAL_SURFACE('',#34902,15.);
#3000=CYLINDRICAL_SURFACE('',#34904,52.);
#3001=CYLINDRICAL_SURFACE('',#35928,127.);
#3002=CYLINDRICAL_SURFACE('',#35965,139.);
#3003=CYLINDRICAL_SURFACE('',#36122,7.18);
#3004=CYLINDRICAL_SURFACE('',#36124,7.18);
#3005=CYLINDRICAL_SURFACE('',#36126,7.18);
#3006=CYLINDRICAL_SURFACE('',#36128,7.18);
#3007=CYLINDRICAL_SURFACE('',#36130,7.18);
#3008=CYLINDRICAL_SURFACE('',#36135,23.);
#3009=CYLINDRICAL_SURFACE('',#36137,15.);
#3010=CYLINDRICAL_SURFACE('',#36139,52.);
#3011=CYLINDRICAL_SURFACE('',#36141,15.);
#3012=CYLINDRICAL_SURFACE('',#36143,52.);
#3013=CYLINDRICAL_SURFACE('',#36146,25.16);
#3014=CYLINDRICAL_SURFACE('',#36149,27.);
#3015=CYLINDRICAL_SURFACE('',#36152,29.58);
#3016=CYLINDRICAL_SURFACE('',#36156,32.6);
#3017=CYLINDRICAL_SURFACE('',#36167,11.59764);
#3018=CYLINDRICAL_SURFACE('',#36168,11.59764);
#3019=CYLINDRICAL_SURFACE('',#36169,11.59764);
#3020=CYLINDRICAL_SURFACE('',#36170,11.59764);
#3021=CYLINDRICAL_SURFACE('',#36171,11.59764);
#3022=CYLINDRICAL_SURFACE('',#36172,11.59764);
#3023=CYLINDRICAL_SURFACE('',#36173,11.59764);
#3024=CYLINDRICAL_SURFACE('',#36175,11.59764);
#3025=CYLINDRICAL_SURFACE('',#36176,11.59764);
#3026=CYLINDRICAL_SURFACE('',#36226,6.75);
#3027=CYLINDRICAL_SURFACE('',#36230,6.75);
#3028=CYLINDRICAL_SURFACE('',#36234,6.75);
#3029=CYLINDRICAL_SURFACE('',#36238,6.75);
#3030=CYLINDRICAL_SURFACE('',#36264,25.4);
#3031=CYLINDRICAL_SURFACE('',#36268,11.59764);
#3032=CYLINDRICAL_SURFACE('',#36269,11.59764);
#3033=CYLINDRICAL_SURFACE('',#36271,11.59764);
#3034=CYLINDRICAL_SURFACE('',#36272,11.59764);
#3035=CYLINDRICAL_SURFACE('',#36273,11.59764);
#3036=CYLINDRICAL_SURFACE('',#36294,12.61364);
#3037=CYLINDRICAL_SURFACE('',#36295,12.61364);
#3038=CYLINDRICAL_SURFACE('',#36296,12.61364);
#3039=CYLINDRICAL_SURFACE('',#36297,12.61364);
#3040=CYLINDRICAL_SURFACE('',#36299,12.61364);
#3041=CYLINDRICAL_SURFACE('',#36301,12.61364);
#3042=CYLINDRICAL_SURFACE('',#36302,12.61364);
#3043=CYLINDRICAL_SURFACE('',#36303,12.61364);
#3044=CYLINDRICAL_SURFACE('',#36304,12.61364);
#3045=CYLINDRICAL_SURFACE('',#36305,12.61364);
#3046=CYLINDRICAL_SURFACE('',#36306,12.61364);
#3047=CYLINDRICAL_SURFACE('',#36307,12.61364);
#3048=CYLINDRICAL_SURFACE('',#36309,12.61364);
#3049=CYLINDRICAL_SURFACE('',#36310,12.61364);
#3050=CYLINDRICAL_SURFACE('',#36311,2.20000000000001);
#3051=CYLINDRICAL_SURFACE('',#36314,21.8313);
#3052=CYLINDRICAL_SURFACE('',#36320,17.47);
#3053=CYLINDRICAL_SURFACE('',#36329,13.47);
#3054=CYLINDRICAL_SURFACE('',#36335,11.9);
#3055=CYLINDRICAL_SURFACE('',#36340,12.61364);
#3056=CYLINDRICAL_SURFACE('',#36348,24.5);
#3057=CYLINDRICAL_SURFACE('',#36356,29.4);
#3058=CYLINDRICAL_SURFACE('',#36366,32.585);
#3059=CYLINDRICAL_SURFACE('',#36373,21.8413);
#3060=CYLINDRICAL_SURFACE('',#36381,29.5655);
#3061=CYLINDRICAL_SURFACE('',#36401,25.8846416389917);
#3062=CYLINDRICAL_SURFACE('',#36407,22.7743990607509);
#3063=CYLINDRICAL_SURFACE('',#36706,17.494);
#3064=CYLINDRICAL_SURFACE('',#36715,25.146);
#3065=CYLINDRICAL_SURFACE('',#36735,21.6856897166516);
#3066=CYLINDRICAL_SURFACE('',#36741,18.818471118769);
#3067=CYLINDRICAL_SURFACE('',#37014,13.494);
#3068=CYLINDRICAL_SURFACE('',#37028,13.6);
#3069=CYLINDRICAL_SURFACE('',#37034,20.5);
#3070=CYLINDRICAL_SURFACE('',#37132,12.75);
#3071=CYLINDRICAL_SURFACE('',#37190,1.95);
#3072=CYLINDRICAL_SURFACE('',#37241,25.6);
#3073=CYLINDRICAL_SURFACE('',#37248,25.12);
#3074=CYLINDRICAL_SURFACE('',#37252,26.8);
#3075=CYLINDRICAL_SURFACE('',#37268,24.32);
#3076=CYLINDRICAL_SURFACE('',#37270,6.28269);
#3077=CYLINDRICAL_SURFACE('',#37272,6.28269);
#3078=CYLINDRICAL_SURFACE('',#37273,6.28269);
#3079=CYLINDRICAL_SURFACE('',#37274,6.28269);
#3080=CYLINDRICAL_SURFACE('',#37275,6.28269);
#3081=CYLINDRICAL_SURFACE('',#37276,6.28269);
#3082=CYLINDRICAL_SURFACE('',#37277,6.28269);
#3083=CYLINDRICAL_SURFACE('',#37278,6.28269);
#3084=CYLINDRICAL_SURFACE('',#37279,6.28269);
#3085=CYLINDRICAL_SURFACE('',#37280,6.28269);
#3086=CYLINDRICAL_SURFACE('',#37281,6.28269);
#3087=CYLINDRICAL_SURFACE('',#37282,6.28269);
#3088=CYLINDRICAL_SURFACE('',#37283,6.28269);
#3089=CYLINDRICAL_SURFACE('',#37284,6.28269);
#3090=CYLINDRICAL_SURFACE('',#37285,6.28269);
#3091=CYLINDRICAL_SURFACE('',#37286,6.28269);
#3092=CYLINDRICAL_SURFACE('',#37287,6.28269);
#3093=CYLINDRICAL_SURFACE('',#37288,6.28269);
#3094=CYLINDRICAL_SURFACE('',#37289,6.28269);
#3095=CYLINDRICAL_SURFACE('',#37290,6.28269);
#3096=CYLINDRICAL_SURFACE('',#37291,6.28269);
#3097=CYLINDRICAL_SURFACE('',#37292,6.28269);
#3098=CYLINDRICAL_SURFACE('',#37293,6.28269);
#3099=CYLINDRICAL_SURFACE('',#37294,6.28269);
#3100=CYLINDRICAL_SURFACE('',#37295,6.28269);
#3101=CYLINDRICAL_SURFACE('',#37296,6.28269);
#3102=CYLINDRICAL_SURFACE('',#37297,6.28269);
#3103=CYLINDRICAL_SURFACE('',#37298,6.28269);
#3104=CYLINDRICAL_SURFACE('',#37299,6.28269);
#3105=CYLINDRICAL_SURFACE('',#37300,5.57784);
#3106=CYLINDRICAL_SURFACE('',#37302,5.57784);
#3107=CYLINDRICAL_SURFACE('',#37304,5.57784);
#3108=CYLINDRICAL_SURFACE('',#37305,5.57784);
#3109=CYLINDRICAL_SURFACE('',#37306,5.57784);
#3110=CYLINDRICAL_SURFACE('',#37307,5.57784);
#3111=CYLINDRICAL_SURFACE('',#37308,5.57784);
#3112=CYLINDRICAL_SURFACE('',#37309,5.57784);
#3113=CYLINDRICAL_SURFACE('',#37310,5.57784);
#3114=CYLINDRICAL_SURFACE('',#37311,5.57784);
#3115=CYLINDRICAL_SURFACE('',#37312,5.57784);
#3116=CYLINDRICAL_SURFACE('',#37313,5.57784);
#3117=CYLINDRICAL_SURFACE('',#37314,5.57784);
#3118=CYLINDRICAL_SURFACE('',#37315,5.57784);
#3119=CYLINDRICAL_SURFACE('',#37316,5.57784);
#3120=CYLINDRICAL_SURFACE('',#37317,5.57784);
#3121=CYLINDRICAL_SURFACE('',#37318,5.57784);
#3122=CYLINDRICAL_SURFACE('',#37319,5.57784);
#3123=CYLINDRICAL_SURFACE('',#37320,5.57784);
#3124=CYLINDRICAL_SURFACE('',#37321,5.57784);
#3125=CYLINDRICAL_SURFACE('',#37322,5.57784);
#3126=CYLINDRICAL_SURFACE('',#37323,5.57784);
#3127=CYLINDRICAL_SURFACE('',#37324,5.57784);
#3128=CYLINDRICAL_SURFACE('',#37325,5.57784);
#3129=CYLINDRICAL_SURFACE('',#37326,5.57784);
#3130=CYLINDRICAL_SURFACE('',#37327,5.57784);
#3131=CYLINDRICAL_SURFACE('',#37328,5.57784);
#3132=CYLINDRICAL_SURFACE('',#37329,5.57784);
#3133=CYLINDRICAL_SURFACE('',#37330,5.57784);
#3134=CYLINDRICAL_SURFACE('',#37345,11.);
#3135=CYLINDRICAL_SURFACE('',#37360,5.57784);
#3136=CYLINDRICAL_SURFACE('',#37361,6.28269);
#3137=CYLINDRICAL_SURFACE('',#37580,7.17);
#3138=CYLINDRICAL_SURFACE('',#37639,6.4);
#3139=FACE_OUTER_BOUND('',#5234,.T.);
#3140=FACE_OUTER_BOUND('',#5235,.T.);
#3141=FACE_OUTER_BOUND('',#5236,.T.);
#3142=FACE_OUTER_BOUND('',#5237,.T.);
#3143=FACE_OUTER_BOUND('',#5238,.T.);
#3144=FACE_OUTER_BOUND('',#5240,.T.);
#3145=FACE_OUTER_BOUND('',#5241,.T.);
#3146=FACE_OUTER_BOUND('',#5242,.T.);
#3147=FACE_OUTER_BOUND('',#5244,.T.);
#3148=FACE_OUTER_BOUND('',#5245,.T.);
#3149=FACE_OUTER_BOUND('',#5246,.T.);
#3150=FACE_OUTER_BOUND('',#5248,.T.);
#3151=FACE_OUTER_BOUND('',#5249,.T.);
#3152=FACE_OUTER_BOUND('',#5250,.T.);
#3153=FACE_OUTER_BOUND('',#5251,.T.);
#3154=FACE_OUTER_BOUND('',#5252,.T.);
#3155=FACE_OUTER_BOUND('',#5253,.T.);
#3156=FACE_OUTER_BOUND('',#5254,.T.);
#3157=FACE_OUTER_BOUND('',#5255,.T.);
#3158=FACE_OUTER_BOUND('',#5256,.T.);
#3159=FACE_OUTER_BOUND('',#5257,.T.);
#3160=FACE_OUTER_BOUND('',#5258,.T.);
#3161=FACE_OUTER_BOUND('',#5330,.T.);
#3162=FACE_OUTER_BOUND('',#5331,.T.);
#3163=FACE_OUTER_BOUND('',#5332,.T.);
#3164=FACE_OUTER_BOUND('',#5333,.T.);
#3165=FACE_OUTER_BOUND('',#5334,.T.);
#3166=FACE_OUTER_BOUND('',#5335,.T.);
#3167=FACE_OUTER_BOUND('',#5336,.T.);
#3168=FACE_OUTER_BOUND('',#5337,.T.);
#3169=FACE_OUTER_BOUND('',#5338,.T.);
#3170=FACE_OUTER_BOUND('',#5339,.T.);
#3171=FACE_OUTER_BOUND('',#5340,.T.);
#3172=FACE_OUTER_BOUND('',#5341,.T.);
#3173=FACE_OUTER_BOUND('',#5342,.T.);
#3174=FACE_OUTER_BOUND('',#5343,.T.);
#3175=FACE_OUTER_BOUND('',#5344,.T.);
#3176=FACE_OUTER_BOUND('',#5345,.T.);
#3177=FACE_OUTER_BOUND('',#5346,.T.);
#3178=FACE_OUTER_BOUND('',#5353,.T.);
#3179=FACE_OUTER_BOUND('',#5354,.T.);
#3180=FACE_OUTER_BOUND('',#5355,.T.);
#3181=FACE_OUTER_BOUND('',#5356,.T.);
#3182=FACE_OUTER_BOUND('',#5357,.T.);
#3183=FACE_OUTER_BOUND('',#5358,.T.);
#3184=FACE_OUTER_BOUND('',#5359,.T.);
#3185=FACE_OUTER_BOUND('',#5360,.T.);
#3186=FACE_OUTER_BOUND('',#5361,.T.);
#3187=FACE_OUTER_BOUND('',#5362,.T.);
#3188=FACE_OUTER_BOUND('',#5363,.T.);
#3189=FACE_OUTER_BOUND('',#5364,.T.);
#3190=FACE_OUTER_BOUND('',#5365,.T.);
#3191=FACE_OUTER_BOUND('',#5366,.T.);
#3192=FACE_OUTER_BOUND('',#5367,.T.);
#3193=FACE_OUTER_BOUND('',#5368,.T.);
#3194=FACE_OUTER_BOUND('',#5369,.T.);
#3195=FACE_OUTER_BOUND('',#5370,.T.);
#3196=FACE_OUTER_BOUND('',#5371,.T.);
#3197=FACE_OUTER_BOUND('',#5372,.T.);
#3198=FACE_OUTER_BOUND('',#5373,.T.);
#3199=FACE_OUTER_BOUND('',#5374,.T.);
#3200=FACE_OUTER_BOUND('',#5375,.T.);
#3201=FACE_OUTER_BOUND('',#5376,.T.);
#3202=FACE_OUTER_BOUND('',#5377,.T.);
#3203=FACE_OUTER_BOUND('',#5378,.T.);
#3204=FACE_OUTER_BOUND('',#5379,.T.);
#3205=FACE_OUTER_BOUND('',#5380,.T.);
#3206=FACE_OUTER_BOUND('',#5381,.T.);
#3207=FACE_OUTER_BOUND('',#5382,.T.);
#3208=FACE_OUTER_BOUND('',#5383,.T.);
#3209=FACE_OUTER_BOUND('',#5384,.T.);
#3210=FACE_OUTER_BOUND('',#5385,.T.);
#3211=FACE_OUTER_BOUND('',#5386,.T.);
#3212=FACE_OUTER_BOUND('',#5387,.T.);
#3213=FACE_OUTER_BOUND('',#5388,.T.);
#3214=FACE_OUTER_BOUND('',#5389,.T.);
#3215=FACE_OUTER_BOUND('',#5390,.T.);
#3216=FACE_OUTER_BOUND('',#5391,.T.);
#3217=FACE_OUTER_BOUND('',#5392,.T.);
#3218=FACE_OUTER_BOUND('',#5393,.T.);
#3219=FACE_OUTER_BOUND('',#5394,.T.);
#3220=FACE_OUTER_BOUND('',#5395,.T.);
#3221=FACE_OUTER_BOUND('',#5396,.T.);
#3222=FACE_OUTER_BOUND('',#5397,.T.);
#3223=FACE_OUTER_BOUND('',#5398,.T.);
#3224=FACE_OUTER_BOUND('',#5399,.T.);
#3225=FACE_OUTER_BOUND('',#5400,.T.);
#3226=FACE_OUTER_BOUND('',#5401,.T.);
#3227=FACE_OUTER_BOUND('',#5402,.T.);
#3228=FACE_OUTER_BOUND('',#5403,.T.);
#3229=FACE_OUTER_BOUND('',#5404,.T.);
#3230=FACE_OUTER_BOUND('',#5405,.T.);
#3231=FACE_OUTER_BOUND('',#5406,.T.);
#3232=FACE_OUTER_BOUND('',#5407,.T.);
#3233=FACE_OUTER_BOUND('',#5408,.T.);
#3234=FACE_OUTER_BOUND('',#5409,.T.);
#3235=FACE_OUTER_BOUND('',#5410,.T.);
#3236=FACE_OUTER_BOUND('',#5411,.T.);
#3237=FACE_OUTER_BOUND('',#5412,.T.);
#3238=FACE_OUTER_BOUND('',#5413,.T.);
#3239=FACE_OUTER_BOUND('',#5414,.T.);
#3240=FACE_OUTER_BOUND('',#5415,.T.);
#3241=FACE_OUTER_BOUND('',#5416,.T.);
#3242=FACE_OUTER_BOUND('',#5417,.T.);
#3243=FACE_OUTER_BOUND('',#5418,.T.);
#3244=FACE_OUTER_BOUND('',#5419,.T.);
#3245=FACE_OUTER_BOUND('',#5420,.T.);
#3246=FACE_OUTER_BOUND('',#5421,.T.);
#3247=FACE_OUTER_BOUND('',#5422,.T.);
#3248=FACE_OUTER_BOUND('',#5423,.T.);
#3249=FACE_OUTER_BOUND('',#5424,.T.);
#3250=FACE_OUTER_BOUND('',#5425,.T.);
#3251=FACE_OUTER_BOUND('',#5426,.T.);
#3252=FACE_OUTER_BOUND('',#5427,.T.);
#3253=FACE_OUTER_BOUND('',#5428,.T.);
#3254=FACE_OUTER_BOUND('',#5429,.T.);
#3255=FACE_OUTER_BOUND('',#5430,.T.);
#3256=FACE_OUTER_BOUND('',#5431,.T.);
#3257=FACE_OUTER_BOUND('',#5432,.T.);
#3258=FACE_OUTER_BOUND('',#5433,.T.);
#3259=FACE_OUTER_BOUND('',#5434,.T.);
#3260=FACE_OUTER_BOUND('',#5435,.T.);
#3261=FACE_OUTER_BOUND('',#5436,.T.);
#3262=FACE_OUTER_BOUND('',#5437,.T.);
#3263=FACE_OUTER_BOUND('',#5438,.T.);
#3264=FACE_OUTER_BOUND('',#5439,.T.);
#3265=FACE_OUTER_BOUND('',#5440,.T.);
#3266=FACE_OUTER_BOUND('',#5441,.T.);
#3267=FACE_OUTER_BOUND('',#5442,.T.);
#3268=FACE_OUTER_BOUND('',#5443,.T.);
#3269=FACE_OUTER_BOUND('',#5444,.T.);
#3270=FACE_OUTER_BOUND('',#5445,.T.);
#3271=FACE_OUTER_BOUND('',#5446,.T.);
#3272=FACE_OUTER_BOUND('',#5447,.T.);
#3273=FACE_OUTER_BOUND('',#5448,.T.);
#3274=FACE_OUTER_BOUND('',#5449,.T.);
#3275=FACE_OUTER_BOUND('',#5450,.T.);
#3276=FACE_OUTER_BOUND('',#5451,.T.);
#3277=FACE_OUTER_BOUND('',#5452,.T.);
#3278=FACE_OUTER_BOUND('',#5453,.T.);
#3279=FACE_OUTER_BOUND('',#5454,.T.);
#3280=FACE_OUTER_BOUND('',#5455,.T.);
#3281=FACE_OUTER_BOUND('',#5456,.T.);
#3282=FACE_OUTER_BOUND('',#5457,.T.);
#3283=FACE_OUTER_BOUND('',#5458,.T.);
#3284=FACE_OUTER_BOUND('',#5459,.T.);
#3285=FACE_OUTER_BOUND('',#5460,.T.);
#3286=FACE_OUTER_BOUND('',#5461,.T.);
#3287=FACE_OUTER_BOUND('',#5462,.T.);
#3288=FACE_OUTER_BOUND('',#5463,.T.);
#3289=FACE_OUTER_BOUND('',#5464,.T.);
#3290=FACE_OUTER_BOUND('',#5465,.T.);
#3291=FACE_OUTER_BOUND('',#5466,.T.);
#3292=FACE_OUTER_BOUND('',#5467,.T.);
#3293=FACE_OUTER_BOUND('',#5468,.T.);
#3294=FACE_OUTER_BOUND('',#5469,.T.);
#3295=FACE_OUTER_BOUND('',#5470,.T.);
#3296=FACE_OUTER_BOUND('',#5471,.T.);
#3297=FACE_OUTER_BOUND('',#5472,.T.);
#3298=FACE_OUTER_BOUND('',#5473,.T.);
#3299=FACE_OUTER_BOUND('',#5474,.T.);
#3300=FACE_OUTER_BOUND('',#5475,.T.);
#3301=FACE_OUTER_BOUND('',#5476,.T.);
#3302=FACE_OUTER_BOUND('',#5477,.T.);
#3303=FACE_OUTER_BOUND('',#5478,.T.);
#3304=FACE_OUTER_BOUND('',#5479,.T.);
#3305=FACE_OUTER_BOUND('',#5480,.T.);
#3306=FACE_OUTER_BOUND('',#5481,.T.);
#3307=FACE_OUTER_BOUND('',#5482,.T.);
#3308=FACE_OUTER_BOUND('',#5483,.T.);
#3309=FACE_OUTER_BOUND('',#5484,.T.);
#3310=FACE_OUTER_BOUND('',#5485,.T.);
#3311=FACE_OUTER_BOUND('',#5486,.T.);
#3312=FACE_OUTER_BOUND('',#5487,.T.);
#3313=FACE_OUTER_BOUND('',#5488,.T.);
#3314=FACE_OUTER_BOUND('',#5489,.T.);
#3315=FACE_OUTER_BOUND('',#5490,.T.);
#3316=FACE_OUTER_BOUND('',#5491,.T.);
#3317=FACE_OUTER_BOUND('',#5492,.T.);
#3318=FACE_OUTER_BOUND('',#5493,.T.);
#3319=FACE_OUTER_BOUND('',#5494,.T.);
#3320=FACE_OUTER_BOUND('',#5495,.T.);
#3321=FACE_OUTER_BOUND('',#5496,.T.);
#3322=FACE_OUTER_BOUND('',#5497,.T.);
#3323=FACE_OUTER_BOUND('',#5498,.T.);
#3324=FACE_OUTER_BOUND('',#5499,.T.);
#3325=FACE_OUTER_BOUND('',#5500,.T.);
#3326=FACE_OUTER_BOUND('',#5501,.T.);
#3327=FACE_OUTER_BOUND('',#5502,.T.);
#3328=FACE_OUTER_BOUND('',#5503,.T.);
#3329=FACE_OUTER_BOUND('',#5504,.T.);
#3330=FACE_OUTER_BOUND('',#5505,.T.);
#3331=FACE_OUTER_BOUND('',#5506,.T.);
#3332=FACE_OUTER_BOUND('',#5507,.T.);
#3333=FACE_OUTER_BOUND('',#5508,.T.);
#3334=FACE_OUTER_BOUND('',#5509,.T.);
#3335=FACE_OUTER_BOUND('',#5510,.T.);
#3336=FACE_OUTER_BOUND('',#5511,.T.);
#3337=FACE_OUTER_BOUND('',#5512,.T.);
#3338=FACE_OUTER_BOUND('',#5513,.T.);
#3339=FACE_OUTER_BOUND('',#5514,.T.);
#3340=FACE_OUTER_BOUND('',#5515,.T.);
#3341=FACE_OUTER_BOUND('',#5516,.T.);
#3342=FACE_OUTER_BOUND('',#5517,.T.);
#3343=FACE_OUTER_BOUND('',#5518,.T.);
#3344=FACE_OUTER_BOUND('',#5519,.T.);
#3345=FACE_OUTER_BOUND('',#5520,.T.);
#3346=FACE_OUTER_BOUND('',#5521,.T.);
#3347=FACE_OUTER_BOUND('',#5522,.T.);
#3348=FACE_OUTER_BOUND('',#5523,.T.);
#3349=FACE_OUTER_BOUND('',#5524,.T.);
#3350=FACE_OUTER_BOUND('',#5525,.T.);
#3351=FACE_OUTER_BOUND('',#5526,.T.);
#3352=FACE_OUTER_BOUND('',#5527,.T.);
#3353=FACE_OUTER_BOUND('',#5528,.T.);
#3354=FACE_OUTER_BOUND('',#5529,.T.);
#3355=FACE_OUTER_BOUND('',#5530,.T.);
#3356=FACE_OUTER_BOUND('',#5531,.T.);
#3357=FACE_OUTER_BOUND('',#5532,.T.);
#3358=FACE_OUTER_BOUND('',#5533,.T.);
#3359=FACE_OUTER_BOUND('',#5534,.T.);
#3360=FACE_OUTER_BOUND('',#5535,.T.);
#3361=FACE_OUTER_BOUND('',#5536,.T.);
#3362=FACE_OUTER_BOUND('',#5537,.T.);
#3363=FACE_OUTER_BOUND('',#5538,.T.);
#3364=FACE_OUTER_BOUND('',#5539,.T.);
#3365=FACE_OUTER_BOUND('',#5540,.T.);
#3366=FACE_OUTER_BOUND('',#5541,.T.);
#3367=FACE_OUTER_BOUND('',#5542,.T.);
#3368=FACE_OUTER_BOUND('',#5543,.T.);
#3369=FACE_OUTER_BOUND('',#5544,.T.);
#3370=FACE_OUTER_BOUND('',#5545,.T.);
#3371=FACE_OUTER_BOUND('',#5546,.T.);
#3372=FACE_OUTER_BOUND('',#5547,.T.);
#3373=FACE_OUTER_BOUND('',#5548,.T.);
#3374=FACE_OUTER_BOUND('',#5549,.T.);
#3375=FACE_OUTER_BOUND('',#5550,.T.);
#3376=FACE_OUTER_BOUND('',#5551,.T.);
#3377=FACE_OUTER_BOUND('',#5552,.T.);
#3378=FACE_OUTER_BOUND('',#5553,.T.);
#3379=FACE_OUTER_BOUND('',#5554,.T.);
#3380=FACE_OUTER_BOUND('',#5555,.T.);
#3381=FACE_OUTER_BOUND('',#5556,.T.);
#3382=FACE_OUTER_BOUND('',#5557,.T.);
#3383=FACE_OUTER_BOUND('',#5558,.T.);
#3384=FACE_OUTER_BOUND('',#5559,.T.);
#3385=FACE_OUTER_BOUND('',#5560,.T.);
#3386=FACE_OUTER_BOUND('',#5561,.T.);
#3387=FACE_OUTER_BOUND('',#5562,.T.);
#3388=FACE_OUTER_BOUND('',#5563,.T.);
#3389=FACE_OUTER_BOUND('',#5564,.T.);
#3390=FACE_OUTER_BOUND('',#5565,.T.);
#3391=FACE_OUTER_BOUND('',#5566,.T.);
#3392=FACE_OUTER_BOUND('',#5567,.T.);
#3393=FACE_OUTER_BOUND('',#5568,.T.);
#3394=FACE_OUTER_BOUND('',#5569,.T.);
#3395=FACE_OUTER_BOUND('',#5570,.T.);
#3396=FACE_OUTER_BOUND('',#5571,.T.);
#3397=FACE_OUTER_BOUND('',#5572,.T.);
#3398=FACE_OUTER_BOUND('',#5573,.T.);
#3399=FACE_OUTER_BOUND('',#5574,.T.);
#3400=FACE_OUTER_BOUND('',#5575,.T.);
#3401=FACE_OUTER_BOUND('',#5576,.T.);
#3402=FACE_OUTER_BOUND('',#5577,.T.);
#3403=FACE_OUTER_BOUND('',#5578,.T.);
#3404=FACE_OUTER_BOUND('',#5579,.T.);
#3405=FACE_OUTER_BOUND('',#5580,.T.);
#3406=FACE_OUTER_BOUND('',#5581,.T.);
#3407=FACE_OUTER_BOUND('',#5582,.T.);
#3408=FACE_OUTER_BOUND('',#5583,.T.);
#3409=FACE_OUTER_BOUND('',#5584,.T.);
#3410=FACE_OUTER_BOUND('',#5585,.T.);
#3411=FACE_OUTER_BOUND('',#5586,.T.);
#3412=FACE_OUTER_BOUND('',#5587,.T.);
#3413=FACE_OUTER_BOUND('',#5588,.T.);
#3414=FACE_OUTER_BOUND('',#5589,.T.);
#3415=FACE_OUTER_BOUND('',#5590,.T.);
#3416=FACE_OUTER_BOUND('',#5591,.T.);
#3417=FACE_OUTER_BOUND('',#5592,.T.);
#3418=FACE_OUTER_BOUND('',#5593,.T.);
#3419=FACE_OUTER_BOUND('',#5594,.T.);
#3420=FACE_OUTER_BOUND('',#5595,.T.);
#3421=FACE_OUTER_BOUND('',#5596,.T.);
#3422=FACE_OUTER_BOUND('',#5597,.T.);
#3423=FACE_OUTER_BOUND('',#5598,.T.);
#3424=FACE_OUTER_BOUND('',#5599,.T.);
#3425=FACE_OUTER_BOUND('',#5600,.T.);
#3426=FACE_OUTER_BOUND('',#5601,.T.);
#3427=FACE_OUTER_BOUND('',#5602,.T.);
#3428=FACE_OUTER_BOUND('',#5603,.T.);
#3429=FACE_OUTER_BOUND('',#5604,.T.);
#3430=FACE_OUTER_BOUND('',#5605,.T.);
#3431=FACE_OUTER_BOUND('',#5606,.T.);
#3432=FACE_OUTER_BOUND('',#5607,.T.);
#3433=FACE_OUTER_BOUND('',#5608,.T.);
#3434=FACE_OUTER_BOUND('',#5609,.T.);
#3435=FACE_OUTER_BOUND('',#5610,.T.);
#3436=FACE_OUTER_BOUND('',#5611,.T.);
#3437=FACE_OUTER_BOUND('',#5612,.T.);
#3438=FACE_OUTER_BOUND('',#5613,.T.);
#3439=FACE_OUTER_BOUND('',#5614,.T.);
#3440=FACE_OUTER_BOUND('',#5615,.T.);
#3441=FACE_OUTER_BOUND('',#5616,.T.);
#3442=FACE_OUTER_BOUND('',#5617,.T.);
#3443=FACE_OUTER_BOUND('',#5618,.T.);
#3444=FACE_OUTER_BOUND('',#5619,.T.);
#3445=FACE_OUTER_BOUND('',#5620,.T.);
#3446=FACE_OUTER_BOUND('',#5621,.T.);
#3447=FACE_OUTER_BOUND('',#5622,.T.);
#3448=FACE_OUTER_BOUND('',#5623,.T.);
#3449=FACE_OUTER_BOUND('',#5624,.T.);
#3450=FACE_OUTER_BOUND('',#5625,.T.);
#3451=FACE_OUTER_BOUND('',#5626,.T.);
#3452=FACE_OUTER_BOUND('',#5627,.T.);
#3453=FACE_OUTER_BOUND('',#5628,.T.);
#3454=FACE_OUTER_BOUND('',#5629,.T.);
#3455=FACE_OUTER_BOUND('',#5630,.T.);
#3456=FACE_OUTER_BOUND('',#5631,.T.);
#3457=FACE_OUTER_BOUND('',#5632,.T.);
#3458=FACE_OUTER_BOUND('',#5633,.T.);
#3459=FACE_OUTER_BOUND('',#5634,.T.);
#3460=FACE_OUTER_BOUND('',#5635,.T.);
#3461=FACE_OUTER_BOUND('',#5636,.T.);
#3462=FACE_OUTER_BOUND('',#5637,.T.);
#3463=FACE_OUTER_BOUND('',#5638,.T.);
#3464=FACE_OUTER_BOUND('',#5639,.T.);
#3465=FACE_OUTER_BOUND('',#5640,.T.);
#3466=FACE_OUTER_BOUND('',#5641,.T.);
#3467=FACE_OUTER_BOUND('',#5642,.T.);
#3468=FACE_OUTER_BOUND('',#5643,.T.);
#3469=FACE_OUTER_BOUND('',#5644,.T.);
#3470=FACE_OUTER_BOUND('',#5645,.T.);
#3471=FACE_OUTER_BOUND('',#5646,.T.);
#3472=FACE_OUTER_BOUND('',#5647,.T.);
#3473=FACE_OUTER_BOUND('',#5648,.T.);
#3474=FACE_OUTER_BOUND('',#5649,.T.);
#3475=FACE_OUTER_BOUND('',#5650,.T.);
#3476=FACE_OUTER_BOUND('',#5651,.T.);
#3477=FACE_OUTER_BOUND('',#5652,.T.);
#3478=FACE_OUTER_BOUND('',#5653,.T.);
#3479=FACE_OUTER_BOUND('',#5654,.T.);
#3480=FACE_OUTER_BOUND('',#5655,.T.);
#3481=FACE_OUTER_BOUND('',#5656,.T.);
#3482=FACE_OUTER_BOUND('',#5657,.T.);
#3483=FACE_OUTER_BOUND('',#5658,.T.);
#3484=FACE_OUTER_BOUND('',#5659,.T.);
#3485=FACE_OUTER_BOUND('',#5660,.T.);
#3486=FACE_OUTER_BOUND('',#5661,.T.);
#3487=FACE_OUTER_BOUND('',#5662,.T.);
#3488=FACE_OUTER_BOUND('',#5663,.T.);
#3489=FACE_OUTER_BOUND('',#5664,.T.);
#3490=FACE_OUTER_BOUND('',#5665,.T.);
#3491=FACE_OUTER_BOUND('',#5666,.T.);
#3492=FACE_OUTER_BOUND('',#5667,.T.);
#3493=FACE_OUTER_BOUND('',#5668,.T.);
#3494=FACE_OUTER_BOUND('',#5669,.T.);
#3495=FACE_OUTER_BOUND('',#5670,.T.);
#3496=FACE_OUTER_BOUND('',#5671,.T.);
#3497=FACE_OUTER_BOUND('',#5672,.T.);
#3498=FACE_OUTER_BOUND('',#5673,.T.);
#3499=FACE_OUTER_BOUND('',#5674,.T.);
#3500=FACE_OUTER_BOUND('',#5675,.T.);
#3501=FACE_OUTER_BOUND('',#5676,.T.);
#3502=FACE_OUTER_BOUND('',#5677,.T.);
#3503=FACE_OUTER_BOUND('',#5678,.T.);
#3504=FACE_OUTER_BOUND('',#5679,.T.);
#3505=FACE_OUTER_BOUND('',#5680,.T.);
#3506=FACE_OUTER_BOUND('',#5681,.T.);
#3507=FACE_OUTER_BOUND('',#5682,.T.);
#3508=FACE_OUTER_BOUND('',#5683,.T.);
#3509=FACE_OUTER_BOUND('',#5684,.T.);
#3510=FACE_OUTER_BOUND('',#5685,.T.);
#3511=FACE_OUTER_BOUND('',#5686,.T.);
#3512=FACE_OUTER_BOUND('',#5687,.T.);
#3513=FACE_OUTER_BOUND('',#5688,.T.);
#3514=FACE_OUTER_BOUND('',#5689,.T.);
#3515=FACE_OUTER_BOUND('',#5690,.T.);
#3516=FACE_OUTER_BOUND('',#5691,.T.);
#3517=FACE_OUTER_BOUND('',#5692,.T.);
#3518=FACE_OUTER_BOUND('',#5693,.T.);
#3519=FACE_OUTER_BOUND('',#5694,.T.);
#3520=FACE_OUTER_BOUND('',#5695,.T.);
#3521=FACE_OUTER_BOUND('',#5696,.T.);
#3522=FACE_OUTER_BOUND('',#5697,.T.);
#3523=FACE_OUTER_BOUND('',#5698,.T.);
#3524=FACE_OUTER_BOUND('',#5699,.T.);
#3525=FACE_OUTER_BOUND('',#5700,.T.);
#3526=FACE_OUTER_BOUND('',#5701,.T.);
#3527=FACE_OUTER_BOUND('',#5702,.T.);
#3528=FACE_OUTER_BOUND('',#5703,.T.);
#3529=FACE_OUTER_BOUND('',#5704,.T.);
#3530=FACE_OUTER_BOUND('',#5705,.T.);
#3531=FACE_OUTER_BOUND('',#5706,.T.);
#3532=FACE_OUTER_BOUND('',#5707,.T.);
#3533=FACE_OUTER_BOUND('',#5708,.T.);
#3534=FACE_OUTER_BOUND('',#5709,.T.);
#3535=FACE_OUTER_BOUND('',#5710,.T.);
#3536=FACE_OUTER_BOUND('',#5711,.T.);
#3537=FACE_OUTER_BOUND('',#5712,.T.);
#3538=FACE_OUTER_BOUND('',#5713,.T.);
#3539=FACE_OUTER_BOUND('',#5714,.T.);
#3540=FACE_OUTER_BOUND('',#5715,.T.);
#3541=FACE_OUTER_BOUND('',#5716,.T.);
#3542=FACE_OUTER_BOUND('',#5717,.T.);
#3543=FACE_OUTER_BOUND('',#5718,.T.);
#3544=FACE_OUTER_BOUND('',#5719,.T.);
#3545=FACE_OUTER_BOUND('',#5720,.T.);
#3546=FACE_OUTER_BOUND('',#5721,.T.);
#3547=FACE_OUTER_BOUND('',#5722,.T.);
#3548=FACE_OUTER_BOUND('',#5723,.T.);
#3549=FACE_OUTER_BOUND('',#5724,.T.);
#3550=FACE_OUTER_BOUND('',#5725,.T.);
#3551=FACE_OUTER_BOUND('',#5726,.T.);
#3552=FACE_OUTER_BOUND('',#5727,.T.);
#3553=FACE_OUTER_BOUND('',#5728,.T.);
#3554=FACE_OUTER_BOUND('',#5729,.T.);
#3555=FACE_OUTER_BOUND('',#5730,.T.);
#3556=FACE_OUTER_BOUND('',#5731,.T.);
#3557=FACE_OUTER_BOUND('',#5732,.T.);
#3558=FACE_OUTER_BOUND('',#5733,.T.);
#3559=FACE_OUTER_BOUND('',#5734,.T.);
#3560=FACE_OUTER_BOUND('',#5735,.T.);
#3561=FACE_OUTER_BOUND('',#5736,.T.);
#3562=FACE_OUTER_BOUND('',#5737,.T.);
#3563=FACE_OUTER_BOUND('',#5738,.T.);
#3564=FACE_OUTER_BOUND('',#5739,.T.);
#3565=FACE_OUTER_BOUND('',#5740,.T.);
#3566=FACE_OUTER_BOUND('',#5741,.T.);
#3567=FACE_OUTER_BOUND('',#5742,.T.);
#3568=FACE_OUTER_BOUND('',#5743,.T.);
#3569=FACE_OUTER_BOUND('',#5744,.T.);
#3570=FACE_OUTER_BOUND('',#5745,.T.);
#3571=FACE_OUTER_BOUND('',#5746,.T.);
#3572=FACE_OUTER_BOUND('',#5747,.T.);
#3573=FACE_OUTER_BOUND('',#5748,.T.);
#3574=FACE_OUTER_BOUND('',#5749,.T.);
#3575=FACE_OUTER_BOUND('',#5750,.T.);
#3576=FACE_OUTER_BOUND('',#5751,.T.);
#3577=FACE_OUTER_BOUND('',#5752,.T.);
#3578=FACE_OUTER_BOUND('',#5753,.T.);
#3579=FACE_OUTER_BOUND('',#5754,.T.);
#3580=FACE_OUTER_BOUND('',#5755,.T.);
#3581=FACE_OUTER_BOUND('',#5756,.T.);
#3582=FACE_OUTER_BOUND('',#5757,.T.);
#3583=FACE_OUTER_BOUND('',#5758,.T.);
#3584=FACE_OUTER_BOUND('',#5759,.T.);
#3585=FACE_OUTER_BOUND('',#5760,.T.);
#3586=FACE_OUTER_BOUND('',#5761,.T.);
#3587=FACE_OUTER_BOUND('',#5762,.T.);
#3588=FACE_OUTER_BOUND('',#5763,.T.);
#3589=FACE_OUTER_BOUND('',#5764,.T.);
#3590=FACE_OUTER_BOUND('',#5765,.T.);
#3591=FACE_OUTER_BOUND('',#5766,.T.);
#3592=FACE_OUTER_BOUND('',#5767,.T.);
#3593=FACE_OUTER_BOUND('',#5768,.T.);
#3594=FACE_OUTER_BOUND('',#5769,.T.);
#3595=FACE_OUTER_BOUND('',#5770,.T.);
#3596=FACE_OUTER_BOUND('',#5771,.T.);
#3597=FACE_OUTER_BOUND('',#5772,.T.);
#3598=FACE_OUTER_BOUND('',#5773,.T.);
#3599=FACE_OUTER_BOUND('',#5774,.T.);
#3600=FACE_OUTER_BOUND('',#5775,.T.);
#3601=FACE_OUTER_BOUND('',#5776,.T.);
#3602=FACE_OUTER_BOUND('',#5777,.T.);
#3603=FACE_OUTER_BOUND('',#5778,.T.);
#3604=FACE_OUTER_BOUND('',#5779,.T.);
#3605=FACE_OUTER_BOUND('',#5780,.T.);
#3606=FACE_OUTER_BOUND('',#5781,.T.);
#3607=FACE_OUTER_BOUND('',#5782,.T.);
#3608=FACE_OUTER_BOUND('',#5783,.T.);
#3609=FACE_OUTER_BOUND('',#5784,.T.);
#3610=FACE_OUTER_BOUND('',#5785,.T.);
#3611=FACE_OUTER_BOUND('',#5786,.T.);
#3612=FACE_OUTER_BOUND('',#5787,.T.);
#3613=FACE_OUTER_BOUND('',#5788,.T.);
#3614=FACE_OUTER_BOUND('',#5789,.T.);
#3615=FACE_OUTER_BOUND('',#5790,.T.);
#3616=FACE_OUTER_BOUND('',#5791,.T.);
#3617=FACE_OUTER_BOUND('',#5792,.T.);
#3618=FACE_OUTER_BOUND('',#5793,.T.);
#3619=FACE_OUTER_BOUND('',#5794,.T.);
#3620=FACE_OUTER_BOUND('',#5795,.T.);
#3621=FACE_OUTER_BOUND('',#5796,.T.);
#3622=FACE_OUTER_BOUND('',#5797,.T.);
#3623=FACE_OUTER_BOUND('',#5798,.T.);
#3624=FACE_OUTER_BOUND('',#5799,.T.);
#3625=FACE_OUTER_BOUND('',#5800,.T.);
#3626=FACE_OUTER_BOUND('',#5801,.T.);
#3627=FACE_OUTER_BOUND('',#5802,.T.);
#3628=FACE_OUTER_BOUND('',#5803,.T.);
#3629=FACE_OUTER_BOUND('',#5804,.T.);
#3630=FACE_OUTER_BOUND('',#5805,.T.);
#3631=FACE_OUTER_BOUND('',#5806,.T.);
#3632=FACE_OUTER_BOUND('',#5807,.T.);
#3633=FACE_OUTER_BOUND('',#5808,.T.);
#3634=FACE_OUTER_BOUND('',#5809,.T.);
#3635=FACE_OUTER_BOUND('',#5810,.T.);
#3636=FACE_OUTER_BOUND('',#5811,.T.);
#3637=FACE_OUTER_BOUND('',#5812,.T.);
#3638=FACE_OUTER_BOUND('',#5813,.T.);
#3639=FACE_OUTER_BOUND('',#5814,.T.);
#3640=FACE_OUTER_BOUND('',#5815,.T.);
#3641=FACE_OUTER_BOUND('',#5816,.T.);
#3642=FACE_OUTER_BOUND('',#5817,.T.);
#3643=FACE_OUTER_BOUND('',#5818,.T.);
#3644=FACE_OUTER_BOUND('',#5819,.T.);
#3645=FACE_OUTER_BOUND('',#5820,.T.);
#3646=FACE_OUTER_BOUND('',#5821,.T.);
#3647=FACE_OUTER_BOUND('',#5822,.T.);
#3648=FACE_OUTER_BOUND('',#5823,.T.);
#3649=FACE_OUTER_BOUND('',#5824,.T.);
#3650=FACE_OUTER_BOUND('',#5825,.T.);
#3651=FACE_OUTER_BOUND('',#5826,.T.);
#3652=FACE_OUTER_BOUND('',#5827,.T.);
#3653=FACE_OUTER_BOUND('',#5828,.T.);
#3654=FACE_OUTER_BOUND('',#5829,.T.);
#3655=FACE_OUTER_BOUND('',#5830,.T.);
#3656=FACE_OUTER_BOUND('',#5831,.T.);
#3657=FACE_OUTER_BOUND('',#5832,.T.);
#3658=FACE_OUTER_BOUND('',#5833,.T.);
#3659=FACE_OUTER_BOUND('',#5834,.T.);
#3660=FACE_OUTER_BOUND('',#5835,.T.);
#3661=FACE_OUTER_BOUND('',#5836,.T.);
#3662=FACE_OUTER_BOUND('',#5837,.T.);
#3663=FACE_OUTER_BOUND('',#5838,.T.);
#3664=FACE_OUTER_BOUND('',#5839,.T.);
#3665=FACE_OUTER_BOUND('',#5840,.T.);
#3666=FACE_OUTER_BOUND('',#5841,.T.);
#3667=FACE_OUTER_BOUND('',#5842,.T.);
#3668=FACE_OUTER_BOUND('',#5843,.T.);
#3669=FACE_OUTER_BOUND('',#5844,.T.);
#3670=FACE_OUTER_BOUND('',#5845,.T.);
#3671=FACE_OUTER_BOUND('',#5846,.T.);
#3672=FACE_OUTER_BOUND('',#5847,.T.);
#3673=FACE_OUTER_BOUND('',#5848,.T.);
#3674=FACE_OUTER_BOUND('',#5849,.T.);
#3675=FACE_OUTER_BOUND('',#5850,.T.);
#3676=FACE_OUTER_BOUND('',#5851,.T.);
#3677=FACE_OUTER_BOUND('',#5852,.T.);
#3678=FACE_OUTER_BOUND('',#5853,.T.);
#3679=FACE_OUTER_BOUND('',#5854,.T.);
#3680=FACE_OUTER_BOUND('',#5855,.T.);
#3681=FACE_OUTER_BOUND('',#5856,.T.);
#3682=FACE_OUTER_BOUND('',#5857,.T.);
#3683=FACE_OUTER_BOUND('',#5858,.T.);
#3684=FACE_OUTER_BOUND('',#5859,.T.);
#3685=FACE_OUTER_BOUND('',#5860,.T.);
#3686=FACE_OUTER_BOUND('',#5861,.T.);
#3687=FACE_OUTER_BOUND('',#5862,.T.);
#3688=FACE_OUTER_BOUND('',#5863,.T.);
#3689=FACE_OUTER_BOUND('',#5864,.T.);
#3690=FACE_OUTER_BOUND('',#5865,.T.);
#3691=FACE_OUTER_BOUND('',#5866,.T.);
#3692=FACE_OUTER_BOUND('',#5867,.T.);
#3693=FACE_OUTER_BOUND('',#5868,.T.);
#3694=FACE_OUTER_BOUND('',#5869,.T.);
#3695=FACE_OUTER_BOUND('',#5870,.T.);
#3696=FACE_OUTER_BOUND('',#5871,.T.);
#3697=FACE_OUTER_BOUND('',#5872,.T.);
#3698=FACE_OUTER_BOUND('',#5873,.T.);
#3699=FACE_OUTER_BOUND('',#5874,.T.);
#3700=FACE_OUTER_BOUND('',#5875,.T.);
#3701=FACE_OUTER_BOUND('',#5876,.T.);
#3702=FACE_OUTER_BOUND('',#5877,.T.);
#3703=FACE_OUTER_BOUND('',#5878,.T.);
#3704=FACE_OUTER_BOUND('',#5879,.T.);
#3705=FACE_OUTER_BOUND('',#5880,.T.);
#3706=FACE_OUTER_BOUND('',#5881,.T.);
#3707=FACE_OUTER_BOUND('',#5882,.T.);
#3708=FACE_OUTER_BOUND('',#5883,.T.);
#3709=FACE_OUTER_BOUND('',#5884,.T.);
#3710=FACE_OUTER_BOUND('',#5885,.T.);
#3711=FACE_OUTER_BOUND('',#5886,.T.);
#3712=FACE_OUTER_BOUND('',#5887,.T.);
#3713=FACE_OUTER_BOUND('',#5888,.T.);
#3714=FACE_OUTER_BOUND('',#5889,.T.);
#3715=FACE_OUTER_BOUND('',#5890,.T.);
#3716=FACE_OUTER_BOUND('',#5891,.T.);
#3717=FACE_OUTER_BOUND('',#5892,.T.);
#3718=FACE_OUTER_BOUND('',#5893,.T.);
#3719=FACE_OUTER_BOUND('',#5894,.T.);
#3720=FACE_OUTER_BOUND('',#5895,.T.);
#3721=FACE_OUTER_BOUND('',#5896,.T.);
#3722=FACE_OUTER_BOUND('',#5897,.T.);
#3723=FACE_OUTER_BOUND('',#5898,.T.);
#3724=FACE_OUTER_BOUND('',#5899,.T.);
#3725=FACE_OUTER_BOUND('',#5900,.T.);
#3726=FACE_OUTER_BOUND('',#5901,.T.);
#3727=FACE_OUTER_BOUND('',#5902,.T.);
#3728=FACE_OUTER_BOUND('',#5903,.T.);
#3729=FACE_OUTER_BOUND('',#5904,.T.);
#3730=FACE_OUTER_BOUND('',#5905,.T.);
#3731=FACE_OUTER_BOUND('',#5906,.T.);
#3732=FACE_OUTER_BOUND('',#5907,.T.);
#3733=FACE_OUTER_BOUND('',#5908,.T.);
#3734=FACE_OUTER_BOUND('',#5909,.T.);
#3735=FACE_OUTER_BOUND('',#5910,.T.);
#3736=FACE_OUTER_BOUND('',#5911,.T.);
#3737=FACE_OUTER_BOUND('',#5912,.T.);
#3738=FACE_OUTER_BOUND('',#5913,.T.);
#3739=FACE_OUTER_BOUND('',#5914,.T.);
#3740=FACE_OUTER_BOUND('',#5915,.T.);
#3741=FACE_OUTER_BOUND('',#5916,.T.);
#3742=FACE_OUTER_BOUND('',#5917,.T.);
#3743=FACE_OUTER_BOUND('',#5918,.T.);
#3744=FACE_OUTER_BOUND('',#5919,.T.);
#3745=FACE_OUTER_BOUND('',#5920,.T.);
#3746=FACE_OUTER_BOUND('',#5921,.T.);
#3747=FACE_OUTER_BOUND('',#5922,.T.);
#3748=FACE_OUTER_BOUND('',#5923,.T.);
#3749=FACE_OUTER_BOUND('',#5924,.T.);
#3750=FACE_OUTER_BOUND('',#5925,.T.);
#3751=FACE_OUTER_BOUND('',#5926,.T.);
#3752=FACE_OUTER_BOUND('',#5927,.T.);
#3753=FACE_OUTER_BOUND('',#5928,.T.);
#3754=FACE_OUTER_BOUND('',#5929,.T.);
#3755=FACE_OUTER_BOUND('',#5930,.T.);
#3756=FACE_OUTER_BOUND('',#5931,.T.);
#3757=FACE_OUTER_BOUND('',#5932,.T.);
#3758=FACE_OUTER_BOUND('',#5933,.T.);
#3759=FACE_OUTER_BOUND('',#5934,.T.);
#3760=FACE_OUTER_BOUND('',#5935,.T.);
#3761=FACE_OUTER_BOUND('',#5936,.T.);
#3762=FACE_OUTER_BOUND('',#5937,.T.);
#3763=FACE_OUTER_BOUND('',#5938,.T.);
#3764=FACE_OUTER_BOUND('',#5939,.T.);
#3765=FACE_OUTER_BOUND('',#5940,.T.);
#3766=FACE_OUTER_BOUND('',#5941,.T.);
#3767=FACE_OUTER_BOUND('',#5942,.T.);
#3768=FACE_OUTER_BOUND('',#5943,.T.);
#3769=FACE_OUTER_BOUND('',#5944,.T.);
#3770=FACE_OUTER_BOUND('',#5945,.T.);
#3771=FACE_OUTER_BOUND('',#5946,.T.);
#3772=FACE_OUTER_BOUND('',#5947,.T.);
#3773=FACE_OUTER_BOUND('',#5948,.T.);
#3774=FACE_OUTER_BOUND('',#5949,.T.);
#3775=FACE_OUTER_BOUND('',#5950,.T.);
#3776=FACE_OUTER_BOUND('',#5951,.T.);
#3777=FACE_OUTER_BOUND('',#5952,.T.);
#3778=FACE_OUTER_BOUND('',#5953,.T.);
#3779=FACE_OUTER_BOUND('',#5954,.T.);
#3780=FACE_OUTER_BOUND('',#5955,.T.);
#3781=FACE_OUTER_BOUND('',#5956,.T.);
#3782=FACE_OUTER_BOUND('',#5957,.T.);
#3783=FACE_OUTER_BOUND('',#5958,.T.);
#3784=FACE_OUTER_BOUND('',#5959,.T.);
#3785=FACE_OUTER_BOUND('',#5960,.T.);
#3786=FACE_OUTER_BOUND('',#5961,.T.);
#3787=FACE_OUTER_BOUND('',#5962,.T.);
#3788=FACE_OUTER_BOUND('',#5963,.T.);
#3789=FACE_OUTER_BOUND('',#5964,.T.);
#3790=FACE_OUTER_BOUND('',#5965,.T.);
#3791=FACE_OUTER_BOUND('',#5966,.T.);
#3792=FACE_OUTER_BOUND('',#5967,.T.);
#3793=FACE_OUTER_BOUND('',#5968,.T.);
#3794=FACE_OUTER_BOUND('',#5969,.T.);
#3795=FACE_OUTER_BOUND('',#5970,.T.);
#3796=FACE_OUTER_BOUND('',#5971,.T.);
#3797=FACE_OUTER_BOUND('',#5972,.T.);
#3798=FACE_OUTER_BOUND('',#5973,.T.);
#3799=FACE_OUTER_BOUND('',#5974,.T.);
#3800=FACE_OUTER_BOUND('',#5975,.T.);
#3801=FACE_OUTER_BOUND('',#5976,.T.);
#3802=FACE_OUTER_BOUND('',#5977,.T.);
#3803=FACE_OUTER_BOUND('',#5978,.T.);
#3804=FACE_OUTER_BOUND('',#5979,.T.);
#3805=FACE_OUTER_BOUND('',#5980,.T.);
#3806=FACE_OUTER_BOUND('',#5981,.T.);
#3807=FACE_OUTER_BOUND('',#5982,.T.);
#3808=FACE_OUTER_BOUND('',#5983,.T.);
#3809=FACE_OUTER_BOUND('',#5984,.T.);
#3810=FACE_OUTER_BOUND('',#5985,.T.);
#3811=FACE_OUTER_BOUND('',#5986,.T.);
#3812=FACE_OUTER_BOUND('',#5987,.T.);
#3813=FACE_OUTER_BOUND('',#5988,.T.);
#3814=FACE_OUTER_BOUND('',#5989,.T.);
#3815=FACE_OUTER_BOUND('',#5990,.T.);
#3816=FACE_OUTER_BOUND('',#5991,.T.);
#3817=FACE_OUTER_BOUND('',#5992,.T.);
#3818=FACE_OUTER_BOUND('',#5993,.T.);
#3819=FACE_OUTER_BOUND('',#5994,.T.);
#3820=FACE_OUTER_BOUND('',#5995,.T.);
#3821=FACE_OUTER_BOUND('',#5996,.T.);
#3822=FACE_OUTER_BOUND('',#5997,.T.);
#3823=FACE_OUTER_BOUND('',#5998,.T.);
#3824=FACE_OUTER_BOUND('',#5999,.T.);
#3825=FACE_OUTER_BOUND('',#6000,.T.);
#3826=FACE_OUTER_BOUND('',#6001,.T.);
#3827=FACE_OUTER_BOUND('',#6002,.T.);
#3828=FACE_OUTER_BOUND('',#6003,.T.);
#3829=FACE_OUTER_BOUND('',#6004,.T.);
#3830=FACE_OUTER_BOUND('',#6005,.T.);
#3831=FACE_OUTER_BOUND('',#6006,.T.);
#3832=FACE_OUTER_BOUND('',#6007,.T.);
#3833=FACE_OUTER_BOUND('',#6008,.T.);
#3834=FACE_OUTER_BOUND('',#6009,.T.);
#3835=FACE_OUTER_BOUND('',#6010,.T.);
#3836=FACE_OUTER_BOUND('',#6011,.T.);
#3837=FACE_OUTER_BOUND('',#6012,.T.);
#3838=FACE_OUTER_BOUND('',#6013,.T.);
#3839=FACE_OUTER_BOUND('',#6014,.T.);
#3840=FACE_OUTER_BOUND('',#6015,.T.);
#3841=FACE_OUTER_BOUND('',#6016,.T.);
#3842=FACE_OUTER_BOUND('',#6017,.T.);
#3843=FACE_OUTER_BOUND('',#6018,.T.);
#3844=FACE_OUTER_BOUND('',#6019,.T.);
#3845=FACE_OUTER_BOUND('',#6020,.T.);
#3846=FACE_OUTER_BOUND('',#6021,.T.);
#3847=FACE_OUTER_BOUND('',#6022,.T.);
#3848=FACE_OUTER_BOUND('',#6023,.T.);
#3849=FACE_OUTER_BOUND('',#6024,.T.);
#3850=FACE_OUTER_BOUND('',#6025,.T.);
#3851=FACE_OUTER_BOUND('',#6026,.T.);
#3852=FACE_OUTER_BOUND('',#6027,.T.);
#3853=FACE_OUTER_BOUND('',#6028,.T.);
#3854=FACE_OUTER_BOUND('',#6029,.T.);
#3855=FACE_OUTER_BOUND('',#6030,.T.);
#3856=FACE_OUTER_BOUND('',#6031,.T.);
#3857=FACE_OUTER_BOUND('',#6032,.T.);
#3858=FACE_OUTER_BOUND('',#6033,.T.);
#3859=FACE_OUTER_BOUND('',#6034,.T.);
#3860=FACE_OUTER_BOUND('',#6035,.T.);
#3861=FACE_OUTER_BOUND('',#6036,.T.);
#3862=FACE_OUTER_BOUND('',#6037,.T.);
#3863=FACE_OUTER_BOUND('',#6038,.T.);
#3864=FACE_OUTER_BOUND('',#6039,.T.);
#3865=FACE_OUTER_BOUND('',#6040,.T.);
#3866=FACE_OUTER_BOUND('',#6041,.T.);
#3867=FACE_OUTER_BOUND('',#6042,.T.);
#3868=FACE_OUTER_BOUND('',#6043,.T.);
#3869=FACE_OUTER_BOUND('',#6044,.T.);
#3870=FACE_OUTER_BOUND('',#6045,.T.);
#3871=FACE_OUTER_BOUND('',#6046,.T.);
#3872=FACE_OUTER_BOUND('',#6047,.T.);
#3873=FACE_OUTER_BOUND('',#6048,.T.);
#3874=FACE_OUTER_BOUND('',#6049,.T.);
#3875=FACE_OUTER_BOUND('',#6050,.T.);
#3876=FACE_OUTER_BOUND('',#6051,.T.);
#3877=FACE_OUTER_BOUND('',#6052,.T.);
#3878=FACE_OUTER_BOUND('',#6053,.T.);
#3879=FACE_OUTER_BOUND('',#6054,.T.);
#3880=FACE_OUTER_BOUND('',#6055,.T.);
#3881=FACE_OUTER_BOUND('',#6056,.T.);
#3882=FACE_OUTER_BOUND('',#6057,.T.);
#3883=FACE_OUTER_BOUND('',#6058,.T.);
#3884=FACE_OUTER_BOUND('',#6059,.T.);
#3885=FACE_OUTER_BOUND('',#6060,.T.);
#3886=FACE_OUTER_BOUND('',#6061,.T.);
#3887=FACE_OUTER_BOUND('',#6062,.T.);
#3888=FACE_OUTER_BOUND('',#6063,.T.);
#3889=FACE_OUTER_BOUND('',#6064,.T.);
#3890=FACE_OUTER_BOUND('',#6065,.T.);
#3891=FACE_OUTER_BOUND('',#6066,.T.);
#3892=FACE_OUTER_BOUND('',#6067,.T.);
#3893=FACE_OUTER_BOUND('',#6068,.T.);
#3894=FACE_OUTER_BOUND('',#6069,.T.);
#3895=FACE_OUTER_BOUND('',#6070,.T.);
#3896=FACE_OUTER_BOUND('',#6071,.T.);
#3897=FACE_OUTER_BOUND('',#6072,.T.);
#3898=FACE_OUTER_BOUND('',#6073,.T.);
#3899=FACE_OUTER_BOUND('',#6074,.T.);
#3900=FACE_OUTER_BOUND('',#6075,.T.);
#3901=FACE_OUTER_BOUND('',#6076,.T.);
#3902=FACE_OUTER_BOUND('',#6077,.T.);
#3903=FACE_OUTER_BOUND('',#6078,.T.);
#3904=FACE_OUTER_BOUND('',#6079,.T.);
#3905=FACE_OUTER_BOUND('',#6080,.T.);
#3906=FACE_OUTER_BOUND('',#6081,.T.);
#3907=FACE_OUTER_BOUND('',#6082,.T.);
#3908=FACE_OUTER_BOUND('',#6083,.T.);
#3909=FACE_OUTER_BOUND('',#6084,.T.);
#3910=FACE_OUTER_BOUND('',#6085,.T.);
#3911=FACE_OUTER_BOUND('',#6086,.T.);
#3912=FACE_OUTER_BOUND('',#6087,.T.);
#3913=FACE_OUTER_BOUND('',#6088,.T.);
#3914=FACE_OUTER_BOUND('',#6089,.T.);
#3915=FACE_OUTER_BOUND('',#6090,.T.);
#3916=FACE_OUTER_BOUND('',#6091,.T.);
#3917=FACE_OUTER_BOUND('',#6092,.T.);
#3918=FACE_OUTER_BOUND('',#6093,.T.);
#3919=FACE_OUTER_BOUND('',#6094,.T.);
#3920=FACE_OUTER_BOUND('',#6095,.T.);
#3921=FACE_OUTER_BOUND('',#6096,.T.);
#3922=FACE_OUTER_BOUND('',#6097,.T.);
#3923=FACE_OUTER_BOUND('',#6098,.T.);
#3924=FACE_OUTER_BOUND('',#6099,.T.);
#3925=FACE_OUTER_BOUND('',#6100,.T.);
#3926=FACE_OUTER_BOUND('',#6101,.T.);
#3927=FACE_OUTER_BOUND('',#6102,.T.);
#3928=FACE_OUTER_BOUND('',#6103,.T.);
#3929=FACE_OUTER_BOUND('',#6104,.T.);
#3930=FACE_OUTER_BOUND('',#6105,.T.);
#3931=FACE_OUTER_BOUND('',#6106,.T.);
#3932=FACE_OUTER_BOUND('',#6107,.T.);
#3933=FACE_OUTER_BOUND('',#6108,.T.);
#3934=FACE_OUTER_BOUND('',#6109,.T.);
#3935=FACE_OUTER_BOUND('',#6110,.T.);
#3936=FACE_OUTER_BOUND('',#6111,.T.);
#3937=FACE_OUTER_BOUND('',#6112,.T.);
#3938=FACE_OUTER_BOUND('',#6113,.T.);
#3939=FACE_OUTER_BOUND('',#6114,.T.);
#3940=FACE_OUTER_BOUND('',#6115,.T.);
#3941=FACE_OUTER_BOUND('',#6116,.T.);
#3942=FACE_OUTER_BOUND('',#6117,.T.);
#3943=FACE_OUTER_BOUND('',#6118,.T.);
#3944=FACE_OUTER_BOUND('',#6119,.T.);
#3945=FACE_OUTER_BOUND('',#6120,.T.);
#3946=FACE_OUTER_BOUND('',#6121,.T.);
#3947=FACE_OUTER_BOUND('',#6122,.T.);
#3948=FACE_OUTER_BOUND('',#6123,.T.);
#3949=FACE_OUTER_BOUND('',#6124,.T.);
#3950=FACE_OUTER_BOUND('',#6125,.T.);
#3951=FACE_OUTER_BOUND('',#6126,.T.);
#3952=FACE_OUTER_BOUND('',#6127,.T.);
#3953=FACE_OUTER_BOUND('',#6128,.T.);
#3954=FACE_OUTER_BOUND('',#6129,.T.);
#3955=FACE_OUTER_BOUND('',#6130,.T.);
#3956=FACE_OUTER_BOUND('',#6131,.T.);
#3957=FACE_OUTER_BOUND('',#6132,.T.);
#3958=FACE_OUTER_BOUND('',#6133,.T.);
#3959=FACE_OUTER_BOUND('',#6134,.T.);
#3960=FACE_OUTER_BOUND('',#6135,.T.);
#3961=FACE_OUTER_BOUND('',#6136,.T.);
#3962=FACE_OUTER_BOUND('',#6137,.T.);
#3963=FACE_OUTER_BOUND('',#6138,.T.);
#3964=FACE_OUTER_BOUND('',#6139,.T.);
#3965=FACE_OUTER_BOUND('',#6140,.T.);
#3966=FACE_OUTER_BOUND('',#6141,.T.);
#3967=FACE_OUTER_BOUND('',#6142,.T.);
#3968=FACE_OUTER_BOUND('',#6143,.T.);
#3969=FACE_OUTER_BOUND('',#6144,.T.);
#3970=FACE_OUTER_BOUND('',#6145,.T.);
#3971=FACE_OUTER_BOUND('',#6146,.T.);
#3972=FACE_OUTER_BOUND('',#6147,.T.);
#3973=FACE_OUTER_BOUND('',#6148,.T.);
#3974=FACE_OUTER_BOUND('',#6149,.T.);
#3975=FACE_OUTER_BOUND('',#6150,.T.);
#3976=FACE_OUTER_BOUND('',#6151,.T.);
#3977=FACE_OUTER_BOUND('',#6152,.T.);
#3978=FACE_OUTER_BOUND('',#6153,.T.);
#3979=FACE_OUTER_BOUND('',#6154,.T.);
#3980=FACE_OUTER_BOUND('',#6155,.T.);
#3981=FACE_OUTER_BOUND('',#6156,.T.);
#3982=FACE_OUTER_BOUND('',#6157,.T.);
#3983=FACE_OUTER_BOUND('',#6158,.T.);
#3984=FACE_OUTER_BOUND('',#6159,.T.);
#3985=FACE_OUTER_BOUND('',#6160,.T.);
#3986=FACE_OUTER_BOUND('',#6161,.T.);
#3987=FACE_OUTER_BOUND('',#6162,.T.);
#3988=FACE_OUTER_BOUND('',#6163,.T.);
#3989=FACE_OUTER_BOUND('',#6164,.T.);
#3990=FACE_OUTER_BOUND('',#6165,.T.);
#3991=FACE_OUTER_BOUND('',#6166,.T.);
#3992=FACE_OUTER_BOUND('',#6167,.T.);
#3993=FACE_OUTER_BOUND('',#6168,.T.);
#3994=FACE_OUTER_BOUND('',#6169,.T.);
#3995=FACE_OUTER_BOUND('',#6170,.T.);
#3996=FACE_OUTER_BOUND('',#6171,.T.);
#3997=FACE_OUTER_BOUND('',#6172,.T.);
#3998=FACE_OUTER_BOUND('',#6173,.T.);
#3999=FACE_OUTER_BOUND('',#6174,.T.);
#4000=FACE_OUTER_BOUND('',#6175,.T.);
#4001=FACE_OUTER_BOUND('',#6176,.T.);
#4002=FACE_OUTER_BOUND('',#6177,.T.);
#4003=FACE_OUTER_BOUND('',#6178,.T.);
#4004=FACE_OUTER_BOUND('',#6179,.T.);
#4005=FACE_OUTER_BOUND('',#6180,.T.);
#4006=FACE_OUTER_BOUND('',#6181,.T.);
#4007=FACE_OUTER_BOUND('',#6182,.T.);
#4008=FACE_OUTER_BOUND('',#6183,.T.);
#4009=FACE_OUTER_BOUND('',#6184,.T.);
#4010=FACE_OUTER_BOUND('',#6185,.T.);
#4011=FACE_OUTER_BOUND('',#6186,.T.);
#4012=FACE_OUTER_BOUND('',#6187,.T.);
#4013=FACE_OUTER_BOUND('',#6188,.T.);
#4014=FACE_OUTER_BOUND('',#6189,.T.);
#4015=FACE_OUTER_BOUND('',#6190,.T.);
#4016=FACE_OUTER_BOUND('',#6191,.T.);
#4017=FACE_OUTER_BOUND('',#6192,.T.);
#4018=FACE_OUTER_BOUND('',#6193,.T.);
#4019=FACE_OUTER_BOUND('',#6194,.T.);
#4020=FACE_OUTER_BOUND('',#6195,.T.);
#4021=FACE_OUTER_BOUND('',#6196,.T.);
#4022=FACE_OUTER_BOUND('',#6197,.T.);
#4023=FACE_OUTER_BOUND('',#6198,.T.);
#4024=FACE_OUTER_BOUND('',#6199,.T.);
#4025=FACE_OUTER_BOUND('',#6200,.T.);
#4026=FACE_OUTER_BOUND('',#6201,.T.);
#4027=FACE_OUTER_BOUND('',#6202,.T.);
#4028=FACE_OUTER_BOUND('',#6203,.T.);
#4029=FACE_OUTER_BOUND('',#6204,.T.);
#4030=FACE_OUTER_BOUND('',#6205,.T.);
#4031=FACE_OUTER_BOUND('',#6206,.T.);
#4032=FACE_OUTER_BOUND('',#6207,.T.);
#4033=FACE_OUTER_BOUND('',#6208,.T.);
#4034=FACE_OUTER_BOUND('',#6209,.T.);
#4035=FACE_OUTER_BOUND('',#6210,.T.);
#4036=FACE_OUTER_BOUND('',#6211,.T.);
#4037=FACE_OUTER_BOUND('',#6212,.T.);
#4038=FACE_OUTER_BOUND('',#6213,.T.);
#4039=FACE_OUTER_BOUND('',#6214,.T.);
#4040=FACE_OUTER_BOUND('',#6215,.T.);
#4041=FACE_OUTER_BOUND('',#6216,.T.);
#4042=FACE_OUTER_BOUND('',#6217,.T.);
#4043=FACE_OUTER_BOUND('',#6218,.T.);
#4044=FACE_OUTER_BOUND('',#6219,.T.);
#4045=FACE_OUTER_BOUND('',#6220,.T.);
#4046=FACE_OUTER_BOUND('',#6221,.T.);
#4047=FACE_OUTER_BOUND('',#6222,.T.);
#4048=FACE_OUTER_BOUND('',#6223,.T.);
#4049=FACE_OUTER_BOUND('',#6224,.T.);
#4050=FACE_OUTER_BOUND('',#6225,.T.);
#4051=FACE_OUTER_BOUND('',#6226,.T.);
#4052=FACE_OUTER_BOUND('',#6227,.T.);
#4053=FACE_OUTER_BOUND('',#6228,.T.);
#4054=FACE_OUTER_BOUND('',#6229,.T.);
#4055=FACE_OUTER_BOUND('',#6230,.T.);
#4056=FACE_OUTER_BOUND('',#6231,.T.);
#4057=FACE_OUTER_BOUND('',#6232,.T.);
#4058=FACE_OUTER_BOUND('',#6233,.T.);
#4059=FACE_OUTER_BOUND('',#6234,.T.);
#4060=FACE_OUTER_BOUND('',#6235,.T.);
#4061=FACE_OUTER_BOUND('',#6236,.T.);
#4062=FACE_OUTER_BOUND('',#6237,.T.);
#4063=FACE_OUTER_BOUND('',#6238,.T.);
#4064=FACE_OUTER_BOUND('',#6239,.T.);
#4065=FACE_OUTER_BOUND('',#6240,.T.);
#4066=FACE_OUTER_BOUND('',#6241,.T.);
#4067=FACE_OUTER_BOUND('',#6242,.T.);
#4068=FACE_OUTER_BOUND('',#6243,.T.);
#4069=FACE_OUTER_BOUND('',#6244,.T.);
#4070=FACE_OUTER_BOUND('',#6245,.T.);
#4071=FACE_OUTER_BOUND('',#6246,.T.);
#4072=FACE_OUTER_BOUND('',#6247,.T.);
#4073=FACE_OUTER_BOUND('',#6248,.T.);
#4074=FACE_OUTER_BOUND('',#6249,.T.);
#4075=FACE_OUTER_BOUND('',#6250,.T.);
#4076=FACE_OUTER_BOUND('',#6251,.T.);
#4077=FACE_OUTER_BOUND('',#6252,.T.);
#4078=FACE_OUTER_BOUND('',#6253,.T.);
#4079=FACE_OUTER_BOUND('',#6254,.T.);
#4080=FACE_OUTER_BOUND('',#6255,.T.);
#4081=FACE_OUTER_BOUND('',#6256,.T.);
#4082=FACE_OUTER_BOUND('',#6257,.T.);
#4083=FACE_OUTER_BOUND('',#6258,.T.);
#4084=FACE_OUTER_BOUND('',#6259,.T.);
#4085=FACE_OUTER_BOUND('',#6260,.T.);
#4086=FACE_OUTER_BOUND('',#6261,.T.);
#4087=FACE_OUTER_BOUND('',#6262,.T.);
#4088=FACE_OUTER_BOUND('',#6263,.T.);
#4089=FACE_OUTER_BOUND('',#6264,.T.);
#4090=FACE_OUTER_BOUND('',#6265,.T.);
#4091=FACE_OUTER_BOUND('',#6266,.T.);
#4092=FACE_OUTER_BOUND('',#6267,.T.);
#4093=FACE_OUTER_BOUND('',#6268,.T.);
#4094=FACE_OUTER_BOUND('',#6269,.T.);
#4095=FACE_OUTER_BOUND('',#6270,.T.);
#4096=FACE_OUTER_BOUND('',#6271,.T.);
#4097=FACE_OUTER_BOUND('',#6272,.T.);
#4098=FACE_OUTER_BOUND('',#6273,.T.);
#4099=FACE_OUTER_BOUND('',#6274,.T.);
#4100=FACE_OUTER_BOUND('',#6275,.T.);
#4101=FACE_OUTER_BOUND('',#6276,.T.);
#4102=FACE_OUTER_BOUND('',#6277,.T.);
#4103=FACE_OUTER_BOUND('',#6278,.T.);
#4104=FACE_OUTER_BOUND('',#6279,.T.);
#4105=FACE_OUTER_BOUND('',#6280,.T.);
#4106=FACE_OUTER_BOUND('',#6281,.T.);
#4107=FACE_OUTER_BOUND('',#6282,.T.);
#4108=FACE_OUTER_BOUND('',#6283,.T.);
#4109=FACE_OUTER_BOUND('',#6284,.T.);
#4110=FACE_OUTER_BOUND('',#6285,.T.);
#4111=FACE_OUTER_BOUND('',#6286,.T.);
#4112=FACE_OUTER_BOUND('',#6287,.T.);
#4113=FACE_OUTER_BOUND('',#6288,.T.);
#4114=FACE_OUTER_BOUND('',#6289,.T.);
#4115=FACE_OUTER_BOUND('',#6290,.T.);
#4116=FACE_OUTER_BOUND('',#6291,.T.);
#4117=FACE_OUTER_BOUND('',#6292,.T.);
#4118=FACE_OUTER_BOUND('',#6293,.T.);
#4119=FACE_OUTER_BOUND('',#6294,.T.);
#4120=FACE_OUTER_BOUND('',#6295,.T.);
#4121=FACE_OUTER_BOUND('',#6296,.T.);
#4122=FACE_OUTER_BOUND('',#6297,.T.);
#4123=FACE_OUTER_BOUND('',#6298,.T.);
#4124=FACE_OUTER_BOUND('',#6299,.T.);
#4125=FACE_OUTER_BOUND('',#6300,.T.);
#4126=FACE_OUTER_BOUND('',#6301,.T.);
#4127=FACE_OUTER_BOUND('',#6302,.T.);
#4128=FACE_OUTER_BOUND('',#6303,.T.);
#4129=FACE_OUTER_BOUND('',#6304,.T.);
#4130=FACE_OUTER_BOUND('',#6305,.T.);
#4131=FACE_OUTER_BOUND('',#6306,.T.);
#4132=FACE_OUTER_BOUND('',#6307,.T.);
#4133=FACE_OUTER_BOUND('',#6308,.T.);
#4134=FACE_OUTER_BOUND('',#6309,.T.);
#4135=FACE_OUTER_BOUND('',#6310,.T.);
#4136=FACE_OUTER_BOUND('',#6311,.T.);
#4137=FACE_OUTER_BOUND('',#6312,.T.);
#4138=FACE_OUTER_BOUND('',#6313,.T.);
#4139=FACE_OUTER_BOUND('',#6314,.T.);
#4140=FACE_OUTER_BOUND('',#6315,.T.);
#4141=FACE_OUTER_BOUND('',#6316,.T.);
#4142=FACE_OUTER_BOUND('',#6317,.T.);
#4143=FACE_OUTER_BOUND('',#6318,.T.);
#4144=FACE_OUTER_BOUND('',#6319,.T.);
#4145=FACE_OUTER_BOUND('',#6320,.T.);
#4146=FACE_OUTER_BOUND('',#6321,.T.);
#4147=FACE_OUTER_BOUND('',#6322,.T.);
#4148=FACE_OUTER_BOUND('',#6323,.T.);
#4149=FACE_OUTER_BOUND('',#6324,.T.);
#4150=FACE_OUTER_BOUND('',#6325,.T.);
#4151=FACE_OUTER_BOUND('',#6326,.T.);
#4152=FACE_OUTER_BOUND('',#6327,.T.);
#4153=FACE_OUTER_BOUND('',#6328,.T.);
#4154=FACE_OUTER_BOUND('',#6329,.T.);
#4155=FACE_OUTER_BOUND('',#6330,.T.);
#4156=FACE_OUTER_BOUND('',#6331,.T.);
#4157=FACE_OUTER_BOUND('',#6332,.T.);
#4158=FACE_OUTER_BOUND('',#6333,.T.);
#4159=FACE_OUTER_BOUND('',#6334,.T.);
#4160=FACE_OUTER_BOUND('',#6335,.T.);
#4161=FACE_OUTER_BOUND('',#6336,.T.);
#4162=FACE_OUTER_BOUND('',#6337,.T.);
#4163=FACE_OUTER_BOUND('',#6338,.T.);
#4164=FACE_OUTER_BOUND('',#6339,.T.);
#4165=FACE_OUTER_BOUND('',#6340,.T.);
#4166=FACE_OUTER_BOUND('',#6341,.T.);
#4167=FACE_OUTER_BOUND('',#6342,.T.);
#4168=FACE_OUTER_BOUND('',#6343,.T.);
#4169=FACE_OUTER_BOUND('',#6344,.T.);
#4170=FACE_OUTER_BOUND('',#6345,.T.);
#4171=FACE_OUTER_BOUND('',#6346,.T.);
#4172=FACE_OUTER_BOUND('',#6347,.T.);
#4173=FACE_OUTER_BOUND('',#6348,.T.);
#4174=FACE_OUTER_BOUND('',#6349,.T.);
#4175=FACE_OUTER_BOUND('',#6350,.T.);
#4176=FACE_OUTER_BOUND('',#6351,.T.);
#4177=FACE_OUTER_BOUND('',#6352,.T.);
#4178=FACE_OUTER_BOUND('',#6353,.T.);
#4179=FACE_OUTER_BOUND('',#6354,.T.);
#4180=FACE_OUTER_BOUND('',#6355,.T.);
#4181=FACE_OUTER_BOUND('',#6356,.T.);
#4182=FACE_OUTER_BOUND('',#6357,.T.);
#4183=FACE_OUTER_BOUND('',#6358,.T.);
#4184=FACE_OUTER_BOUND('',#6359,.T.);
#4185=FACE_OUTER_BOUND('',#6360,.T.);
#4186=FACE_OUTER_BOUND('',#6361,.T.);
#4187=FACE_OUTER_BOUND('',#6362,.T.);
#4188=FACE_OUTER_BOUND('',#6363,.T.);
#4189=FACE_OUTER_BOUND('',#6364,.T.);
#4190=FACE_OUTER_BOUND('',#6365,.T.);
#4191=FACE_OUTER_BOUND('',#6366,.T.);
#4192=FACE_OUTER_BOUND('',#6367,.T.);
#4193=FACE_OUTER_BOUND('',#6368,.T.);
#4194=FACE_OUTER_BOUND('',#6369,.T.);
#4195=FACE_OUTER_BOUND('',#6370,.T.);
#4196=FACE_OUTER_BOUND('',#6371,.T.);
#4197=FACE_OUTER_BOUND('',#6372,.T.);
#4198=FACE_OUTER_BOUND('',#6373,.T.);
#4199=FACE_OUTER_BOUND('',#6374,.T.);
#4200=FACE_OUTER_BOUND('',#6375,.T.);
#4201=FACE_OUTER_BOUND('',#6376,.T.);
#4202=FACE_OUTER_BOUND('',#6377,.T.);
#4203=FACE_OUTER_BOUND('',#6378,.T.);
#4204=FACE_OUTER_BOUND('',#6379,.T.);
#4205=FACE_OUTER_BOUND('',#6380,.T.);
#4206=FACE_OUTER_BOUND('',#6381,.T.);
#4207=FACE_OUTER_BOUND('',#6382,.T.);
#4208=FACE_OUTER_BOUND('',#6383,.T.);
#4209=FACE_OUTER_BOUND('',#6384,.T.);
#4210=FACE_OUTER_BOUND('',#6385,.T.);
#4211=FACE_OUTER_BOUND('',#6386,.T.);
#4212=FACE_OUTER_BOUND('',#6387,.T.);
#4213=FACE_OUTER_BOUND('',#6388,.T.);
#4214=FACE_OUTER_BOUND('',#6389,.T.);
#4215=FACE_OUTER_BOUND('',#6390,.T.);
#4216=FACE_OUTER_BOUND('',#6391,.T.);
#4217=FACE_OUTER_BOUND('',#6392,.T.);
#4218=FACE_OUTER_BOUND('',#6393,.T.);
#4219=FACE_OUTER_BOUND('',#6394,.T.);
#4220=FACE_OUTER_BOUND('',#6395,.T.);
#4221=FACE_OUTER_BOUND('',#6396,.T.);
#4222=FACE_OUTER_BOUND('',#6397,.T.);
#4223=FACE_OUTER_BOUND('',#6398,.T.);
#4224=FACE_OUTER_BOUND('',#6400,.T.);
#4225=FACE_OUTER_BOUND('',#6401,.T.);
#4226=FACE_OUTER_BOUND('',#6402,.T.);
#4227=FACE_OUTER_BOUND('',#6403,.T.);
#4228=FACE_OUTER_BOUND('',#6404,.T.);
#4229=FACE_OUTER_BOUND('',#6405,.T.);
#4230=FACE_OUTER_BOUND('',#6406,.T.);
#4231=FACE_OUTER_BOUND('',#6407,.T.);
#4232=FACE_OUTER_BOUND('',#6408,.T.);
#4233=FACE_OUTER_BOUND('',#6409,.T.);
#4234=FACE_OUTER_BOUND('',#6410,.T.);
#4235=FACE_OUTER_BOUND('',#6411,.T.);
#4236=FACE_OUTER_BOUND('',#6412,.T.);
#4237=FACE_OUTER_BOUND('',#6413,.T.);
#4238=FACE_OUTER_BOUND('',#6414,.T.);
#4239=FACE_OUTER_BOUND('',#6415,.T.);
#4240=FACE_OUTER_BOUND('',#6416,.T.);
#4241=FACE_OUTER_BOUND('',#6417,.T.);
#4242=FACE_OUTER_BOUND('',#6418,.T.);
#4243=FACE_OUTER_BOUND('',#6419,.T.);
#4244=FACE_OUTER_BOUND('',#6420,.T.);
#4245=FACE_OUTER_BOUND('',#6421,.T.);
#4246=FACE_OUTER_BOUND('',#6422,.T.);
#4247=FACE_OUTER_BOUND('',#6423,.T.);
#4248=FACE_OUTER_BOUND('',#6424,.T.);
#4249=FACE_OUTER_BOUND('',#6425,.T.);
#4250=FACE_OUTER_BOUND('',#6426,.T.);
#4251=FACE_OUTER_BOUND('',#6427,.T.);
#4252=FACE_OUTER_BOUND('',#6428,.T.);
#4253=FACE_OUTER_BOUND('',#6429,.T.);
#4254=FACE_OUTER_BOUND('',#6430,.T.);
#4255=FACE_OUTER_BOUND('',#6431,.T.);
#4256=FACE_OUTER_BOUND('',#6432,.T.);
#4257=FACE_OUTER_BOUND('',#6433,.T.);
#4258=FACE_OUTER_BOUND('',#6434,.T.);
#4259=FACE_OUTER_BOUND('',#6435,.T.);
#4260=FACE_OUTER_BOUND('',#6436,.T.);
#4261=FACE_OUTER_BOUND('',#6437,.T.);
#4262=FACE_OUTER_BOUND('',#6438,.T.);
#4263=FACE_OUTER_BOUND('',#6439,.T.);
#4264=FACE_OUTER_BOUND('',#6440,.T.);
#4265=FACE_OUTER_BOUND('',#6441,.T.);
#4266=FACE_OUTER_BOUND('',#6442,.T.);
#4267=FACE_OUTER_BOUND('',#6443,.T.);
#4268=FACE_OUTER_BOUND('',#6444,.T.);
#4269=FACE_OUTER_BOUND('',#6445,.T.);
#4270=FACE_OUTER_BOUND('',#6446,.T.);
#4271=FACE_OUTER_BOUND('',#6447,.T.);
#4272=FACE_OUTER_BOUND('',#6448,.T.);
#4273=FACE_OUTER_BOUND('',#6449,.T.);
#4274=FACE_OUTER_BOUND('',#6450,.T.);
#4275=FACE_OUTER_BOUND('',#6451,.T.);
#4276=FACE_OUTER_BOUND('',#6452,.T.);
#4277=FACE_OUTER_BOUND('',#6453,.T.);
#4278=FACE_OUTER_BOUND('',#6454,.T.);
#4279=FACE_OUTER_BOUND('',#6455,.T.);
#4280=FACE_OUTER_BOUND('',#6456,.T.);
#4281=FACE_OUTER_BOUND('',#6457,.T.);
#4282=FACE_OUTER_BOUND('',#6458,.T.);
#4283=FACE_OUTER_BOUND('',#6459,.T.);
#4284=FACE_OUTER_BOUND('',#6460,.T.);
#4285=FACE_OUTER_BOUND('',#6461,.T.);
#4286=FACE_OUTER_BOUND('',#6462,.T.);
#4287=FACE_OUTER_BOUND('',#6463,.T.);
#4288=FACE_OUTER_BOUND('',#6464,.T.);
#4289=FACE_OUTER_BOUND('',#6465,.T.);
#4290=FACE_OUTER_BOUND('',#6466,.T.);
#4291=FACE_OUTER_BOUND('',#6467,.T.);
#4292=FACE_OUTER_BOUND('',#6468,.T.);
#4293=FACE_OUTER_BOUND('',#6469,.T.);
#4294=FACE_OUTER_BOUND('',#6470,.T.);
#4295=FACE_OUTER_BOUND('',#6471,.T.);
#4296=FACE_OUTER_BOUND('',#6472,.T.);
#4297=FACE_OUTER_BOUND('',#6473,.T.);
#4298=FACE_OUTER_BOUND('',#6474,.T.);
#4299=FACE_OUTER_BOUND('',#6475,.T.);
#4300=FACE_OUTER_BOUND('',#6476,.T.);
#4301=FACE_OUTER_BOUND('',#6477,.T.);
#4302=FACE_OUTER_BOUND('',#6478,.T.);
#4303=FACE_OUTER_BOUND('',#6479,.T.);
#4304=FACE_OUTER_BOUND('',#6480,.T.);
#4305=FACE_OUTER_BOUND('',#6481,.T.);
#4306=FACE_OUTER_BOUND('',#6482,.T.);
#4307=FACE_OUTER_BOUND('',#6483,.T.);
#4308=FACE_OUTER_BOUND('',#6484,.T.);
#4309=FACE_OUTER_BOUND('',#6485,.T.);
#4310=FACE_OUTER_BOUND('',#6486,.T.);
#4311=FACE_OUTER_BOUND('',#6487,.T.);
#4312=FACE_OUTER_BOUND('',#6488,.T.);
#4313=FACE_OUTER_BOUND('',#6489,.T.);
#4314=FACE_OUTER_BOUND('',#6490,.T.);
#4315=FACE_OUTER_BOUND('',#6491,.T.);
#4316=FACE_OUTER_BOUND('',#6492,.T.);
#4317=FACE_OUTER_BOUND('',#6493,.T.);
#4318=FACE_OUTER_BOUND('',#6494,.T.);
#4319=FACE_OUTER_BOUND('',#6495,.T.);
#4320=FACE_OUTER_BOUND('',#6496,.T.);
#4321=FACE_OUTER_BOUND('',#6497,.T.);
#4322=FACE_OUTER_BOUND('',#6498,.T.);
#4323=FACE_OUTER_BOUND('',#6499,.T.);
#4324=FACE_OUTER_BOUND('',#6500,.T.);
#4325=FACE_OUTER_BOUND('',#6501,.T.);
#4326=FACE_OUTER_BOUND('',#6502,.T.);
#4327=FACE_OUTER_BOUND('',#6503,.T.);
#4328=FACE_OUTER_BOUND('',#6504,.T.);
#4329=FACE_OUTER_BOUND('',#6505,.T.);
#4330=FACE_OUTER_BOUND('',#6506,.T.);
#4331=FACE_OUTER_BOUND('',#6507,.T.);
#4332=FACE_OUTER_BOUND('',#6508,.T.);
#4333=FACE_OUTER_BOUND('',#6509,.T.);
#4334=FACE_OUTER_BOUND('',#6510,.T.);
#4335=FACE_OUTER_BOUND('',#6511,.T.);
#4336=FACE_OUTER_BOUND('',#6512,.T.);
#4337=FACE_OUTER_BOUND('',#6513,.T.);
#4338=FACE_OUTER_BOUND('',#6514,.T.);
#4339=FACE_OUTER_BOUND('',#6515,.T.);
#4340=FACE_OUTER_BOUND('',#6516,.T.);
#4341=FACE_OUTER_BOUND('',#6517,.T.);
#4342=FACE_OUTER_BOUND('',#6518,.T.);
#4343=FACE_OUTER_BOUND('',#6519,.T.);
#4344=FACE_OUTER_BOUND('',#6520,.T.);
#4345=FACE_OUTER_BOUND('',#6521,.T.);
#4346=FACE_OUTER_BOUND('',#6522,.T.);
#4347=FACE_OUTER_BOUND('',#6523,.T.);
#4348=FACE_OUTER_BOUND('',#6524,.T.);
#4349=FACE_OUTER_BOUND('',#6525,.T.);
#4350=FACE_OUTER_BOUND('',#6526,.T.);
#4351=FACE_OUTER_BOUND('',#6527,.T.);
#4352=FACE_OUTER_BOUND('',#6528,.T.);
#4353=FACE_OUTER_BOUND('',#6529,.T.);
#4354=FACE_OUTER_BOUND('',#6530,.T.);
#4355=FACE_OUTER_BOUND('',#6531,.T.);
#4356=FACE_OUTER_BOUND('',#6532,.T.);
#4357=FACE_OUTER_BOUND('',#6533,.T.);
#4358=FACE_OUTER_BOUND('',#6534,.T.);
#4359=FACE_OUTER_BOUND('',#6535,.T.);
#4360=FACE_OUTER_BOUND('',#6536,.T.);
#4361=FACE_OUTER_BOUND('',#6537,.T.);
#4362=FACE_OUTER_BOUND('',#6538,.T.);
#4363=FACE_OUTER_BOUND('',#6539,.T.);
#4364=FACE_OUTER_BOUND('',#6540,.T.);
#4365=FACE_OUTER_BOUND('',#6541,.T.);
#4366=FACE_OUTER_BOUND('',#6542,.T.);
#4367=FACE_OUTER_BOUND('',#6543,.T.);
#4368=FACE_OUTER_BOUND('',#6544,.T.);
#4369=FACE_OUTER_BOUND('',#6545,.T.);
#4370=FACE_OUTER_BOUND('',#6546,.T.);
#4371=FACE_OUTER_BOUND('',#6547,.T.);
#4372=FACE_OUTER_BOUND('',#6548,.T.);
#4373=FACE_OUTER_BOUND('',#6549,.T.);
#4374=FACE_OUTER_BOUND('',#6550,.T.);
#4375=FACE_OUTER_BOUND('',#6551,.T.);
#4376=FACE_OUTER_BOUND('',#6552,.T.);
#4377=FACE_OUTER_BOUND('',#6553,.T.);
#4378=FACE_OUTER_BOUND('',#6554,.T.);
#4379=FACE_OUTER_BOUND('',#6555,.T.);
#4380=FACE_OUTER_BOUND('',#6556,.T.);
#4381=FACE_OUTER_BOUND('',#6557,.T.);
#4382=FACE_OUTER_BOUND('',#6558,.T.);
#4383=FACE_OUTER_BOUND('',#6560,.T.);
#4384=FACE_OUTER_BOUND('',#6561,.T.);
#4385=FACE_OUTER_BOUND('',#6563,.T.);
#4386=FACE_OUTER_BOUND('',#6564,.T.);
#4387=FACE_OUTER_BOUND('',#6566,.T.);
#4388=FACE_OUTER_BOUND('',#6567,.T.);
#4389=FACE_OUTER_BOUND('',#6569,.T.);
#4390=FACE_OUTER_BOUND('',#6570,.T.);
#4391=FACE_OUTER_BOUND('',#6571,.T.);
#4392=FACE_OUTER_BOUND('',#6572,.T.);
#4393=FACE_OUTER_BOUND('',#6579,.T.);
#4394=FACE_OUTER_BOUND('',#6580,.T.);
#4395=FACE_OUTER_BOUND('',#6581,.T.);
#4396=FACE_OUTER_BOUND('',#6582,.T.);
#4397=FACE_OUTER_BOUND('',#6583,.T.);
#4398=FACE_OUTER_BOUND('',#6584,.T.);
#4399=FACE_OUTER_BOUND('',#6585,.T.);
#4400=FACE_OUTER_BOUND('',#6586,.T.);
#4401=FACE_OUTER_BOUND('',#6587,.T.);
#4402=FACE_OUTER_BOUND('',#6588,.T.);
#4403=FACE_OUTER_BOUND('',#6589,.T.);
#4404=FACE_OUTER_BOUND('',#6590,.T.);
#4405=FACE_OUTER_BOUND('',#6591,.T.);
#4406=FACE_OUTER_BOUND('',#6592,.T.);
#4407=FACE_OUTER_BOUND('',#6594,.T.);
#4408=FACE_OUTER_BOUND('',#6595,.T.);
#4409=FACE_OUTER_BOUND('',#6596,.T.);
#4410=FACE_OUTER_BOUND('',#6597,.T.);
#4411=FACE_OUTER_BOUND('',#6598,.T.);
#4412=FACE_OUTER_BOUND('',#6599,.T.);
#4413=FACE_OUTER_BOUND('',#6600,.T.);
#4414=FACE_OUTER_BOUND('',#6601,.T.);
#4415=FACE_OUTER_BOUND('',#6602,.T.);
#4416=FACE_OUTER_BOUND('',#6603,.T.);
#4417=FACE_OUTER_BOUND('',#6604,.T.);
#4418=FACE_OUTER_BOUND('',#6605,.T.);
#4419=FACE_OUTER_BOUND('',#6606,.T.);
#4420=FACE_OUTER_BOUND('',#6607,.T.);
#4421=FACE_OUTER_BOUND('',#6608,.T.);
#4422=FACE_OUTER_BOUND('',#6609,.T.);
#4423=FACE_OUTER_BOUND('',#6610,.T.);
#4424=FACE_OUTER_BOUND('',#6611,.T.);
#4425=FACE_OUTER_BOUND('',#6612,.T.);
#4426=FACE_OUTER_BOUND('',#6613,.T.);
#4427=FACE_OUTER_BOUND('',#6614,.T.);
#4428=FACE_OUTER_BOUND('',#6615,.T.);
#4429=FACE_OUTER_BOUND('',#6616,.T.);
#4430=FACE_OUTER_BOUND('',#6617,.T.);
#4431=FACE_OUTER_BOUND('',#6618,.T.);
#4432=FACE_OUTER_BOUND('',#6619,.T.);
#4433=FACE_OUTER_BOUND('',#6620,.T.);
#4434=FACE_OUTER_BOUND('',#6621,.T.);
#4435=FACE_OUTER_BOUND('',#6622,.T.);
#4436=FACE_OUTER_BOUND('',#6623,.T.);
#4437=FACE_OUTER_BOUND('',#6624,.T.);
#4438=FACE_OUTER_BOUND('',#6625,.T.);
#4439=FACE_OUTER_BOUND('',#6626,.T.);
#4440=FACE_OUTER_BOUND('',#6627,.T.);
#4441=FACE_OUTER_BOUND('',#6628,.T.);
#4442=FACE_OUTER_BOUND('',#6629,.T.);
#4443=FACE_OUTER_BOUND('',#6630,.T.);
#4444=FACE_OUTER_BOUND('',#6636,.T.);
#4445=FACE_OUTER_BOUND('',#6637,.T.);
#4446=FACE_OUTER_BOUND('',#6638,.T.);
#4447=FACE_OUTER_BOUND('',#6639,.T.);
#4448=FACE_OUTER_BOUND('',#6640,.T.);
#4449=FACE_OUTER_BOUND('',#6641,.T.);
#4450=FACE_OUTER_BOUND('',#6642,.T.);
#4451=FACE_OUTER_BOUND('',#6643,.T.);
#4452=FACE_OUTER_BOUND('',#6644,.T.);
#4453=FACE_OUTER_BOUND('',#6650,.T.);
#4454=FACE_OUTER_BOUND('',#6651,.T.);
#4455=FACE_OUTER_BOUND('',#6652,.T.);
#4456=FACE_OUTER_BOUND('',#6653,.T.);
#4457=FACE_OUTER_BOUND('',#6654,.T.);
#4458=FACE_OUTER_BOUND('',#6655,.T.);
#4459=FACE_OUTER_BOUND('',#6656,.T.);
#4460=FACE_OUTER_BOUND('',#6657,.T.);
#4461=FACE_OUTER_BOUND('',#6658,.T.);
#4462=FACE_OUTER_BOUND('',#6659,.T.);
#4463=FACE_OUTER_BOUND('',#6660,.T.);
#4464=FACE_OUTER_BOUND('',#6661,.T.);
#4465=FACE_OUTER_BOUND('',#6662,.T.);
#4466=FACE_OUTER_BOUND('',#6663,.T.);
#4467=FACE_OUTER_BOUND('',#6664,.T.);
#4468=FACE_OUTER_BOUND('',#6665,.T.);
#4469=FACE_OUTER_BOUND('',#6666,.T.);
#4470=FACE_OUTER_BOUND('',#6667,.T.);
#4471=FACE_OUTER_BOUND('',#6668,.T.);
#4472=FACE_OUTER_BOUND('',#6669,.T.);
#4473=FACE_OUTER_BOUND('',#6670,.T.);
#4474=FACE_OUTER_BOUND('',#6671,.T.);
#4475=FACE_OUTER_BOUND('',#6672,.T.);
#4476=FACE_OUTER_BOUND('',#6673,.T.);
#4477=FACE_OUTER_BOUND('',#6674,.T.);
#4478=FACE_OUTER_BOUND('',#6675,.T.);
#4479=FACE_OUTER_BOUND('',#6676,.T.);
#4480=FACE_OUTER_BOUND('',#6677,.T.);
#4481=FACE_OUTER_BOUND('',#6678,.T.);
#4482=FACE_OUTER_BOUND('',#6679,.T.);
#4483=FACE_OUTER_BOUND('',#6680,.T.);
#4484=FACE_OUTER_BOUND('',#6681,.T.);
#4485=FACE_OUTER_BOUND('',#6682,.T.);
#4486=FACE_OUTER_BOUND('',#6683,.T.);
#4487=FACE_OUTER_BOUND('',#6684,.T.);
#4488=FACE_OUTER_BOUND('',#6685,.T.);
#4489=FACE_OUTER_BOUND('',#6686,.T.);
#4490=FACE_OUTER_BOUND('',#6687,.T.);
#4491=FACE_OUTER_BOUND('',#6688,.T.);
#4492=FACE_OUTER_BOUND('',#6689,.T.);
#4493=FACE_OUTER_BOUND('',#6690,.T.);
#4494=FACE_OUTER_BOUND('',#6691,.T.);
#4495=FACE_OUTER_BOUND('',#6692,.T.);
#4496=FACE_OUTER_BOUND('',#6693,.T.);
#4497=FACE_OUTER_BOUND('',#6694,.T.);
#4498=FACE_OUTER_BOUND('',#6695,.T.);
#4499=FACE_OUTER_BOUND('',#6696,.T.);
#4500=FACE_OUTER_BOUND('',#6697,.T.);
#4501=FACE_OUTER_BOUND('',#6698,.T.);
#4502=FACE_OUTER_BOUND('',#6699,.T.);
#4503=FACE_OUTER_BOUND('',#6700,.T.);
#4504=FACE_OUTER_BOUND('',#6701,.T.);
#4505=FACE_OUTER_BOUND('',#6702,.T.);
#4506=FACE_OUTER_BOUND('',#6703,.T.);
#4507=FACE_OUTER_BOUND('',#6704,.T.);
#4508=FACE_OUTER_BOUND('',#6705,.T.);
#4509=FACE_OUTER_BOUND('',#6706,.T.);
#4510=FACE_OUTER_BOUND('',#6707,.T.);
#4511=FACE_OUTER_BOUND('',#6708,.T.);
#4512=FACE_OUTER_BOUND('',#6709,.T.);
#4513=FACE_OUTER_BOUND('',#6710,.T.);
#4514=FACE_OUTER_BOUND('',#6711,.T.);
#4515=FACE_OUTER_BOUND('',#6713,.T.);
#4516=FACE_OUTER_BOUND('',#6714,.T.);
#4517=FACE_OUTER_BOUND('',#6715,.T.);
#4518=FACE_OUTER_BOUND('',#6716,.T.);
#4519=FACE_OUTER_BOUND('',#6717,.T.);
#4520=FACE_OUTER_BOUND('',#6718,.T.);
#4521=FACE_OUTER_BOUND('',#6719,.T.);
#4522=FACE_OUTER_BOUND('',#6720,.T.);
#4523=FACE_OUTER_BOUND('',#6721,.T.);
#4524=FACE_OUTER_BOUND('',#6723,.T.);
#4525=FACE_OUTER_BOUND('',#6724,.T.);
#4526=FACE_OUTER_BOUND('',#6725,.T.);
#4527=FACE_OUTER_BOUND('',#6726,.T.);
#4528=FACE_OUTER_BOUND('',#6727,.T.);
#4529=FACE_OUTER_BOUND('',#6728,.T.);
#4530=FACE_OUTER_BOUND('',#6729,.T.);
#4531=FACE_OUTER_BOUND('',#6731,.T.);
#4532=FACE_OUTER_BOUND('',#6732,.T.);
#4533=FACE_OUTER_BOUND('',#6733,.T.);
#4534=FACE_OUTER_BOUND('',#6735,.T.);
#4535=FACE_OUTER_BOUND('',#6736,.T.);
#4536=FACE_OUTER_BOUND('',#6737,.T.);
#4537=FACE_OUTER_BOUND('',#6739,.T.);
#4538=FACE_OUTER_BOUND('',#6740,.T.);
#4539=FACE_OUTER_BOUND('',#6741,.T.);
#4540=FACE_OUTER_BOUND('',#6742,.T.);
#4541=FACE_OUTER_BOUND('',#6743,.T.);
#4542=FACE_OUTER_BOUND('',#6744,.T.);
#4543=FACE_OUTER_BOUND('',#6745,.T.);
#4544=FACE_OUTER_BOUND('',#6746,.T.);
#4545=FACE_OUTER_BOUND('',#6748,.T.);
#4546=FACE_OUTER_BOUND('',#6749,.T.);
#4547=FACE_OUTER_BOUND('',#6750,.T.);
#4548=FACE_OUTER_BOUND('',#6751,.T.);
#4549=FACE_OUTER_BOUND('',#6753,.T.);
#4550=FACE_OUTER_BOUND('',#6754,.T.);
#4551=FACE_OUTER_BOUND('',#6755,.T.);
#4552=FACE_OUTER_BOUND('',#6756,.T.);
#4553=FACE_OUTER_BOUND('',#6758,.T.);
#4554=FACE_OUTER_BOUND('',#6759,.T.);
#4555=FACE_OUTER_BOUND('',#6761,.T.);
#4556=FACE_OUTER_BOUND('',#6762,.T.);
#4557=FACE_OUTER_BOUND('',#6763,.T.);
#4558=FACE_OUTER_BOUND('',#6764,.T.);
#4559=FACE_OUTER_BOUND('',#6766,.T.);
#4560=FACE_OUTER_BOUND('',#6767,.T.);
#4561=FACE_OUTER_BOUND('',#6768,.T.);
#4562=FACE_OUTER_BOUND('',#6769,.T.);
#4563=FACE_OUTER_BOUND('',#6770,.T.);
#4564=FACE_OUTER_BOUND('',#6771,.T.);
#4565=FACE_OUTER_BOUND('',#6772,.T.);
#4566=FACE_OUTER_BOUND('',#6773,.T.);
#4567=FACE_OUTER_BOUND('',#6774,.T.);
#4568=FACE_OUTER_BOUND('',#6775,.T.);
#4569=FACE_OUTER_BOUND('',#6776,.T.);
#4570=FACE_OUTER_BOUND('',#6777,.T.);
#4571=FACE_OUTER_BOUND('',#6778,.T.);
#4572=FACE_OUTER_BOUND('',#6779,.T.);
#4573=FACE_OUTER_BOUND('',#6780,.T.);
#4574=FACE_OUTER_BOUND('',#6781,.T.);
#4575=FACE_OUTER_BOUND('',#6782,.T.);
#4576=FACE_OUTER_BOUND('',#6783,.T.);
#4577=FACE_OUTER_BOUND('',#6784,.T.);
#4578=FACE_OUTER_BOUND('',#6785,.T.);
#4579=FACE_OUTER_BOUND('',#6786,.T.);
#4580=FACE_OUTER_BOUND('',#6787,.T.);
#4581=FACE_OUTER_BOUND('',#6788,.T.);
#4582=FACE_OUTER_BOUND('',#6789,.T.);
#4583=FACE_OUTER_BOUND('',#6790,.T.);
#4584=FACE_OUTER_BOUND('',#6791,.T.);
#4585=FACE_OUTER_BOUND('',#6792,.T.);
#4586=FACE_OUTER_BOUND('',#6793,.T.);
#4587=FACE_OUTER_BOUND('',#6794,.T.);
#4588=FACE_OUTER_BOUND('',#6795,.T.);
#4589=FACE_OUTER_BOUND('',#6796,.T.);
#4590=FACE_OUTER_BOUND('',#6797,.T.);
#4591=FACE_OUTER_BOUND('',#6798,.T.);
#4592=FACE_OUTER_BOUND('',#6799,.T.);
#4593=FACE_OUTER_BOUND('',#6800,.T.);
#4594=FACE_OUTER_BOUND('',#6801,.T.);
#4595=FACE_OUTER_BOUND('',#6802,.T.);
#4596=FACE_OUTER_BOUND('',#6803,.T.);
#4597=FACE_OUTER_BOUND('',#6804,.T.);
#4598=FACE_OUTER_BOUND('',#6805,.T.);
#4599=FACE_OUTER_BOUND('',#6806,.T.);
#4600=FACE_OUTER_BOUND('',#6807,.T.);
#4601=FACE_OUTER_BOUND('',#6808,.T.);
#4602=FACE_OUTER_BOUND('',#6809,.T.);
#4603=FACE_OUTER_BOUND('',#6810,.T.);
#4604=FACE_OUTER_BOUND('',#6811,.T.);
#4605=FACE_OUTER_BOUND('',#6812,.T.);
#4606=FACE_OUTER_BOUND('',#6813,.T.);
#4607=FACE_OUTER_BOUND('',#6814,.T.);
#4608=FACE_OUTER_BOUND('',#6815,.T.);
#4609=FACE_OUTER_BOUND('',#6816,.T.);
#4610=FACE_OUTER_BOUND('',#6817,.T.);
#4611=FACE_OUTER_BOUND('',#6818,.T.);
#4612=FACE_OUTER_BOUND('',#6819,.T.);
#4613=FACE_OUTER_BOUND('',#6820,.T.);
#4614=FACE_OUTER_BOUND('',#6821,.T.);
#4615=FACE_OUTER_BOUND('',#6822,.T.);
#4616=FACE_OUTER_BOUND('',#6823,.T.);
#4617=FACE_OUTER_BOUND('',#6824,.T.);
#4618=FACE_OUTER_BOUND('',#6825,.T.);
#4619=FACE_OUTER_BOUND('',#6826,.T.);
#4620=FACE_OUTER_BOUND('',#6827,.T.);
#4621=FACE_OUTER_BOUND('',#6828,.T.);
#4622=FACE_OUTER_BOUND('',#6829,.T.);
#4623=FACE_OUTER_BOUND('',#6830,.T.);
#4624=FACE_OUTER_BOUND('',#6831,.T.);
#4625=FACE_OUTER_BOUND('',#6832,.T.);
#4626=FACE_OUTER_BOUND('',#6833,.T.);
#4627=FACE_OUTER_BOUND('',#6834,.T.);
#4628=FACE_OUTER_BOUND('',#6835,.T.);
#4629=FACE_OUTER_BOUND('',#6836,.T.);
#4630=FACE_OUTER_BOUND('',#6837,.T.);
#4631=FACE_OUTER_BOUND('',#6838,.T.);
#4632=FACE_OUTER_BOUND('',#6839,.T.);
#4633=FACE_OUTER_BOUND('',#6840,.T.);
#4634=FACE_OUTER_BOUND('',#6841,.T.);
#4635=FACE_OUTER_BOUND('',#6842,.T.);
#4636=FACE_OUTER_BOUND('',#6843,.T.);
#4637=FACE_OUTER_BOUND('',#6844,.T.);
#4638=FACE_OUTER_BOUND('',#6845,.T.);
#4639=FACE_OUTER_BOUND('',#6846,.T.);
#4640=FACE_OUTER_BOUND('',#6847,.T.);
#4641=FACE_OUTER_BOUND('',#6848,.T.);
#4642=FACE_OUTER_BOUND('',#6849,.T.);
#4643=FACE_OUTER_BOUND('',#6850,.T.);
#4644=FACE_OUTER_BOUND('',#6851,.T.);
#4645=FACE_OUTER_BOUND('',#6852,.T.);
#4646=FACE_OUTER_BOUND('',#6853,.T.);
#4647=FACE_OUTER_BOUND('',#6854,.T.);
#4648=FACE_OUTER_BOUND('',#6855,.T.);
#4649=FACE_OUTER_BOUND('',#6856,.T.);
#4650=FACE_OUTER_BOUND('',#6857,.T.);
#4651=FACE_OUTER_BOUND('',#6858,.T.);
#4652=FACE_OUTER_BOUND('',#6859,.T.);
#4653=FACE_OUTER_BOUND('',#6860,.T.);
#4654=FACE_OUTER_BOUND('',#6861,.T.);
#4655=FACE_OUTER_BOUND('',#6862,.T.);
#4656=FACE_OUTER_BOUND('',#6863,.T.);
#4657=FACE_OUTER_BOUND('',#6864,.T.);
#4658=FACE_OUTER_BOUND('',#6865,.T.);
#4659=FACE_OUTER_BOUND('',#6866,.T.);
#4660=FACE_OUTER_BOUND('',#6867,.T.);
#4661=FACE_OUTER_BOUND('',#6868,.T.);
#4662=FACE_OUTER_BOUND('',#6869,.T.);
#4663=FACE_OUTER_BOUND('',#6870,.T.);
#4664=FACE_OUTER_BOUND('',#6871,.T.);
#4665=FACE_OUTER_BOUND('',#6872,.T.);
#4666=FACE_OUTER_BOUND('',#6873,.T.);
#4667=FACE_OUTER_BOUND('',#6874,.T.);
#4668=FACE_OUTER_BOUND('',#6875,.T.);
#4669=FACE_OUTER_BOUND('',#6876,.T.);
#4670=FACE_OUTER_BOUND('',#6877,.T.);
#4671=FACE_OUTER_BOUND('',#6899,.T.);
#4672=FACE_OUTER_BOUND('',#6900,.T.);
#4673=FACE_OUTER_BOUND('',#6902,.T.);
#4674=FACE_OUTER_BOUND('',#6903,.T.);
#4675=FACE_OUTER_BOUND('',#6904,.T.);
#4676=FACE_OUTER_BOUND('',#6905,.T.);
#4677=FACE_OUTER_BOUND('',#6907,.T.);
#4678=FACE_OUTER_BOUND('',#6908,.T.);
#4679=FACE_OUTER_BOUND('',#6909,.T.);
#4680=FACE_OUTER_BOUND('',#6910,.T.);
#4681=FACE_OUTER_BOUND('',#6912,.T.);
#4682=FACE_OUTER_BOUND('',#6913,.T.);
#4683=FACE_OUTER_BOUND('',#6914,.T.);
#4684=FACE_OUTER_BOUND('',#6915,.T.);
#4685=FACE_OUTER_BOUND('',#6917,.T.);
#4686=FACE_OUTER_BOUND('',#6918,.T.);
#4687=FACE_OUTER_BOUND('',#6920,.T.);
#4688=FACE_OUTER_BOUND('',#6921,.T.);
#4689=FACE_OUTER_BOUND('',#6922,.T.);
#4690=FACE_OUTER_BOUND('',#6923,.T.);
#4691=FACE_OUTER_BOUND('',#6925,.T.);
#4692=FACE_OUTER_BOUND('',#6926,.T.);
#4693=FACE_OUTER_BOUND('',#6927,.T.);
#4694=FACE_OUTER_BOUND('',#6928,.T.);
#4695=FACE_OUTER_BOUND('',#6929,.T.);
#4696=FACE_OUTER_BOUND('',#6930,.T.);
#4697=FACE_OUTER_BOUND('',#6931,.T.);
#4698=FACE_OUTER_BOUND('',#6932,.T.);
#4699=FACE_OUTER_BOUND('',#6933,.T.);
#4700=FACE_OUTER_BOUND('',#6934,.T.);
#4701=FACE_OUTER_BOUND('',#6935,.T.);
#4702=FACE_OUTER_BOUND('',#6936,.T.);
#4703=FACE_OUTER_BOUND('',#6937,.T.);
#4704=FACE_OUTER_BOUND('',#6938,.T.);
#4705=FACE_OUTER_BOUND('',#6939,.T.);
#4706=FACE_OUTER_BOUND('',#6940,.T.);
#4707=FACE_OUTER_BOUND('',#6941,.T.);
#4708=FACE_OUTER_BOUND('',#6942,.T.);
#4709=FACE_OUTER_BOUND('',#6943,.T.);
#4710=FACE_OUTER_BOUND('',#6944,.T.);
#4711=FACE_OUTER_BOUND('',#6945,.T.);
#4712=FACE_OUTER_BOUND('',#6946,.T.);
#4713=FACE_OUTER_BOUND('',#6947,.T.);
#4714=FACE_OUTER_BOUND('',#6948,.T.);
#4715=FACE_OUTER_BOUND('',#6949,.T.);
#4716=FACE_OUTER_BOUND('',#6950,.T.);
#4717=FACE_OUTER_BOUND('',#6951,.T.);
#4718=FACE_OUTER_BOUND('',#6952,.T.);
#4719=FACE_OUTER_BOUND('',#6953,.T.);
#4720=FACE_OUTER_BOUND('',#6954,.T.);
#4721=FACE_OUTER_BOUND('',#6955,.T.);
#4722=FACE_OUTER_BOUND('',#6956,.T.);
#4723=FACE_OUTER_BOUND('',#6957,.T.);
#4724=FACE_OUTER_BOUND('',#6958,.T.);
#4725=FACE_OUTER_BOUND('',#6959,.T.);
#4726=FACE_OUTER_BOUND('',#6960,.T.);
#4727=FACE_OUTER_BOUND('',#6961,.T.);
#4728=FACE_OUTER_BOUND('',#6962,.T.);
#4729=FACE_OUTER_BOUND('',#6963,.T.);
#4730=FACE_OUTER_BOUND('',#6964,.T.);
#4731=FACE_OUTER_BOUND('',#6965,.T.);
#4732=FACE_OUTER_BOUND('',#6966,.T.);
#4733=FACE_OUTER_BOUND('',#6967,.T.);
#4734=FACE_OUTER_BOUND('',#6968,.T.);
#4735=FACE_OUTER_BOUND('',#6969,.T.);
#4736=FACE_OUTER_BOUND('',#6970,.T.);
#4737=FACE_OUTER_BOUND('',#6971,.T.);
#4738=FACE_OUTER_BOUND('',#6972,.T.);
#4739=FACE_OUTER_BOUND('',#6973,.T.);
#4740=FACE_OUTER_BOUND('',#6974,.T.);
#4741=FACE_OUTER_BOUND('',#6975,.T.);
#4742=FACE_OUTER_BOUND('',#6976,.T.);
#4743=FACE_OUTER_BOUND('',#6977,.T.);
#4744=FACE_OUTER_BOUND('',#6978,.T.);
#4745=FACE_OUTER_BOUND('',#6979,.T.);
#4746=FACE_OUTER_BOUND('',#6980,.T.);
#4747=FACE_OUTER_BOUND('',#6981,.T.);
#4748=FACE_OUTER_BOUND('',#6982,.T.);
#4749=FACE_OUTER_BOUND('',#6983,.T.);
#4750=FACE_OUTER_BOUND('',#6984,.T.);
#4751=FACE_OUTER_BOUND('',#6985,.T.);
#4752=FACE_OUTER_BOUND('',#6986,.T.);
#4753=FACE_OUTER_BOUND('',#6987,.T.);
#4754=FACE_OUTER_BOUND('',#6988,.T.);
#4755=FACE_OUTER_BOUND('',#6989,.T.);
#4756=FACE_OUTER_BOUND('',#6990,.T.);
#4757=FACE_OUTER_BOUND('',#6991,.T.);
#4758=FACE_OUTER_BOUND('',#6992,.T.);
#4759=FACE_OUTER_BOUND('',#6993,.T.);
#4760=FACE_OUTER_BOUND('',#6994,.T.);
#4761=FACE_OUTER_BOUND('',#6995,.T.);
#4762=FACE_OUTER_BOUND('',#6996,.T.);
#4763=FACE_OUTER_BOUND('',#6997,.T.);
#4764=FACE_OUTER_BOUND('',#6998,.T.);
#4765=FACE_OUTER_BOUND('',#6999,.T.);
#4766=FACE_OUTER_BOUND('',#7000,.T.);
#4767=FACE_OUTER_BOUND('',#7001,.T.);
#4768=FACE_OUTER_BOUND('',#7002,.T.);
#4769=FACE_OUTER_BOUND('',#7003,.T.);
#4770=FACE_OUTER_BOUND('',#7004,.T.);
#4771=FACE_OUTER_BOUND('',#7005,.T.);
#4772=FACE_OUTER_BOUND('',#7006,.T.);
#4773=FACE_OUTER_BOUND('',#7007,.T.);
#4774=FACE_OUTER_BOUND('',#7008,.T.);
#4775=FACE_OUTER_BOUND('',#7009,.T.);
#4776=FACE_OUTER_BOUND('',#7010,.T.);
#4777=FACE_OUTER_BOUND('',#7011,.T.);
#4778=FACE_OUTER_BOUND('',#7012,.T.);
#4779=FACE_OUTER_BOUND('',#7013,.T.);
#4780=FACE_OUTER_BOUND('',#7014,.T.);
#4781=FACE_OUTER_BOUND('',#7015,.T.);
#4782=FACE_OUTER_BOUND('',#7016,.T.);
#4783=FACE_OUTER_BOUND('',#7017,.T.);
#4784=FACE_OUTER_BOUND('',#7018,.T.);
#4785=FACE_OUTER_BOUND('',#7019,.T.);
#4786=FACE_OUTER_BOUND('',#7020,.T.);
#4787=FACE_OUTER_BOUND('',#7021,.T.);
#4788=FACE_OUTER_BOUND('',#7022,.T.);
#4789=FACE_OUTER_BOUND('',#7023,.T.);
#4790=FACE_OUTER_BOUND('',#7024,.T.);
#4791=FACE_OUTER_BOUND('',#7025,.T.);
#4792=FACE_OUTER_BOUND('',#7026,.T.);
#4793=FACE_OUTER_BOUND('',#7046,.T.);
#4794=FACE_OUTER_BOUND('',#7047,.T.);
#4795=FACE_OUTER_BOUND('',#7049,.T.);
#4796=FACE_OUTER_BOUND('',#7050,.T.);
#4797=FACE_OUTER_BOUND('',#7051,.T.);
#4798=FACE_OUTER_BOUND('',#7052,.T.);
#4799=FACE_OUTER_BOUND('',#7054,.T.);
#4800=FACE_OUTER_BOUND('',#7055,.T.);
#4801=FACE_OUTER_BOUND('',#7056,.T.);
#4802=FACE_OUTER_BOUND('',#7057,.T.);
#4803=FACE_OUTER_BOUND('',#7058,.T.);
#4804=FACE_OUTER_BOUND('',#7059,.T.);
#4805=FACE_OUTER_BOUND('',#7061,.T.);
#4806=FACE_OUTER_BOUND('',#7062,.T.);
#4807=FACE_OUTER_BOUND('',#7064,.T.);
#4808=FACE_OUTER_BOUND('',#7065,.T.);
#4809=FACE_OUTER_BOUND('',#7066,.T.);
#4810=FACE_OUTER_BOUND('',#7067,.T.);
#4811=FACE_OUTER_BOUND('',#7068,.T.);
#4812=FACE_OUTER_BOUND('',#7069,.T.);
#4813=FACE_OUTER_BOUND('',#7070,.T.);
#4814=FACE_OUTER_BOUND('',#7071,.T.);
#4815=FACE_OUTER_BOUND('',#7072,.T.);
#4816=FACE_OUTER_BOUND('',#7073,.T.);
#4817=FACE_OUTER_BOUND('',#7074,.T.);
#4818=FACE_OUTER_BOUND('',#7075,.T.);
#4819=FACE_OUTER_BOUND('',#7076,.T.);
#4820=FACE_OUTER_BOUND('',#7077,.T.);
#4821=FACE_OUTER_BOUND('',#7078,.T.);
#4822=FACE_OUTER_BOUND('',#7079,.T.);
#4823=FACE_OUTER_BOUND('',#7080,.T.);
#4824=FACE_OUTER_BOUND('',#7081,.T.);
#4825=FACE_OUTER_BOUND('',#7082,.T.);
#4826=FACE_OUTER_BOUND('',#7083,.T.);
#4827=FACE_OUTER_BOUND('',#7084,.T.);
#4828=FACE_OUTER_BOUND('',#7085,.T.);
#4829=FACE_OUTER_BOUND('',#7086,.T.);
#4830=FACE_OUTER_BOUND('',#7087,.T.);
#4831=FACE_OUTER_BOUND('',#7088,.T.);
#4832=FACE_OUTER_BOUND('',#7089,.T.);
#4833=FACE_OUTER_BOUND('',#7090,.T.);
#4834=FACE_OUTER_BOUND('',#7091,.T.);
#4835=FACE_OUTER_BOUND('',#7092,.T.);
#4836=FACE_OUTER_BOUND('',#7093,.T.);
#4837=FACE_OUTER_BOUND('',#7094,.T.);
#4838=FACE_OUTER_BOUND('',#7095,.T.);
#4839=FACE_OUTER_BOUND('',#7096,.T.);
#4840=FACE_OUTER_BOUND('',#7097,.T.);
#4841=FACE_OUTER_BOUND('',#7098,.T.);
#4842=FACE_OUTER_BOUND('',#7099,.T.);
#4843=FACE_OUTER_BOUND('',#7100,.T.);
#4844=FACE_OUTER_BOUND('',#7101,.T.);
#4845=FACE_OUTER_BOUND('',#7102,.T.);
#4846=FACE_OUTER_BOUND('',#7103,.T.);
#4847=FACE_OUTER_BOUND('',#7104,.T.);
#4848=FACE_OUTER_BOUND('',#7105,.T.);
#4849=FACE_OUTER_BOUND('',#7106,.T.);
#4850=FACE_OUTER_BOUND('',#7107,.T.);
#4851=FACE_OUTER_BOUND('',#7108,.T.);
#4852=FACE_OUTER_BOUND('',#7109,.T.);
#4853=FACE_OUTER_BOUND('',#7110,.T.);
#4854=FACE_OUTER_BOUND('',#7111,.T.);
#4855=FACE_OUTER_BOUND('',#7112,.T.);
#4856=FACE_OUTER_BOUND('',#7113,.T.);
#4857=FACE_OUTER_BOUND('',#7114,.T.);
#4858=FACE_OUTER_BOUND('',#7115,.T.);
#4859=FACE_OUTER_BOUND('',#7116,.T.);
#4860=FACE_OUTER_BOUND('',#7117,.T.);
#4861=FACE_OUTER_BOUND('',#7118,.T.);
#4862=FACE_OUTER_BOUND('',#7119,.T.);
#4863=FACE_OUTER_BOUND('',#7120,.T.);
#4864=FACE_OUTER_BOUND('',#7121,.T.);
#4865=FACE_OUTER_BOUND('',#7122,.T.);
#4866=FACE_OUTER_BOUND('',#7123,.T.);
#4867=FACE_OUTER_BOUND('',#7124,.T.);
#4868=FACE_OUTER_BOUND('',#7125,.T.);
#4869=FACE_OUTER_BOUND('',#7126,.T.);
#4870=FACE_OUTER_BOUND('',#7127,.T.);
#4871=FACE_OUTER_BOUND('',#7128,.T.);
#4872=FACE_OUTER_BOUND('',#7129,.T.);
#4873=FACE_OUTER_BOUND('',#7130,.T.);
#4874=FACE_OUTER_BOUND('',#7131,.T.);
#4875=FACE_OUTER_BOUND('',#7132,.T.);
#4876=FACE_OUTER_BOUND('',#7133,.T.);
#4877=FACE_OUTER_BOUND('',#7134,.T.);
#4878=FACE_OUTER_BOUND('',#7135,.T.);
#4879=FACE_OUTER_BOUND('',#7136,.T.);
#4880=FACE_OUTER_BOUND('',#7137,.T.);
#4881=FACE_OUTER_BOUND('',#7138,.T.);
#4882=FACE_OUTER_BOUND('',#7139,.T.);
#4883=FACE_OUTER_BOUND('',#7140,.T.);
#4884=FACE_OUTER_BOUND('',#7141,.T.);
#4885=FACE_OUTER_BOUND('',#7142,.T.);
#4886=FACE_OUTER_BOUND('',#7143,.T.);
#4887=FACE_OUTER_BOUND('',#7144,.T.);
#4888=FACE_OUTER_BOUND('',#7145,.T.);
#4889=FACE_OUTER_BOUND('',#7146,.T.);
#4890=FACE_OUTER_BOUND('',#7147,.T.);
#4891=FACE_OUTER_BOUND('',#7148,.T.);
#4892=FACE_OUTER_BOUND('',#7149,.T.);
#4893=FACE_OUTER_BOUND('',#7150,.T.);
#4894=FACE_OUTER_BOUND('',#7151,.T.);
#4895=FACE_OUTER_BOUND('',#7152,.T.);
#4896=FACE_OUTER_BOUND('',#7153,.T.);
#4897=FACE_OUTER_BOUND('',#7154,.T.);
#4898=FACE_OUTER_BOUND('',#7155,.T.);
#4899=FACE_OUTER_BOUND('',#7156,.T.);
#4900=FACE_OUTER_BOUND('',#7157,.T.);
#4901=FACE_OUTER_BOUND('',#7158,.T.);
#4902=FACE_OUTER_BOUND('',#7159,.T.);
#4903=FACE_OUTER_BOUND('',#7160,.T.);
#4904=FACE_OUTER_BOUND('',#7161,.T.);
#4905=FACE_OUTER_BOUND('',#7162,.T.);
#4906=FACE_OUTER_BOUND('',#7163,.T.);
#4907=FACE_OUTER_BOUND('',#7164,.T.);
#4908=FACE_OUTER_BOUND('',#7165,.T.);
#4909=FACE_OUTER_BOUND('',#7166,.T.);
#4910=FACE_OUTER_BOUND('',#7167,.T.);
#4911=FACE_OUTER_BOUND('',#7168,.T.);
#4912=FACE_OUTER_BOUND('',#7169,.T.);
#4913=FACE_OUTER_BOUND('',#7170,.T.);
#4914=FACE_OUTER_BOUND('',#7171,.T.);
#4915=FACE_OUTER_BOUND('',#7172,.T.);
#4916=FACE_OUTER_BOUND('',#7173,.T.);
#4917=FACE_OUTER_BOUND('',#7174,.T.);
#4918=FACE_OUTER_BOUND('',#7175,.T.);
#4919=FACE_OUTER_BOUND('',#7176,.T.);
#4920=FACE_OUTER_BOUND('',#7177,.T.);
#4921=FACE_OUTER_BOUND('',#7178,.T.);
#4922=FACE_OUTER_BOUND('',#7180,.T.);
#4923=FACE_OUTER_BOUND('',#7181,.T.);
#4924=FACE_OUTER_BOUND('',#7182,.T.);
#4925=FACE_OUTER_BOUND('',#7183,.T.);
#4926=FACE_OUTER_BOUND('',#7184,.T.);
#4927=FACE_OUTER_BOUND('',#7185,.T.);
#4928=FACE_OUTER_BOUND('',#7186,.T.);
#4929=FACE_OUTER_BOUND('',#7187,.T.);
#4930=FACE_OUTER_BOUND('',#7188,.T.);
#4931=FACE_OUTER_BOUND('',#7189,.T.);
#4932=FACE_OUTER_BOUND('',#7190,.T.);
#4933=FACE_OUTER_BOUND('',#7191,.T.);
#4934=FACE_OUTER_BOUND('',#7192,.T.);
#4935=FACE_OUTER_BOUND('',#7193,.T.);
#4936=FACE_OUTER_BOUND('',#7194,.T.);
#4937=FACE_OUTER_BOUND('',#7195,.T.);
#4938=FACE_OUTER_BOUND('',#7197,.T.);
#4939=FACE_OUTER_BOUND('',#7198,.T.);
#4940=FACE_OUTER_BOUND('',#7199,.T.);
#4941=FACE_OUTER_BOUND('',#7200,.T.);
#4942=FACE_OUTER_BOUND('',#7201,.T.);
#4943=FACE_OUTER_BOUND('',#7202,.T.);
#4944=FACE_OUTER_BOUND('',#7203,.T.);
#4945=FACE_OUTER_BOUND('',#7204,.T.);
#4946=FACE_OUTER_BOUND('',#7205,.T.);
#4947=FACE_OUTER_BOUND('',#7206,.T.);
#4948=FACE_OUTER_BOUND('',#7207,.T.);
#4949=FACE_OUTER_BOUND('',#7209,.T.);
#4950=FACE_OUTER_BOUND('',#7210,.T.);
#4951=FACE_OUTER_BOUND('',#7211,.T.);
#4952=FACE_OUTER_BOUND('',#7213,.T.);
#4953=FACE_OUTER_BOUND('',#7214,.T.);
#4954=FACE_OUTER_BOUND('',#7215,.T.);
#4955=FACE_OUTER_BOUND('',#7216,.T.);
#4956=FACE_OUTER_BOUND('',#7217,.T.);
#4957=FACE_OUTER_BOUND('',#7218,.T.);
#4958=FACE_OUTER_BOUND('',#7219,.T.);
#4959=FACE_OUTER_BOUND('',#7220,.T.);
#4960=FACE_OUTER_BOUND('',#7221,.T.);
#4961=FACE_OUTER_BOUND('',#7222,.T.);
#4962=FACE_OUTER_BOUND('',#7223,.T.);
#4963=FACE_OUTER_BOUND('',#7224,.T.);
#4964=FACE_OUTER_BOUND('',#7225,.T.);
#4965=FACE_OUTER_BOUND('',#7226,.T.);
#4966=FACE_OUTER_BOUND('',#7227,.T.);
#4967=FACE_OUTER_BOUND('',#7228,.T.);
#4968=FACE_OUTER_BOUND('',#7229,.T.);
#4969=FACE_OUTER_BOUND('',#7230,.T.);
#4970=FACE_OUTER_BOUND('',#7231,.T.);
#4971=FACE_OUTER_BOUND('',#7232,.T.);
#4972=FACE_OUTER_BOUND('',#7233,.T.);
#4973=FACE_OUTER_BOUND('',#7234,.T.);
#4974=FACE_OUTER_BOUND('',#7235,.T.);
#4975=FACE_OUTER_BOUND('',#7236,.T.);
#4976=FACE_OUTER_BOUND('',#7237,.T.);
#4977=FACE_OUTER_BOUND('',#7238,.T.);
#4978=FACE_OUTER_BOUND('',#7239,.T.);
#4979=FACE_OUTER_BOUND('',#7240,.T.);
#4980=FACE_OUTER_BOUND('',#7241,.T.);
#4981=FACE_OUTER_BOUND('',#7242,.T.);
#4982=FACE_OUTER_BOUND('',#7243,.T.);
#4983=FACE_OUTER_BOUND('',#7244,.T.);
#4984=FACE_OUTER_BOUND('',#7245,.T.);
#4985=FACE_OUTER_BOUND('',#7246,.T.);
#4986=FACE_OUTER_BOUND('',#7247,.T.);
#4987=FACE_OUTER_BOUND('',#7248,.T.);
#4988=FACE_OUTER_BOUND('',#7249,.T.);
#4989=FACE_OUTER_BOUND('',#7250,.T.);
#4990=FACE_OUTER_BOUND('',#7251,.T.);
#4991=FACE_OUTER_BOUND('',#7252,.T.);
#4992=FACE_OUTER_BOUND('',#7253,.T.);
#4993=FACE_OUTER_BOUND('',#7254,.T.);
#4994=FACE_OUTER_BOUND('',#7255,.T.);
#4995=FACE_OUTER_BOUND('',#7256,.T.);
#4996=FACE_OUTER_BOUND('',#7257,.T.);
#4997=FACE_OUTER_BOUND('',#7258,.T.);
#4998=FACE_OUTER_BOUND('',#7259,.T.);
#4999=FACE_OUTER_BOUND('',#7260,.T.);
#5000=FACE_OUTER_BOUND('',#7261,.T.);
#5001=FACE_OUTER_BOUND('',#7262,.T.);
#5002=FACE_OUTER_BOUND('',#7263,.T.);
#5003=FACE_OUTER_BOUND('',#7264,.T.);
#5004=FACE_OUTER_BOUND('',#7265,.T.);
#5005=FACE_OUTER_BOUND('',#7266,.T.);
#5006=FACE_OUTER_BOUND('',#7267,.T.);
#5007=FACE_OUTER_BOUND('',#7268,.T.);
#5008=FACE_OUTER_BOUND('',#7269,.T.);
#5009=FACE_OUTER_BOUND('',#7270,.T.);
#5010=FACE_OUTER_BOUND('',#7271,.T.);
#5011=FACE_OUTER_BOUND('',#7272,.T.);
#5012=FACE_OUTER_BOUND('',#7273,.T.);
#5013=FACE_OUTER_BOUND('',#7274,.T.);
#5014=FACE_OUTER_BOUND('',#7275,.T.);
#5015=FACE_OUTER_BOUND('',#7276,.T.);
#5016=FACE_OUTER_BOUND('',#7277,.T.);
#5017=FACE_OUTER_BOUND('',#7278,.T.);
#5018=FACE_OUTER_BOUND('',#7279,.T.);
#5019=FACE_OUTER_BOUND('',#7280,.T.);
#5020=FACE_OUTER_BOUND('',#7281,.T.);
#5021=FACE_OUTER_BOUND('',#7282,.T.);
#5022=FACE_OUTER_BOUND('',#7283,.T.);
#5023=FACE_OUTER_BOUND('',#7284,.T.);
#5024=FACE_OUTER_BOUND('',#7285,.T.);
#5025=FACE_OUTER_BOUND('',#7287,.T.);
#5026=FACE_OUTER_BOUND('',#7288,.T.);
#5027=FACE_OUTER_BOUND('',#7289,.T.);
#5028=FACE_OUTER_BOUND('',#7290,.T.);
#5029=FACE_OUTER_BOUND('',#7291,.T.);
#5030=FACE_OUTER_BOUND('',#7292,.T.);
#5031=FACE_OUTER_BOUND('',#7293,.T.);
#5032=FACE_OUTER_BOUND('',#7294,.T.);
#5033=FACE_OUTER_BOUND('',#7295,.T.);
#5034=FACE_OUTER_BOUND('',#7296,.T.);
#5035=FACE_OUTER_BOUND('',#7297,.T.);
#5036=FACE_OUTER_BOUND('',#7298,.T.);
#5037=FACE_OUTER_BOUND('',#7299,.T.);
#5038=FACE_OUTER_BOUND('',#7300,.T.);
#5039=FACE_OUTER_BOUND('',#7301,.T.);
#5040=FACE_OUTER_BOUND('',#7302,.T.);
#5041=FACE_OUTER_BOUND('',#7303,.T.);
#5042=FACE_OUTER_BOUND('',#7304,.T.);
#5043=FACE_OUTER_BOUND('',#7305,.T.);
#5044=FACE_OUTER_BOUND('',#7306,.T.);
#5045=FACE_OUTER_BOUND('',#7307,.T.);
#5046=FACE_OUTER_BOUND('',#7308,.T.);
#5047=FACE_OUTER_BOUND('',#7309,.T.);
#5048=FACE_OUTER_BOUND('',#7310,.T.);
#5049=FACE_OUTER_BOUND('',#7311,.T.);
#5050=FACE_OUTER_BOUND('',#7312,.T.);
#5051=FACE_OUTER_BOUND('',#7313,.T.);
#5052=FACE_OUTER_BOUND('',#7314,.T.);
#5053=FACE_OUTER_BOUND('',#7315,.T.);
#5054=FACE_OUTER_BOUND('',#7316,.T.);
#5055=FACE_OUTER_BOUND('',#7317,.T.);
#5056=FACE_OUTER_BOUND('',#7318,.T.);
#5057=FACE_OUTER_BOUND('',#7319,.T.);
#5058=FACE_OUTER_BOUND('',#7320,.T.);
#5059=FACE_OUTER_BOUND('',#7321,.T.);
#5060=FACE_OUTER_BOUND('',#7322,.T.);
#5061=FACE_OUTER_BOUND('',#7323,.T.);
#5062=FACE_OUTER_BOUND('',#7324,.T.);
#5063=FACE_OUTER_BOUND('',#7325,.T.);
#5064=FACE_OUTER_BOUND('',#7326,.T.);
#5065=FACE_OUTER_BOUND('',#7327,.T.);
#5066=FACE_OUTER_BOUND('',#7328,.T.);
#5067=FACE_OUTER_BOUND('',#7329,.T.);
#5068=FACE_OUTER_BOUND('',#7330,.T.);
#5069=FACE_OUTER_BOUND('',#7331,.T.);
#5070=FACE_OUTER_BOUND('',#7332,.T.);
#5071=FACE_OUTER_BOUND('',#7333,.T.);
#5072=FACE_OUTER_BOUND('',#7334,.T.);
#5073=FACE_OUTER_BOUND('',#7335,.T.);
#5074=FACE_OUTER_BOUND('',#7336,.T.);
#5075=FACE_OUTER_BOUND('',#7337,.T.);
#5076=FACE_OUTER_BOUND('',#7338,.T.);
#5077=FACE_OUTER_BOUND('',#7339,.T.);
#5078=FACE_OUTER_BOUND('',#7340,.T.);
#5079=FACE_OUTER_BOUND('',#7341,.T.);
#5080=FACE_OUTER_BOUND('',#7342,.T.);
#5081=FACE_OUTER_BOUND('',#7343,.T.);
#5082=FACE_OUTER_BOUND('',#7344,.T.);
#5083=FACE_OUTER_BOUND('',#7345,.T.);
#5084=FACE_OUTER_BOUND('',#7346,.T.);
#5085=FACE_OUTER_BOUND('',#7347,.T.);
#5086=FACE_OUTER_BOUND('',#7348,.T.);
#5087=FACE_OUTER_BOUND('',#7349,.T.);
#5088=FACE_OUTER_BOUND('',#7350,.T.);
#5089=FACE_OUTER_BOUND('',#7351,.T.);
#5090=FACE_OUTER_BOUND('',#7352,.T.);
#5091=FACE_OUTER_BOUND('',#7353,.T.);
#5092=FACE_OUTER_BOUND('',#7354,.T.);
#5093=FACE_OUTER_BOUND('',#7355,.T.);
#5094=FACE_OUTER_BOUND('',#7356,.T.);
#5095=FACE_OUTER_BOUND('',#7357,.T.);
#5096=FACE_OUTER_BOUND('',#7358,.T.);
#5097=FACE_OUTER_BOUND('',#7359,.T.);
#5098=FACE_OUTER_BOUND('',#7360,.T.);
#5099=FACE_OUTER_BOUND('',#7361,.T.);
#5100=FACE_OUTER_BOUND('',#7362,.T.);
#5101=FACE_OUTER_BOUND('',#7363,.T.);
#5102=FACE_OUTER_BOUND('',#7364,.T.);
#5103=FACE_OUTER_BOUND('',#7365,.T.);
#5104=FACE_OUTER_BOUND('',#7366,.T.);
#5105=FACE_OUTER_BOUND('',#7367,.T.);
#5106=FACE_OUTER_BOUND('',#7368,.T.);
#5107=FACE_OUTER_BOUND('',#7369,.T.);
#5108=FACE_OUTER_BOUND('',#7370,.T.);
#5109=FACE_OUTER_BOUND('',#7371,.T.);
#5110=FACE_OUTER_BOUND('',#7372,.T.);
#5111=FACE_OUTER_BOUND('',#7373,.T.);
#5112=FACE_OUTER_BOUND('',#7374,.T.);
#5113=FACE_OUTER_BOUND('',#7375,.T.);
#5114=FACE_OUTER_BOUND('',#7376,.T.);
#5115=FACE_OUTER_BOUND('',#7377,.T.);
#5116=FACE_OUTER_BOUND('',#7378,.T.);
#5117=FACE_OUTER_BOUND('',#7379,.T.);
#5118=FACE_OUTER_BOUND('',#7380,.T.);
#5119=FACE_OUTER_BOUND('',#7381,.T.);
#5120=FACE_OUTER_BOUND('',#7382,.T.);
#5121=FACE_OUTER_BOUND('',#7383,.T.);
#5122=FACE_OUTER_BOUND('',#7384,.T.);
#5123=FACE_OUTER_BOUND('',#7385,.T.);
#5124=FACE_OUTER_BOUND('',#7386,.T.);
#5125=FACE_OUTER_BOUND('',#7387,.T.);
#5126=FACE_OUTER_BOUND('',#7388,.T.);
#5127=FACE_OUTER_BOUND('',#7389,.T.);
#5128=FACE_OUTER_BOUND('',#7390,.T.);
#5129=FACE_OUTER_BOUND('',#7391,.T.);
#5130=FACE_OUTER_BOUND('',#7392,.T.);
#5131=FACE_OUTER_BOUND('',#7393,.T.);
#5132=FACE_OUTER_BOUND('',#7394,.T.);
#5133=FACE_OUTER_BOUND('',#7395,.T.);
#5134=FACE_OUTER_BOUND('',#7396,.T.);
#5135=FACE_OUTER_BOUND('',#7397,.T.);
#5136=FACE_OUTER_BOUND('',#7398,.T.);
#5137=FACE_OUTER_BOUND('',#7399,.T.);
#5138=FACE_OUTER_BOUND('',#7400,.T.);
#5139=FACE_OUTER_BOUND('',#7401,.T.);
#5140=FACE_OUTER_BOUND('',#7402,.T.);
#5141=FACE_OUTER_BOUND('',#7403,.T.);
#5142=FACE_OUTER_BOUND('',#7404,.T.);
#5143=FACE_OUTER_BOUND('',#7405,.T.);
#5144=FACE_OUTER_BOUND('',#7406,.T.);
#5145=FACE_OUTER_BOUND('',#7407,.T.);
#5146=FACE_OUTER_BOUND('',#7408,.T.);
#5147=FACE_OUTER_BOUND('',#7409,.T.);
#5148=FACE_OUTER_BOUND('',#7410,.T.);
#5149=FACE_OUTER_BOUND('',#7411,.T.);
#5150=FACE_OUTER_BOUND('',#7412,.T.);
#5151=FACE_OUTER_BOUND('',#7413,.T.);
#5152=FACE_OUTER_BOUND('',#7414,.T.);
#5153=FACE_OUTER_BOUND('',#7415,.T.);
#5154=FACE_OUTER_BOUND('',#7416,.T.);
#5155=FACE_OUTER_BOUND('',#7417,.T.);
#5156=FACE_OUTER_BOUND('',#7418,.T.);
#5157=FACE_OUTER_BOUND('',#7419,.T.);
#5158=FACE_OUTER_BOUND('',#7420,.T.);
#5159=FACE_OUTER_BOUND('',#7421,.T.);
#5160=FACE_OUTER_BOUND('',#7422,.T.);
#5161=FACE_OUTER_BOUND('',#7423,.T.);
#5162=FACE_OUTER_BOUND('',#7424,.T.);
#5163=FACE_OUTER_BOUND('',#7425,.T.);
#5164=FACE_OUTER_BOUND('',#7426,.T.);
#5165=FACE_OUTER_BOUND('',#7427,.T.);
#5166=FACE_OUTER_BOUND('',#7428,.T.);
#5167=FACE_OUTER_BOUND('',#7429,.T.);
#5168=FACE_OUTER_BOUND('',#7430,.T.);
#5169=FACE_OUTER_BOUND('',#7431,.T.);
#5170=FACE_OUTER_BOUND('',#7432,.T.);
#5171=FACE_OUTER_BOUND('',#7433,.T.);
#5172=FACE_OUTER_BOUND('',#7434,.T.);
#5173=FACE_OUTER_BOUND('',#7435,.T.);
#5174=FACE_OUTER_BOUND('',#7436,.T.);
#5175=FACE_OUTER_BOUND('',#7437,.T.);
#5176=FACE_OUTER_BOUND('',#7438,.T.);
#5177=FACE_OUTER_BOUND('',#7439,.T.);
#5178=FACE_OUTER_BOUND('',#7440,.T.);
#5179=FACE_OUTER_BOUND('',#7441,.T.);
#5180=FACE_OUTER_BOUND('',#7442,.T.);
#5181=FACE_OUTER_BOUND('',#7443,.T.);
#5182=FACE_OUTER_BOUND('',#7444,.T.);
#5183=FACE_OUTER_BOUND('',#7445,.T.);
#5184=FACE_OUTER_BOUND('',#7481,.T.);
#5185=FACE_OUTER_BOUND('',#7482,.T.);
#5186=FACE_OUTER_BOUND('',#7483,.T.);
#5187=FACE_OUTER_BOUND('',#7484,.T.);
#5188=FACE_OUTER_BOUND('',#7485,.T.);
#5189=FACE_OUTER_BOUND('',#7486,.T.);
#5190=FACE_OUTER_BOUND('',#7487,.T.);
#5191=FACE_OUTER_BOUND('',#7488,.T.);
#5192=FACE_OUTER_BOUND('',#7489,.T.);
#5193=FACE_OUTER_BOUND('',#7490,.T.);
#5194=FACE_OUTER_BOUND('',#7491,.T.);
#5195=FACE_OUTER_BOUND('',#7492,.T.);
#5196=FACE_OUTER_BOUND('',#7494,.T.);
#5197=FACE_OUTER_BOUND('',#7495,.T.);
#5198=FACE_OUTER_BOUND('',#7496,.T.);
#5199=FACE_OUTER_BOUND('',#7497,.T.);
#5200=FACE_OUTER_BOUND('',#7498,.T.);
#5201=FACE_OUTER_BOUND('',#7499,.T.);
#5202=FACE_OUTER_BOUND('',#7500,.T.);
#5203=FACE_OUTER_BOUND('',#7501,.T.);
#5204=FACE_OUTER_BOUND('',#7502,.T.);
#5205=FACE_OUTER_BOUND('',#7503,.T.);
#5206=FACE_OUTER_BOUND('',#7504,.T.);
#5207=FACE_OUTER_BOUND('',#7505,.T.);
#5208=FACE_OUTER_BOUND('',#7506,.T.);
#5209=FACE_OUTER_BOUND('',#7507,.T.);
#5210=FACE_OUTER_BOUND('',#7508,.T.);
#5211=FACE_OUTER_BOUND('',#7509,.T.);
#5212=FACE_OUTER_BOUND('',#7510,.T.);
#5213=FACE_OUTER_BOUND('',#7511,.T.);
#5214=FACE_OUTER_BOUND('',#7512,.T.);
#5215=FACE_OUTER_BOUND('',#7513,.T.);
#5216=FACE_OUTER_BOUND('',#7514,.T.);
#5217=FACE_OUTER_BOUND('',#7515,.T.);
#5218=FACE_OUTER_BOUND('',#7516,.T.);
#5219=FACE_OUTER_BOUND('',#7517,.T.);
#5220=FACE_OUTER_BOUND('',#7518,.T.);
#5221=FACE_OUTER_BOUND('',#7519,.T.);
#5222=FACE_OUTER_BOUND('',#7520,.T.);
#5223=FACE_OUTER_BOUND('',#7521,.T.);
#5224=FACE_OUTER_BOUND('',#7522,.T.);
#5225=FACE_OUTER_BOUND('',#7524,.T.);
#5226=FACE_OUTER_BOUND('',#7525,.T.);
#5227=FACE_OUTER_BOUND('',#7526,.T.);
#5228=FACE_OUTER_BOUND('',#7527,.T.);
#5229=FACE_OUTER_BOUND('',#7528,.T.);
#5230=FACE_OUTER_BOUND('',#7529,.T.);
#5231=FACE_OUTER_BOUND('',#7530,.T.);
#5232=FACE_OUTER_BOUND('',#7531,.T.);
#5233=FACE_OUTER_BOUND('',#7533,.T.);
#5234=EDGE_LOOP('',(#22278,#22279,#22280,#22281,#22282,#22283));
#5235=EDGE_LOOP('',(#22284,#22285,#22286,#22287,#22288,#22289));
#5236=EDGE_LOOP('',(#22290,#22291,#22292,#22293,#22294));
#5237=EDGE_LOOP('',(#22295,#22296,#22297,#22298,#22299));
#5238=EDGE_LOOP('',(#22300));
#5239=EDGE_LOOP('',(#22301));
#5240=EDGE_LOOP('',(#22302,#22303,#22304,#22305,#22306));
#5241=EDGE_LOOP('',(#22307,#22308,#22309,#22310,#22311));
#5242=EDGE_LOOP('',(#22312));
#5243=EDGE_LOOP('',(#22313));
#5244=EDGE_LOOP('',(#22314,#22315,#22316,#22317,#22318));
#5245=EDGE_LOOP('',(#22319,#22320,#22321,#22322,#22323,#22324));
#5246=EDGE_LOOP('',(#22325));
#5247=EDGE_LOOP('',(#22326));
#5248=EDGE_LOOP('',(#22327,#22328,#22329,#22330,#22331,#22332));
#5249=EDGE_LOOP('',(#22333,#22334,#22335,#22336,#22337));
#5250=EDGE_LOOP('',(#22338,#22339,#22340,#22341,#22342,#22343));
#5251=EDGE_LOOP('',(#22344,#22345,#22346,#22347,#22348,#22349));
#5252=EDGE_LOOP('',(#22350,#22351,#22352,#22353,#22354));
#5253=EDGE_LOOP('',(#22355,#22356,#22357,#22358,#22359,#22360));
#5254=EDGE_LOOP('',(#22361,#22362,#22363,#22364,#22365,#22366));
#5255=EDGE_LOOP('',(#22367,#22368,#22369,#22370,#22371,#22372));
#5256=EDGE_LOOP('',(#22373,#22374,#22375,#22376,#22377,#22378));
#5257=EDGE_LOOP('',(#22379,#22380,#22381,#22382,#22383,#22384));
#5258=EDGE_LOOP('',(#22385,#22386,#22387,#22388,#22389,#22390,#22391,#22392,
#22393,#22394,#22395,#22396,#22397,#22398,#22399,#22400,#22401));
#5259=EDGE_LOOP('',(#22402,#22403,#22404,#22405,#22406,#22407,#22408,#22409));
#5260=EDGE_LOOP('',(#22410,#22411,#22412,#22413,#22414,#22415,#22416,#22417));
#5261=EDGE_LOOP('',(#22418,#22419,#22420,#22421,#22422,#22423,#22424,#22425));
#5262=EDGE_LOOP('',(#22426,#22427,#22428,#22429,#22430,#22431,#22432,#22433));
#5263=EDGE_LOOP('',(#22434,#22435,#22436,#22437,#22438,#22439,#22440,#22441));
#5264=EDGE_LOOP('',(#22442,#22443,#22444,#22445,#22446,#22447,#22448,#22449));
#5265=EDGE_LOOP('',(#22450,#22451,#22452,#22453,#22454,#22455,#22456,#22457));
#5266=EDGE_LOOP('',(#22458,#22459,#22460,#22461,#22462,#22463,#22464,#22465));
#5267=EDGE_LOOP('',(#22466,#22467,#22468,#22469,#22470,#22471,#22472,#22473));
#5268=EDGE_LOOP('',(#22474,#22475,#22476,#22477,#22478,#22479,#22480,#22481));
#5269=EDGE_LOOP('',(#22482,#22483,#22484,#22485,#22486,#22487,#22488,#22489));
#5270=EDGE_LOOP('',(#22490,#22491,#22492,#22493,#22494,#22495,#22496,#22497));
#5271=EDGE_LOOP('',(#22498,#22499,#22500,#22501,#22502,#22503,#22504,#22505));
#5272=EDGE_LOOP('',(#22506,#22507,#22508,#22509,#22510,#22511,#22512,#22513));
#5273=EDGE_LOOP('',(#22514,#22515,#22516,#22517,#22518,#22519,#22520,#22521));
#5274=EDGE_LOOP('',(#22522,#22523,#22524,#22525,#22526,#22527,#22528,#22529));
#5275=EDGE_LOOP('',(#22530,#22531,#22532,#22533,#22534,#22535,#22536,#22537));
#5276=EDGE_LOOP('',(#22538,#22539,#22540,#22541,#22542,#22543,#22544,#22545));
#5277=EDGE_LOOP('',(#22546,#22547,#22548,#22549,#22550,#22551,#22552,#22553));
#5278=EDGE_LOOP('',(#22554,#22555,#22556,#22557,#22558,#22559,#22560,#22561));
#5279=EDGE_LOOP('',(#22562,#22563,#22564,#22565,#22566,#22567,#22568,#22569));
#5280=EDGE_LOOP('',(#22570,#22571,#22572,#22573,#22574,#22575,#22576,#22577));
#5281=EDGE_LOOP('',(#22578,#22579,#22580,#22581,#22582,#22583,#22584,#22585));
#5282=EDGE_LOOP('',(#22586,#22587,#22588,#22589,#22590,#22591,#22592,#22593));
#5283=EDGE_LOOP('',(#22594,#22595,#22596,#22597,#22598,#22599,#22600,#22601));
#5284=EDGE_LOOP('',(#22602,#22603,#22604,#22605,#22606,#22607,#22608,#22609));
#5285=EDGE_LOOP('',(#22610,#22611,#22612,#22613,#22614,#22615,#22616,#22617));
#5286=EDGE_LOOP('',(#22618,#22619,#22620,#22621,#22622,#22623,#22624,#22625));
#5287=EDGE_LOOP('',(#22626,#22627,#22628,#22629,#22630,#22631,#22632,#22633));
#5288=EDGE_LOOP('',(#22634,#22635,#22636,#22637,#22638,#22639,#22640,#22641));
#5289=EDGE_LOOP('',(#22642,#22643,#22644,#22645,#22646,#22647,#22648,#22649));
#5290=EDGE_LOOP('',(#22650,#22651,#22652,#22653,#22654,#22655,#22656,#22657));
#5291=EDGE_LOOP('',(#22658,#22659,#22660,#22661,#22662,#22663,#22664,#22665));
#5292=EDGE_LOOP('',(#22666,#22667,#22668,#22669,#22670,#22671,#22672,#22673));
#5293=EDGE_LOOP('',(#22674,#22675,#22676,#22677,#22678,#22679,#22680,#22681));
#5294=EDGE_LOOP('',(#22682,#22683,#22684,#22685,#22686,#22687,#22688,#22689));
#5295=EDGE_LOOP('',(#22690,#22691,#22692,#22693,#22694,#22695,#22696,#22697));
#5296=EDGE_LOOP('',(#22698,#22699,#22700,#22701,#22702,#22703,#22704,#22705));
#5297=EDGE_LOOP('',(#22706,#22707,#22708,#22709,#22710,#22711,#22712,#22713));
#5298=EDGE_LOOP('',(#22714,#22715,#22716,#22717,#22718,#22719,#22720,#22721));
#5299=EDGE_LOOP('',(#22722,#22723,#22724,#22725,#22726,#22727,#22728,#22729));
#5300=EDGE_LOOP('',(#22730,#22731,#22732,#22733,#22734,#22735,#22736,#22737));
#5301=EDGE_LOOP('',(#22738,#22739,#22740,#22741,#22742,#22743,#22744,#22745));
#5302=EDGE_LOOP('',(#22746,#22747,#22748,#22749,#22750,#22751,#22752,#22753));
#5303=EDGE_LOOP('',(#22754,#22755,#22756,#22757,#22758,#22759,#22760,#22761));
#5304=EDGE_LOOP('',(#22762,#22763,#22764,#22765,#22766,#22767,#22768,#22769));
#5305=EDGE_LOOP('',(#22770,#22771,#22772,#22773,#22774,#22775,#22776,#22777));
#5306=EDGE_LOOP('',(#22778,#22779,#22780,#22781,#22782,#22783,#22784,#22785));
#5307=EDGE_LOOP('',(#22786,#22787,#22788,#22789,#22790,#22791,#22792,#22793));
#5308=EDGE_LOOP('',(#22794,#22795,#22796,#22797,#22798,#22799,#22800,#22801));
#5309=EDGE_LOOP('',(#22802,#22803,#22804,#22805,#22806,#22807,#22808,#22809));
#5310=EDGE_LOOP('',(#22810,#22811,#22812,#22813,#22814,#22815,#22816,#22817));
#5311=EDGE_LOOP('',(#22818,#22819,#22820,#22821,#22822,#22823,#22824,#22825));
#5312=EDGE_LOOP('',(#22826,#22827,#22828,#22829,#22830,#22831,#22832,#22833));
#5313=EDGE_LOOP('',(#22834,#22835,#22836,#22837,#22838,#22839,#22840,#22841));
#5314=EDGE_LOOP('',(#22842,#22843,#22844,#22845,#22846,#22847,#22848,#22849));
#5315=EDGE_LOOP('',(#22850,#22851,#22852,#22853,#22854,#22855,#22856,#22857));
#5316=EDGE_LOOP('',(#22858,#22859,#22860,#22861,#22862,#22863,#22864,#22865));
#5317=EDGE_LOOP('',(#22866,#22867,#22868,#22869,#22870,#22871,#22872,#22873));
#5318=EDGE_LOOP('',(#22874,#22875,#22876,#22877,#22878,#22879,#22880,#22881));
#5319=EDGE_LOOP('',(#22882,#22883,#22884,#22885,#22886,#22887,#22888,#22889));
#5320=EDGE_LOOP('',(#22890,#22891,#22892,#22893,#22894,#22895,#22896,#22897));
#5321=EDGE_LOOP('',(#22898,#22899,#22900,#22901,#22902,#22903,#22904,#22905));
#5322=EDGE_LOOP('',(#22906,#22907,#22908,#22909,#22910,#22911,#22912,#22913));
#5323=EDGE_LOOP('',(#22914,#22915,#22916,#22917,#22918,#22919,#22920,#22921));
#5324=EDGE_LOOP('',(#22922,#22923,#22924,#22925,#22926,#22927,#22928,#22929));
#5325=EDGE_LOOP('',(#22930,#22931,#22932,#22933,#22934,#22935,#22936,#22937));
#5326=EDGE_LOOP('',(#22938,#22939,#22940,#22941,#22942,#22943,#22944,#22945));
#5327=EDGE_LOOP('',(#22946,#22947,#22948,#22949,#22950,#22951,#22952,#22953));
#5328=EDGE_LOOP('',(#22954,#22955,#22956,#22957,#22958,#22959,#22960,#22961));
#5329=EDGE_LOOP('',(#22962,#22963,#22964,#22965,#22966,#22967,#22968,#22969));
#5330=EDGE_LOOP('',(#22970,#22971,#22972,#22973));
#5331=EDGE_LOOP('',(#22974,#22975,#22976,#22977));
#5332=EDGE_LOOP('',(#22978,#22979,#22980,#22981));
#5333=EDGE_LOOP('',(#22982,#22983,#22984,#22985));
#5334=EDGE_LOOP('',(#22986,#22987,#22988,#22989));
#5335=EDGE_LOOP('',(#22990,#22991,#22992,#22993));
#5336=EDGE_LOOP('',(#22994,#22995,#22996,#22997));
#5337=EDGE_LOOP('',(#22998,#22999,#23000,#23001));
#5338=EDGE_LOOP('',(#23002,#23003,#23004,#23005));
#5339=EDGE_LOOP('',(#23006,#23007,#23008,#23009));
#5340=EDGE_LOOP('',(#23010,#23011,#23012,#23013));
#5341=EDGE_LOOP('',(#23014,#23015,#23016,#23017));
#5342=EDGE_LOOP('',(#23018,#23019,#23020,#23021));
#5343=EDGE_LOOP('',(#23022,#23023,#23024,#23025));
#5344=EDGE_LOOP('',(#23026,#23027,#23028,#23029));
#5345=EDGE_LOOP('',(#23030,#23031,#23032,#23033));
#5346=EDGE_LOOP('',(#23034,#23035,#23036,#23037,#23038,#23039,#23040,#23041,
#23042,#23043));
#5347=EDGE_LOOP('',(#23044));
#5348=EDGE_LOOP('',(#23045));
#5349=EDGE_LOOP('',(#23046));
#5350=EDGE_LOOP('',(#23047));
#5351=EDGE_LOOP('',(#23048));
#5352=EDGE_LOOP('',(#23049));
#5353=EDGE_LOOP('',(#23050,#23051,#23052,#23053,#23054));
#5354=EDGE_LOOP('',(#23055,#23056,#23057,#23058));
#5355=EDGE_LOOP('',(#23059,#23060,#23061,#23062,#23063));
#5356=EDGE_LOOP('',(#23064,#23065,#23066,#23067,#23068));
#5357=EDGE_LOOP('',(#23069,#23070,#23071));
#5358=EDGE_LOOP('',(#23072,#23073,#23074));
#5359=EDGE_LOOP('',(#23075,#23076,#23077,#23078));
#5360=EDGE_LOOP('',(#23079,#23080,#23081));
#5361=EDGE_LOOP('',(#23082,#23083,#23084,#23085));
#5362=EDGE_LOOP('',(#23086,#23087,#23088,#23089));
#5363=EDGE_LOOP('',(#23090,#23091,#23092,#23093));
#5364=EDGE_LOOP('',(#23094,#23095,#23096,#23097));
#5365=EDGE_LOOP('',(#23098,#23099,#23100,#23101));
#5366=EDGE_LOOP('',(#23102,#23103,#23104,#23105));
#5367=EDGE_LOOP('',(#23106,#23107,#23108));
#5368=EDGE_LOOP('',(#23109,#23110,#23111));
#5369=EDGE_LOOP('',(#23112,#23113,#23114));
#5370=EDGE_LOOP('',(#23115,#23116,#23117,#23118));
#5371=EDGE_LOOP('',(#23119,#23120,#23121));
#5372=EDGE_LOOP('',(#23122,#23123,#23124,#23125));
#5373=EDGE_LOOP('',(#23126,#23127,#23128,#23129));
#5374=EDGE_LOOP('',(#23130,#23131,#23132,#23133));
#5375=EDGE_LOOP('',(#23134,#23135,#23136,#23137));
#5376=EDGE_LOOP('',(#23138,#23139,#23140,#23141));
#5377=EDGE_LOOP('',(#23142,#23143,#23144,#23145));
#5378=EDGE_LOOP('',(#23146,#23147,#23148,#23149));
#5379=EDGE_LOOP('',(#23150,#23151,#23152,#23153));
#5380=EDGE_LOOP('',(#23154,#23155,#23156,#23157));
#5381=EDGE_LOOP('',(#23158,#23159,#23160,#23161));
#5382=EDGE_LOOP('',(#23162,#23163,#23164));
#5383=EDGE_LOOP('',(#23165,#23166,#23167,#23168,#23169));
#5384=EDGE_LOOP('',(#23170,#23171,#23172,#23173));
#5385=EDGE_LOOP('',(#23174,#23175,#23176));
#5386=EDGE_LOOP('',(#23177,#23178,#23179,#23180,#23181));
#5387=EDGE_LOOP('',(#23182,#23183,#23184,#23185));
#5388=EDGE_LOOP('',(#23186,#23187,#23188,#23189));
#5389=EDGE_LOOP('',(#23190,#23191,#23192,#23193,#23194));
#5390=EDGE_LOOP('',(#23195,#23196,#23197,#23198));
#5391=EDGE_LOOP('',(#23199,#23200,#23201,#23202,#23203,#23204));
#5392=EDGE_LOOP('',(#23205,#23206,#23207,#23208,#23209));
#5393=EDGE_LOOP('',(#23210,#23211,#23212,#23213));
#5394=EDGE_LOOP('',(#23214,#23215,#23216,#23217));
#5395=EDGE_LOOP('',(#23218,#23219,#23220));
#5396=EDGE_LOOP('',(#23221,#23222,#23223));
#5397=EDGE_LOOP('',(#23224,#23225,#23226));
#5398=EDGE_LOOP('',(#23227,#23228,#23229,#23230));
#5399=EDGE_LOOP('',(#23231,#23232,#23233));
#5400=EDGE_LOOP('',(#23234,#23235,#23236,#23237));
#5401=EDGE_LOOP('',(#23238,#23239,#23240,#23241));
#5402=EDGE_LOOP('',(#23242,#23243,#23244,#23245));
#5403=EDGE_LOOP('',(#23246,#23247,#23248,#23249));
#5404=EDGE_LOOP('',(#23250,#23251,#23252,#23253));
#5405=EDGE_LOOP('',(#23254,#23255,#23256,#23257));
#5406=EDGE_LOOP('',(#23258,#23259,#23260,#23261));
#5407=EDGE_LOOP('',(#23262,#23263,#23264,#23265));
#5408=EDGE_LOOP('',(#23266,#23267,#23268,#23269));
#5409=EDGE_LOOP('',(#23270,#23271,#23272,#23273));
#5410=EDGE_LOOP('',(#23274,#23275,#23276));
#5411=EDGE_LOOP('',(#23277,#23278,#23279));
#5412=EDGE_LOOP('',(#23280,#23281,#23282));
#5413=EDGE_LOOP('',(#23283,#23284,#23285,#23286));
#5414=EDGE_LOOP('',(#23287,#23288,#23289));
#5415=EDGE_LOOP('',(#23290,#23291,#23292,#23293));
#5416=EDGE_LOOP('',(#23294,#23295,#23296,#23297));
#5417=EDGE_LOOP('',(#23298,#23299,#23300,#23301));
#5418=EDGE_LOOP('',(#23302,#23303,#23304,#23305));
#5419=EDGE_LOOP('',(#23306,#23307,#23308,#23309));
#5420=EDGE_LOOP('',(#23310,#23311,#23312,#23313));
#5421=EDGE_LOOP('',(#23314,#23315,#23316,#23317));
#5422=EDGE_LOOP('',(#23318,#23319,#23320,#23321));
#5423=EDGE_LOOP('',(#23322,#23323,#23324,#23325));
#5424=EDGE_LOOP('',(#23326,#23327,#23328,#23329));
#5425=EDGE_LOOP('',(#23330,#23331,#23332,#23333,#23334));
#5426=EDGE_LOOP('',(#23335,#23336,#23337,#23338));
#5427=EDGE_LOOP('',(#23339,#23340,#23341,#23342,#23343));
#5428=EDGE_LOOP('',(#23344,#23345,#23346,#23347,#23348));
#5429=EDGE_LOOP('',(#23349,#23350,#23351));
#5430=EDGE_LOOP('',(#23352,#23353,#23354));
#5431=EDGE_LOOP('',(#23355,#23356,#23357,#23358));
#5432=EDGE_LOOP('',(#23359,#23360,#23361));
#5433=EDGE_LOOP('',(#23362,#23363,#23364,#23365));
#5434=EDGE_LOOP('',(#23366,#23367,#23368,#23369));
#5435=EDGE_LOOP('',(#23370,#23371,#23372,#23373));
#5436=EDGE_LOOP('',(#23374,#23375,#23376,#23377));
#5437=EDGE_LOOP('',(#23378,#23379,#23380,#23381));
#5438=EDGE_LOOP('',(#23382,#23383,#23384,#23385));
#5439=EDGE_LOOP('',(#23386,#23387,#23388));
#5440=EDGE_LOOP('',(#23389,#23390,#23391));
#5441=EDGE_LOOP('',(#23392,#23393,#23394));
#5442=EDGE_LOOP('',(#23395,#23396,#23397,#23398));
#5443=EDGE_LOOP('',(#23399,#23400,#23401));
#5444=EDGE_LOOP('',(#23402,#23403,#23404,#23405));
#5445=EDGE_LOOP('',(#23406,#23407,#23408,#23409));
#5446=EDGE_LOOP('',(#23410,#23411,#23412,#23413));
#5447=EDGE_LOOP('',(#23414,#23415,#23416,#23417));
#5448=EDGE_LOOP('',(#23418,#23419,#23420,#23421));
#5449=EDGE_LOOP('',(#23422,#23423,#23424,#23425));
#5450=EDGE_LOOP('',(#23426,#23427,#23428,#23429));
#5451=EDGE_LOOP('',(#23430,#23431,#23432,#23433));
#5452=EDGE_LOOP('',(#23434,#23435,#23436,#23437));
#5453=EDGE_LOOP('',(#23438,#23439,#23440,#23441));
#5454=EDGE_LOOP('',(#23442,#23443,#23444));
#5455=EDGE_LOOP('',(#23445,#23446,#23447,#23448,#23449));
#5456=EDGE_LOOP('',(#23450,#23451,#23452,#23453));
#5457=EDGE_LOOP('',(#23454,#23455,#23456));
#5458=EDGE_LOOP('',(#23457,#23458,#23459,#23460,#23461));
#5459=EDGE_LOOP('',(#23462,#23463,#23464,#23465));
#5460=EDGE_LOOP('',(#23466,#23467,#23468,#23469));
#5461=EDGE_LOOP('',(#23470,#23471,#23472,#23473,#23474));
#5462=EDGE_LOOP('',(#23475,#23476,#23477,#23478));
#5463=EDGE_LOOP('',(#23479,#23480,#23481,#23482,#23483,#23484));
#5464=EDGE_LOOP('',(#23485,#23486,#23487,#23488,#23489));
#5465=EDGE_LOOP('',(#23490,#23491,#23492,#23493));
#5466=EDGE_LOOP('',(#23494,#23495,#23496,#23497));
#5467=EDGE_LOOP('',(#23498,#23499,#23500));
#5468=EDGE_LOOP('',(#23501,#23502,#23503));
#5469=EDGE_LOOP('',(#23504,#23505,#23506));
#5470=EDGE_LOOP('',(#23507,#23508,#23509,#23510));
#5471=EDGE_LOOP('',(#23511,#23512,#23513));
#5472=EDGE_LOOP('',(#23514,#23515,#23516,#23517));
#5473=EDGE_LOOP('',(#23518,#23519,#23520,#23521));
#5474=EDGE_LOOP('',(#23522,#23523,#23524,#23525));
#5475=EDGE_LOOP('',(#23526,#23527,#23528,#23529));
#5476=EDGE_LOOP('',(#23530,#23531,#23532,#23533));
#5477=EDGE_LOOP('',(#23534,#23535,#23536,#23537));
#5478=EDGE_LOOP('',(#23538,#23539,#23540,#23541));
#5479=EDGE_LOOP('',(#23542,#23543,#23544,#23545));
#5480=EDGE_LOOP('',(#23546,#23547,#23548,#23549));
#5481=EDGE_LOOP('',(#23550,#23551,#23552,#23553));
#5482=EDGE_LOOP('',(#23554,#23555,#23556));
#5483=EDGE_LOOP('',(#23557,#23558,#23559));
#5484=EDGE_LOOP('',(#23560,#23561,#23562));
#5485=EDGE_LOOP('',(#23563,#23564,#23565,#23566));
#5486=EDGE_LOOP('',(#23567,#23568,#23569));
#5487=EDGE_LOOP('',(#23570,#23571,#23572,#23573));
#5488=EDGE_LOOP('',(#23574,#23575,#23576,#23577));
#5489=EDGE_LOOP('',(#23578,#23579,#23580,#23581));
#5490=EDGE_LOOP('',(#23582,#23583,#23584,#23585));
#5491=EDGE_LOOP('',(#23586,#23587,#23588,#23589));
#5492=EDGE_LOOP('',(#23590,#23591,#23592,#23593));
#5493=EDGE_LOOP('',(#23594,#23595,#23596,#23597));
#5494=EDGE_LOOP('',(#23598,#23599,#23600,#23601));
#5495=EDGE_LOOP('',(#23602,#23603,#23604,#23605));
#5496=EDGE_LOOP('',(#23606,#23607,#23608,#23609));
#5497=EDGE_LOOP('',(#23610,#23611,#23612,#23613,#23614));
#5498=EDGE_LOOP('',(#23615,#23616,#23617,#23618));
#5499=EDGE_LOOP('',(#23619,#23620,#23621,#23622,#23623));
#5500=EDGE_LOOP('',(#23624,#23625,#23626,#23627,#23628));
#5501=EDGE_LOOP('',(#23629,#23630,#23631));
#5502=EDGE_LOOP('',(#23632,#23633,#23634));
#5503=EDGE_LOOP('',(#23635,#23636,#23637,#23638));
#5504=EDGE_LOOP('',(#23639,#23640,#23641));
#5505=EDGE_LOOP('',(#23642,#23643,#23644,#23645));
#5506=EDGE_LOOP('',(#23646,#23647,#23648,#23649));
#5507=EDGE_LOOP('',(#23650,#23651,#23652,#23653));
#5508=EDGE_LOOP('',(#23654,#23655,#23656,#23657));
#5509=EDGE_LOOP('',(#23658,#23659,#23660,#23661));
#5510=EDGE_LOOP('',(#23662,#23663,#23664,#23665));
#5511=EDGE_LOOP('',(#23666,#23667,#23668));
#5512=EDGE_LOOP('',(#23669,#23670,#23671));
#5513=EDGE_LOOP('',(#23672,#23673,#23674));
#5514=EDGE_LOOP('',(#23675,#23676,#23677,#23678));
#5515=EDGE_LOOP('',(#23679,#23680,#23681));
#5516=EDGE_LOOP('',(#23682,#23683,#23684,#23685));
#5517=EDGE_LOOP('',(#23686,#23687,#23688,#23689));
#5518=EDGE_LOOP('',(#23690,#23691,#23692,#23693));
#5519=EDGE_LOOP('',(#23694,#23695,#23696,#23697));
#5520=EDGE_LOOP('',(#23698,#23699,#23700,#23701));
#5521=EDGE_LOOP('',(#23702,#23703,#23704,#23705));
#5522=EDGE_LOOP('',(#23706,#23707,#23708,#23709));
#5523=EDGE_LOOP('',(#23710,#23711,#23712,#23713));
#5524=EDGE_LOOP('',(#23714,#23715,#23716,#23717));
#5525=EDGE_LOOP('',(#23718,#23719,#23720,#23721));
#5526=EDGE_LOOP('',(#23722,#23723,#23724));
#5527=EDGE_LOOP('',(#23725,#23726,#23727,#23728,#23729));
#5528=EDGE_LOOP('',(#23730,#23731,#23732,#23733));
#5529=EDGE_LOOP('',(#23734,#23735,#23736));
#5530=EDGE_LOOP('',(#23737,#23738,#23739,#23740,#23741));
#5531=EDGE_LOOP('',(#23742,#23743,#23744,#23745));
#5532=EDGE_LOOP('',(#23746,#23747,#23748,#23749));
#5533=EDGE_LOOP('',(#23750,#23751,#23752,#23753,#23754));
#5534=EDGE_LOOP('',(#23755,#23756,#23757,#23758));
#5535=EDGE_LOOP('',(#23759,#23760,#23761,#23762,#23763,#23764));
#5536=EDGE_LOOP('',(#23765,#23766,#23767,#23768,#23769));
#5537=EDGE_LOOP('',(#23770,#23771,#23772,#23773));
#5538=EDGE_LOOP('',(#23774,#23775,#23776,#23777));
#5539=EDGE_LOOP('',(#23778,#23779,#23780));
#5540=EDGE_LOOP('',(#23781,#23782,#23783));
#5541=EDGE_LOOP('',(#23784,#23785,#23786));
#5542=EDGE_LOOP('',(#23787,#23788,#23789,#23790));
#5543=EDGE_LOOP('',(#23791,#23792,#23793));
#5544=EDGE_LOOP('',(#23794,#23795,#23796,#23797));
#5545=EDGE_LOOP('',(#23798,#23799,#23800,#23801));
#5546=EDGE_LOOP('',(#23802,#23803,#23804,#23805));
#5547=EDGE_LOOP('',(#23806,#23807,#23808,#23809));
#5548=EDGE_LOOP('',(#23810,#23811,#23812,#23813));
#5549=EDGE_LOOP('',(#23814,#23815,#23816,#23817));
#5550=EDGE_LOOP('',(#23818,#23819,#23820,#23821));
#5551=EDGE_LOOP('',(#23822,#23823,#23824,#23825));
#5552=EDGE_LOOP('',(#23826,#23827,#23828,#23829));
#5553=EDGE_LOOP('',(#23830,#23831,#23832,#23833));
#5554=EDGE_LOOP('',(#23834,#23835,#23836));
#5555=EDGE_LOOP('',(#23837,#23838,#23839));
#5556=EDGE_LOOP('',(#23840,#23841,#23842));
#5557=EDGE_LOOP('',(#23843,#23844,#23845,#23846));
#5558=EDGE_LOOP('',(#23847,#23848,#23849));
#5559=EDGE_LOOP('',(#23850,#23851,#23852,#23853));
#5560=EDGE_LOOP('',(#23854,#23855,#23856,#23857));
#5561=EDGE_LOOP('',(#23858,#23859,#23860,#23861));
#5562=EDGE_LOOP('',(#23862,#23863,#23864,#23865));
#5563=EDGE_LOOP('',(#23866,#23867,#23868,#23869));
#5564=EDGE_LOOP('',(#23870,#23871,#23872,#23873));
#5565=EDGE_LOOP('',(#23874,#23875,#23876,#23877));
#5566=EDGE_LOOP('',(#23878,#23879,#23880,#23881));
#5567=EDGE_LOOP('',(#23882,#23883,#23884,#23885));
#5568=EDGE_LOOP('',(#23886,#23887,#23888,#23889));
#5569=EDGE_LOOP('',(#23890,#23891,#23892,#23893,#23894));
#5570=EDGE_LOOP('',(#23895,#23896,#23897,#23898));
#5571=EDGE_LOOP('',(#23899,#23900,#23901,#23902,#23903));
#5572=EDGE_LOOP('',(#23904,#23905,#23906,#23907,#23908));
#5573=EDGE_LOOP('',(#23909,#23910,#23911));
#5574=EDGE_LOOP('',(#23912,#23913,#23914));
#5575=EDGE_LOOP('',(#23915,#23916,#23917,#23918));
#5576=EDGE_LOOP('',(#23919,#23920,#23921));
#5577=EDGE_LOOP('',(#23922,#23923,#23924,#23925));
#5578=EDGE_LOOP('',(#23926,#23927,#23928,#23929));
#5579=EDGE_LOOP('',(#23930,#23931,#23932,#23933));
#5580=EDGE_LOOP('',(#23934,#23935,#23936,#23937));
#5581=EDGE_LOOP('',(#23938,#23939,#23940,#23941));
#5582=EDGE_LOOP('',(#23942,#23943,#23944,#23945));
#5583=EDGE_LOOP('',(#23946,#23947,#23948));
#5584=EDGE_LOOP('',(#23949,#23950,#23951));
#5585=EDGE_LOOP('',(#23952,#23953,#23954));
#5586=EDGE_LOOP('',(#23955,#23956,#23957,#23958));
#5587=EDGE_LOOP('',(#23959,#23960,#23961));
#5588=EDGE_LOOP('',(#23962,#23963,#23964,#23965));
#5589=EDGE_LOOP('',(#23966,#23967,#23968,#23969));
#5590=EDGE_LOOP('',(#23970,#23971,#23972,#23973));
#5591=EDGE_LOOP('',(#23974,#23975,#23976,#23977));
#5592=EDGE_LOOP('',(#23978,#23979,#23980,#23981));
#5593=EDGE_LOOP('',(#23982,#23983,#23984,#23985));
#5594=EDGE_LOOP('',(#23986,#23987,#23988,#23989));
#5595=EDGE_LOOP('',(#23990,#23991,#23992,#23993));
#5596=EDGE_LOOP('',(#23994,#23995,#23996,#23997));
#5597=EDGE_LOOP('',(#23998,#23999,#24000,#24001));
#5598=EDGE_LOOP('',(#24002,#24003,#24004));
#5599=EDGE_LOOP('',(#24005,#24006,#24007,#24008,#24009));
#5600=EDGE_LOOP('',(#24010,#24011,#24012,#24013));
#5601=EDGE_LOOP('',(#24014,#24015,#24016));
#5602=EDGE_LOOP('',(#24017,#24018,#24019,#24020,#24021));
#5603=EDGE_LOOP('',(#24022,#24023,#24024,#24025));
#5604=EDGE_LOOP('',(#24026,#24027,#24028,#24029));
#5605=EDGE_LOOP('',(#24030,#24031,#24032,#24033,#24034));
#5606=EDGE_LOOP('',(#24035,#24036,#24037,#24038));
#5607=EDGE_LOOP('',(#24039,#24040,#24041,#24042,#24043,#24044));
#5608=EDGE_LOOP('',(#24045,#24046,#24047,#24048,#24049));
#5609=EDGE_LOOP('',(#24050,#24051,#24052,#24053));
#5610=EDGE_LOOP('',(#24054,#24055,#24056,#24057));
#5611=EDGE_LOOP('',(#24058,#24059,#24060));
#5612=EDGE_LOOP('',(#24061,#24062,#24063));
#5613=EDGE_LOOP('',(#24064,#24065,#24066));
#5614=EDGE_LOOP('',(#24067,#24068,#24069,#24070));
#5615=EDGE_LOOP('',(#24071,#24072,#24073));
#5616=EDGE_LOOP('',(#24074,#24075,#24076,#24077));
#5617=EDGE_LOOP('',(#24078,#24079,#24080,#24081));
#5618=EDGE_LOOP('',(#24082,#24083,#24084,#24085));
#5619=EDGE_LOOP('',(#24086,#24087,#24088,#24089));
#5620=EDGE_LOOP('',(#24090,#24091,#24092,#24093));
#5621=EDGE_LOOP('',(#24094,#24095,#24096,#24097));
#5622=EDGE_LOOP('',(#24098,#24099,#24100,#24101));
#5623=EDGE_LOOP('',(#24102,#24103,#24104,#24105,#24106));
#5624=EDGE_LOOP('',(#24107,#24108,#24109,#24110));
#5625=EDGE_LOOP('',(#24111,#24112,#24113,#24114));
#5626=EDGE_LOOP('',(#24115,#24116,#24117));
#5627=EDGE_LOOP('',(#24118,#24119,#24120));
#5628=EDGE_LOOP('',(#24121,#24122,#24123));
#5629=EDGE_LOOP('',(#24124,#24125,#24126,#24127));
#5630=EDGE_LOOP('',(#24128,#24129,#24130));
#5631=EDGE_LOOP('',(#24131,#24132,#24133,#24134));
#5632=EDGE_LOOP('',(#24135,#24136,#24137,#24138));
#5633=EDGE_LOOP('',(#24139,#24140,#24141,#24142));
#5634=EDGE_LOOP('',(#24143,#24144,#24145,#24146));
#5635=EDGE_LOOP('',(#24147,#24148,#24149,#24150));
#5636=EDGE_LOOP('',(#24151,#24152,#24153,#24154));
#5637=EDGE_LOOP('',(#24155,#24156,#24157,#24158));
#5638=EDGE_LOOP('',(#24159,#24160,#24161,#24162));
#5639=EDGE_LOOP('',(#24163,#24164,#24165,#24166));
#5640=EDGE_LOOP('',(#24167,#24168,#24169,#24170));
#5641=EDGE_LOOP('',(#24171,#24172,#24173,#24174,#24175));
#5642=EDGE_LOOP('',(#24176,#24177,#24178,#24179));
#5643=EDGE_LOOP('',(#24180,#24181,#24182,#24183,#24184));
#5644=EDGE_LOOP('',(#24185,#24186,#24187,#24188,#24189));
#5645=EDGE_LOOP('',(#24190,#24191,#24192));
#5646=EDGE_LOOP('',(#24193,#24194,#24195));
#5647=EDGE_LOOP('',(#24196,#24197,#24198,#24199));
#5648=EDGE_LOOP('',(#24200,#24201,#24202));
#5649=EDGE_LOOP('',(#24203,#24204,#24205,#24206));
#5650=EDGE_LOOP('',(#24207,#24208,#24209,#24210));
#5651=EDGE_LOOP('',(#24211,#24212,#24213,#24214));
#5652=EDGE_LOOP('',(#24215,#24216,#24217,#24218));
#5653=EDGE_LOOP('',(#24219,#24220,#24221,#24222));
#5654=EDGE_LOOP('',(#24223,#24224,#24225,#24226));
#5655=EDGE_LOOP('',(#24227,#24228,#24229));
#5656=EDGE_LOOP('',(#24230,#24231,#24232));
#5657=EDGE_LOOP('',(#24233,#24234,#24235));
#5658=EDGE_LOOP('',(#24236,#24237,#24238,#24239));
#5659=EDGE_LOOP('',(#24240,#24241,#24242));
#5660=EDGE_LOOP('',(#24243,#24244,#24245,#24246));
#5661=EDGE_LOOP('',(#24247,#24248,#24249,#24250));
#5662=EDGE_LOOP('',(#24251,#24252,#24253,#24254));
#5663=EDGE_LOOP('',(#24255,#24256,#24257,#24258));
#5664=EDGE_LOOP('',(#24259,#24260,#24261,#24262));
#5665=EDGE_LOOP('',(#24263,#24264,#24265,#24266));
#5666=EDGE_LOOP('',(#24267,#24268,#24269,#24270));
#5667=EDGE_LOOP('',(#24271,#24272,#24273,#24274));
#5668=EDGE_LOOP('',(#24275,#24276,#24277,#24278));
#5669=EDGE_LOOP('',(#24279,#24280,#24281,#24282));
#5670=EDGE_LOOP('',(#24283,#24284,#24285));
#5671=EDGE_LOOP('',(#24286,#24287,#24288,#24289,#24290));
#5672=EDGE_LOOP('',(#24291,#24292,#24293,#24294));
#5673=EDGE_LOOP('',(#24295,#24296,#24297));
#5674=EDGE_LOOP('',(#24298,#24299,#24300,#24301,#24302));
#5675=EDGE_LOOP('',(#24303,#24304,#24305,#24306));
#5676=EDGE_LOOP('',(#24307,#24308,#24309,#24310));
#5677=EDGE_LOOP('',(#24311,#24312,#24313,#24314,#24315));
#5678=EDGE_LOOP('',(#24316,#24317,#24318,#24319));
#5679=EDGE_LOOP('',(#24320,#24321,#24322,#24323,#24324,#24325));
#5680=EDGE_LOOP('',(#24326,#24327,#24328,#24329,#24330));
#5681=EDGE_LOOP('',(#24331,#24332,#24333,#24334));
#5682=EDGE_LOOP('',(#24335,#24336,#24337,#24338));
#5683=EDGE_LOOP('',(#24339,#24340,#24341));
#5684=EDGE_LOOP('',(#24342,#24343,#24344));
#5685=EDGE_LOOP('',(#24345,#24346,#24347));
#5686=EDGE_LOOP('',(#24348,#24349,#24350,#24351));
#5687=EDGE_LOOP('',(#24352,#24353,#24354));
#5688=EDGE_LOOP('',(#24355,#24356,#24357,#24358));
#5689=EDGE_LOOP('',(#24359,#24360,#24361,#24362));
#5690=EDGE_LOOP('',(#24363,#24364,#24365,#24366));
#5691=EDGE_LOOP('',(#24367,#24368,#24369,#24370));
#5692=EDGE_LOOP('',(#24371,#24372,#24373,#24374));
#5693=EDGE_LOOP('',(#24375,#24376,#24377,#24378));
#5694=EDGE_LOOP('',(#24379,#24380,#24381,#24382));
#5695=EDGE_LOOP('',(#24383,#24384,#24385,#24386));
#5696=EDGE_LOOP('',(#24387,#24388,#24389,#24390));
#5697=EDGE_LOOP('',(#24391,#24392,#24393,#24394));
#5698=EDGE_LOOP('',(#24395,#24396,#24397));
#5699=EDGE_LOOP('',(#24398,#24399,#24400));
#5700=EDGE_LOOP('',(#24401,#24402,#24403));
#5701=EDGE_LOOP('',(#24404,#24405,#24406,#24407));
#5702=EDGE_LOOP('',(#24408,#24409,#24410));
#5703=EDGE_LOOP('',(#24411,#24412,#24413,#24414));
#5704=EDGE_LOOP('',(#24415,#24416,#24417,#24418));
#5705=EDGE_LOOP('',(#24419,#24420,#24421,#24422));
#5706=EDGE_LOOP('',(#24423,#24424,#24425,#24426));
#5707=EDGE_LOOP('',(#24427,#24428,#24429,#24430));
#5708=EDGE_LOOP('',(#24431,#24432,#24433,#24434));
#5709=EDGE_LOOP('',(#24435,#24436,#24437,#24438));
#5710=EDGE_LOOP('',(#24439,#24440,#24441,#24442));
#5711=EDGE_LOOP('',(#24443,#24444,#24445,#24446));
#5712=EDGE_LOOP('',(#24447,#24448,#24449,#24450));
#5713=EDGE_LOOP('',(#24451,#24452,#24453,#24454,#24455));
#5714=EDGE_LOOP('',(#24456,#24457,#24458,#24459));
#5715=EDGE_LOOP('',(#24460,#24461,#24462,#24463,#24464));
#5716=EDGE_LOOP('',(#24465,#24466,#24467,#24468,#24469));
#5717=EDGE_LOOP('',(#24470,#24471,#24472));
#5718=EDGE_LOOP('',(#24473,#24474,#24475));
#5719=EDGE_LOOP('',(#24476,#24477,#24478,#24479));
#5720=EDGE_LOOP('',(#24480,#24481,#24482));
#5721=EDGE_LOOP('',(#24483,#24484,#24485,#24486));
#5722=EDGE_LOOP('',(#24487,#24488,#24489,#24490));
#5723=EDGE_LOOP('',(#24491,#24492,#24493,#24494));
#5724=EDGE_LOOP('',(#24495,#24496,#24497,#24498));
#5725=EDGE_LOOP('',(#24499,#24500,#24501,#24502));
#5726=EDGE_LOOP('',(#24503,#24504,#24505,#24506));
#5727=EDGE_LOOP('',(#24507,#24508,#24509));
#5728=EDGE_LOOP('',(#24510,#24511,#24512));
#5729=EDGE_LOOP('',(#24513,#24514,#24515));
#5730=EDGE_LOOP('',(#24516,#24517,#24518,#24519));
#5731=EDGE_LOOP('',(#24520,#24521,#24522));
#5732=EDGE_LOOP('',(#24523,#24524,#24525,#24526));
#5733=EDGE_LOOP('',(#24527,#24528,#24529,#24530));
#5734=EDGE_LOOP('',(#24531,#24532,#24533,#24534));
#5735=EDGE_LOOP('',(#24535,#24536,#24537,#24538));
#5736=EDGE_LOOP('',(#24539,#24540,#24541,#24542));
#5737=EDGE_LOOP('',(#24543,#24544,#24545,#24546));
#5738=EDGE_LOOP('',(#24547,#24548,#24549,#24550));
#5739=EDGE_LOOP('',(#24551,#24552,#24553,#24554));
#5740=EDGE_LOOP('',(#24555,#24556,#24557,#24558));
#5741=EDGE_LOOP('',(#24559,#24560,#24561,#24562));
#5742=EDGE_LOOP('',(#24563,#24564,#24565));
#5743=EDGE_LOOP('',(#24566,#24567,#24568,#24569,#24570));
#5744=EDGE_LOOP('',(#24571,#24572,#24573,#24574));
#5745=EDGE_LOOP('',(#24575,#24576,#24577));
#5746=EDGE_LOOP('',(#24578,#24579,#24580,#24581,#24582));
#5747=EDGE_LOOP('',(#24583,#24584,#24585,#24586));
#5748=EDGE_LOOP('',(#24587,#24588,#24589,#24590));
#5749=EDGE_LOOP('',(#24591,#24592,#24593,#24594,#24595));
#5750=EDGE_LOOP('',(#24596,#24597,#24598,#24599));
#5751=EDGE_LOOP('',(#24600,#24601,#24602,#24603,#24604,#24605));
#5752=EDGE_LOOP('',(#24606,#24607,#24608,#24609,#24610));
#5753=EDGE_LOOP('',(#24611,#24612,#24613,#24614));
#5754=EDGE_LOOP('',(#24615,#24616,#24617,#24618));
#5755=EDGE_LOOP('',(#24619,#24620,#24621));
#5756=EDGE_LOOP('',(#24622,#24623,#24624));
#5757=EDGE_LOOP('',(#24625,#24626,#24627));
#5758=EDGE_LOOP('',(#24628,#24629,#24630,#24631));
#5759=EDGE_LOOP('',(#24632,#24633,#24634));
#5760=EDGE_LOOP('',(#24635,#24636,#24637,#24638));
#5761=EDGE_LOOP('',(#24639,#24640,#24641,#24642));
#5762=EDGE_LOOP('',(#24643,#24644,#24645,#24646));
#5763=EDGE_LOOP('',(#24647,#24648,#24649,#24650));
#5764=EDGE_LOOP('',(#24651,#24652,#24653,#24654));
#5765=EDGE_LOOP('',(#24655,#24656,#24657,#24658));
#5766=EDGE_LOOP('',(#24659,#24660,#24661,#24662));
#5767=EDGE_LOOP('',(#24663,#24664,#24665,#24666));
#5768=EDGE_LOOP('',(#24667,#24668,#24669,#24670));
#5769=EDGE_LOOP('',(#24671,#24672,#24673,#24674));
#5770=EDGE_LOOP('',(#24675,#24676,#24677));
#5771=EDGE_LOOP('',(#24678,#24679,#24680));
#5772=EDGE_LOOP('',(#24681,#24682,#24683));
#5773=EDGE_LOOP('',(#24684,#24685,#24686,#24687));
#5774=EDGE_LOOP('',(#24688,#24689,#24690));
#5775=EDGE_LOOP('',(#24691,#24692,#24693,#24694));
#5776=EDGE_LOOP('',(#24695,#24696,#24697,#24698));
#5777=EDGE_LOOP('',(#24699,#24700,#24701,#24702));
#5778=EDGE_LOOP('',(#24703,#24704,#24705,#24706));
#5779=EDGE_LOOP('',(#24707,#24708,#24709,#24710));
#5780=EDGE_LOOP('',(#24711,#24712,#24713,#24714));
#5781=EDGE_LOOP('',(#24715,#24716,#24717,#24718));
#5782=EDGE_LOOP('',(#24719,#24720,#24721,#24722));
#5783=EDGE_LOOP('',(#24723,#24724,#24725,#24726));
#5784=EDGE_LOOP('',(#24727,#24728,#24729,#24730));
#5785=EDGE_LOOP('',(#24731,#24732,#24733,#24734,#24735));
#5786=EDGE_LOOP('',(#24736,#24737,#24738,#24739));
#5787=EDGE_LOOP('',(#24740,#24741,#24742,#24743,#24744));
#5788=EDGE_LOOP('',(#24745,#24746,#24747,#24748,#24749));
#5789=EDGE_LOOP('',(#24750,#24751,#24752));
#5790=EDGE_LOOP('',(#24753,#24754,#24755));
#5791=EDGE_LOOP('',(#24756,#24757,#24758,#24759));
#5792=EDGE_LOOP('',(#24760,#24761,#24762));
#5793=EDGE_LOOP('',(#24763,#24764,#24765,#24766));
#5794=EDGE_LOOP('',(#24767,#24768,#24769,#24770));
#5795=EDGE_LOOP('',(#24771,#24772,#24773,#24774));
#5796=EDGE_LOOP('',(#24775,#24776,#24777,#24778));
#5797=EDGE_LOOP('',(#24779,#24780,#24781,#24782));
#5798=EDGE_LOOP('',(#24783,#24784,#24785,#24786));
#5799=EDGE_LOOP('',(#24787,#24788,#24789));
#5800=EDGE_LOOP('',(#24790,#24791,#24792));
#5801=EDGE_LOOP('',(#24793,#24794,#24795));
#5802=EDGE_LOOP('',(#24796,#24797,#24798,#24799));
#5803=EDGE_LOOP('',(#24800,#24801,#24802));
#5804=EDGE_LOOP('',(#24803,#24804,#24805,#24806));
#5805=EDGE_LOOP('',(#24807,#24808,#24809,#24810));
#5806=EDGE_LOOP('',(#24811,#24812,#24813,#24814));
#5807=EDGE_LOOP('',(#24815,#24816,#24817,#24818));
#5808=EDGE_LOOP('',(#24819,#24820,#24821,#24822));
#5809=EDGE_LOOP('',(#24823,#24824,#24825,#24826));
#5810=EDGE_LOOP('',(#24827,#24828,#24829,#24830));
#5811=EDGE_LOOP('',(#24831,#24832,#24833,#24834));
#5812=EDGE_LOOP('',(#24835,#24836,#24837,#24838));
#5813=EDGE_LOOP('',(#24839,#24840,#24841,#24842));
#5814=EDGE_LOOP('',(#24843,#24844,#24845));
#5815=EDGE_LOOP('',(#24846,#24847,#24848,#24849,#24850));
#5816=EDGE_LOOP('',(#24851,#24852,#24853,#24854));
#5817=EDGE_LOOP('',(#24855,#24856,#24857));
#5818=EDGE_LOOP('',(#24858,#24859,#24860,#24861,#24862));
#5819=EDGE_LOOP('',(#24863,#24864,#24865,#24866));
#5820=EDGE_LOOP('',(#24867,#24868,#24869,#24870));
#5821=EDGE_LOOP('',(#24871,#24872,#24873,#24874,#24875));
#5822=EDGE_LOOP('',(#24876,#24877,#24878,#24879));
#5823=EDGE_LOOP('',(#24880,#24881,#24882,#24883,#24884,#24885));
#5824=EDGE_LOOP('',(#24886,#24887,#24888,#24889,#24890));
#5825=EDGE_LOOP('',(#24891,#24892,#24893,#24894));
#5826=EDGE_LOOP('',(#24895,#24896,#24897,#24898));
#5827=EDGE_LOOP('',(#24899,#24900,#24901));
#5828=EDGE_LOOP('',(#24902,#24903,#24904));
#5829=EDGE_LOOP('',(#24905,#24906,#24907));
#5830=EDGE_LOOP('',(#24908,#24909,#24910,#24911));
#5831=EDGE_LOOP('',(#24912,#24913,#24914));
#5832=EDGE_LOOP('',(#24915,#24916,#24917,#24918));
#5833=EDGE_LOOP('',(#24919,#24920,#24921,#24922));
#5834=EDGE_LOOP('',(#24923,#24924,#24925,#24926));
#5835=EDGE_LOOP('',(#24927,#24928,#24929,#24930));
#5836=EDGE_LOOP('',(#24931,#24932,#24933,#24934));
#5837=EDGE_LOOP('',(#24935,#24936,#24937,#24938));
#5838=EDGE_LOOP('',(#24939,#24940,#24941,#24942));
#5839=EDGE_LOOP('',(#24943,#24944,#24945,#24946));
#5840=EDGE_LOOP('',(#24947,#24948,#24949,#24950));
#5841=EDGE_LOOP('',(#24951,#24952,#24953,#24954));
#5842=EDGE_LOOP('',(#24955,#24956,#24957));
#5843=EDGE_LOOP('',(#24958,#24959,#24960));
#5844=EDGE_LOOP('',(#24961,#24962,#24963));
#5845=EDGE_LOOP('',(#24964,#24965,#24966,#24967));
#5846=EDGE_LOOP('',(#24968,#24969,#24970));
#5847=EDGE_LOOP('',(#24971,#24972,#24973,#24974));
#5848=EDGE_LOOP('',(#24975,#24976,#24977,#24978));
#5849=EDGE_LOOP('',(#24979,#24980,#24981,#24982));
#5850=EDGE_LOOP('',(#24983,#24984,#24985,#24986));
#5851=EDGE_LOOP('',(#24987,#24988,#24989,#24990));
#5852=EDGE_LOOP('',(#24991,#24992,#24993,#24994));
#5853=EDGE_LOOP('',(#24995,#24996,#24997,#24998));
#5854=EDGE_LOOP('',(#24999,#25000,#25001,#25002));
#5855=EDGE_LOOP('',(#25003,#25004,#25005,#25006));
#5856=EDGE_LOOP('',(#25007,#25008,#25009,#25010));
#5857=EDGE_LOOP('',(#25011,#25012,#25013,#25014,#25015));
#5858=EDGE_LOOP('',(#25016,#25017,#25018,#25019));
#5859=EDGE_LOOP('',(#25020,#25021,#25022,#25023,#25024));
#5860=EDGE_LOOP('',(#25025,#25026,#25027,#25028,#25029));
#5861=EDGE_LOOP('',(#25030,#25031,#25032));
#5862=EDGE_LOOP('',(#25033,#25034,#25035));
#5863=EDGE_LOOP('',(#25036,#25037,#25038,#25039));
#5864=EDGE_LOOP('',(#25040,#25041,#25042));
#5865=EDGE_LOOP('',(#25043,#25044,#25045,#25046));
#5866=EDGE_LOOP('',(#25047,#25048,#25049,#25050));
#5867=EDGE_LOOP('',(#25051,#25052,#25053,#25054));
#5868=EDGE_LOOP('',(#25055,#25056,#25057,#25058));
#5869=EDGE_LOOP('',(#25059,#25060,#25061,#25062));
#5870=EDGE_LOOP('',(#25063,#25064,#25065,#25066));
#5871=EDGE_LOOP('',(#25067,#25068,#25069));
#5872=EDGE_LOOP('',(#25070,#25071,#25072));
#5873=EDGE_LOOP('',(#25073,#25074,#25075));
#5874=EDGE_LOOP('',(#25076,#25077,#25078,#25079));
#5875=EDGE_LOOP('',(#25080,#25081,#25082));
#5876=EDGE_LOOP('',(#25083,#25084,#25085,#25086));
#5877=EDGE_LOOP('',(#25087,#25088,#25089,#25090));
#5878=EDGE_LOOP('',(#25091,#25092,#25093,#25094));
#5879=EDGE_LOOP('',(#25095,#25096,#25097,#25098));
#5880=EDGE_LOOP('',(#25099,#25100,#25101,#25102));
#5881=EDGE_LOOP('',(#25103,#25104,#25105,#25106));
#5882=EDGE_LOOP('',(#25107,#25108,#25109,#25110));
#5883=EDGE_LOOP('',(#25111,#25112,#25113,#25114));
#5884=EDGE_LOOP('',(#25115,#25116,#25117,#25118));
#5885=EDGE_LOOP('',(#25119,#25120,#25121,#25122));
#5886=EDGE_LOOP('',(#25123,#25124,#25125));
#5887=EDGE_LOOP('',(#25126,#25127,#25128,#25129,#25130));
#5888=EDGE_LOOP('',(#25131,#25132,#25133,#25134));
#5889=EDGE_LOOP('',(#25135,#25136,#25137));
#5890=EDGE_LOOP('',(#25138,#25139,#25140,#25141,#25142));
#5891=EDGE_LOOP('',(#25143,#25144,#25145,#25146));
#5892=EDGE_LOOP('',(#25147,#25148,#25149,#25150));
#5893=EDGE_LOOP('',(#25151,#25152,#25153,#25154,#25155));
#5894=EDGE_LOOP('',(#25156,#25157,#25158,#25159));
#5895=EDGE_LOOP('',(#25160,#25161,#25162,#25163,#25164,#25165));
#5896=EDGE_LOOP('',(#25166,#25167,#25168,#25169,#25170));
#5897=EDGE_LOOP('',(#25171,#25172,#25173,#25174));
#5898=EDGE_LOOP('',(#25175,#25176,#25177,#25178));
#5899=EDGE_LOOP('',(#25179,#25180,#25181));
#5900=EDGE_LOOP('',(#25182,#25183,#25184));
#5901=EDGE_LOOP('',(#25185,#25186,#25187));
#5902=EDGE_LOOP('',(#25188,#25189,#25190,#25191));
#5903=EDGE_LOOP('',(#25192,#25193,#25194));
#5904=EDGE_LOOP('',(#25195,#25196,#25197,#25198));
#5905=EDGE_LOOP('',(#25199,#25200,#25201,#25202));
#5906=EDGE_LOOP('',(#25203,#25204,#25205,#25206));
#5907=EDGE_LOOP('',(#25207,#25208,#25209,#25210));
#5908=EDGE_LOOP('',(#25211,#25212,#25213,#25214));
#5909=EDGE_LOOP('',(#25215,#25216,#25217,#25218));
#5910=EDGE_LOOP('',(#25219,#25220,#25221,#25222));
#5911=EDGE_LOOP('',(#25223,#25224,#25225,#25226));
#5912=EDGE_LOOP('',(#25227,#25228,#25229,#25230));
#5913=EDGE_LOOP('',(#25231,#25232,#25233,#25234));
#5914=EDGE_LOOP('',(#25235,#25236,#25237));
#5915=EDGE_LOOP('',(#25238,#25239,#25240));
#5916=EDGE_LOOP('',(#25241,#25242,#25243));
#5917=EDGE_LOOP('',(#25244,#25245,#25246,#25247));
#5918=EDGE_LOOP('',(#25248,#25249,#25250));
#5919=EDGE_LOOP('',(#25251,#25252,#25253,#25254));
#5920=EDGE_LOOP('',(#25255,#25256,#25257,#25258));
#5921=EDGE_LOOP('',(#25259,#25260,#25261,#25262));
#5922=EDGE_LOOP('',(#25263,#25264,#25265,#25266));
#5923=EDGE_LOOP('',(#25267,#25268,#25269,#25270));
#5924=EDGE_LOOP('',(#25271,#25272,#25273,#25274));
#5925=EDGE_LOOP('',(#25275,#25276,#25277,#25278));
#5926=EDGE_LOOP('',(#25279,#25280,#25281,#25282));
#5927=EDGE_LOOP('',(#25283,#25284,#25285,#25286));
#5928=EDGE_LOOP('',(#25287,#25288,#25289,#25290));
#5929=EDGE_LOOP('',(#25291,#25292,#25293,#25294,#25295));
#5930=EDGE_LOOP('',(#25296,#25297,#25298,#25299));
#5931=EDGE_LOOP('',(#25300,#25301,#25302,#25303,#25304));
#5932=EDGE_LOOP('',(#25305,#25306,#25307,#25308,#25309));
#5933=EDGE_LOOP('',(#25310,#25311,#25312));
#5934=EDGE_LOOP('',(#25313,#25314,#25315));
#5935=EDGE_LOOP('',(#25316,#25317,#25318,#25319));
#5936=EDGE_LOOP('',(#25320,#25321,#25322));
#5937=EDGE_LOOP('',(#25323,#25324,#25325,#25326));
#5938=EDGE_LOOP('',(#25327,#25328,#25329,#25330));
#5939=EDGE_LOOP('',(#25331,#25332,#25333,#25334));
#5940=EDGE_LOOP('',(#25335,#25336,#25337,#25338));
#5941=EDGE_LOOP('',(#25339,#25340,#25341,#25342));
#5942=EDGE_LOOP('',(#25343,#25344,#25345,#25346));
#5943=EDGE_LOOP('',(#25347,#25348,#25349));
#5944=EDGE_LOOP('',(#25350,#25351,#25352));
#5945=EDGE_LOOP('',(#25353,#25354,#25355));
#5946=EDGE_LOOP('',(#25356,#25357,#25358,#25359));
#5947=EDGE_LOOP('',(#25360,#25361,#25362));
#5948=EDGE_LOOP('',(#25363,#25364,#25365,#25366));
#5949=EDGE_LOOP('',(#25367,#25368,#25369,#25370));
#5950=EDGE_LOOP('',(#25371,#25372,#25373,#25374));
#5951=EDGE_LOOP('',(#25375,#25376,#25377,#25378));
#5952=EDGE_LOOP('',(#25379,#25380,#25381,#25382));
#5953=EDGE_LOOP('',(#25383,#25384,#25385,#25386));
#5954=EDGE_LOOP('',(#25387,#25388,#25389,#25390));
#5955=EDGE_LOOP('',(#25391,#25392,#25393,#25394));
#5956=EDGE_LOOP('',(#25395,#25396,#25397,#25398));
#5957=EDGE_LOOP('',(#25399,#25400,#25401,#25402));
#5958=EDGE_LOOP('',(#25403,#25404,#25405));
#5959=EDGE_LOOP('',(#25406,#25407,#25408,#25409,#25410));
#5960=EDGE_LOOP('',(#25411,#25412,#25413,#25414));
#5961=EDGE_LOOP('',(#25415,#25416,#25417));
#5962=EDGE_LOOP('',(#25418,#25419,#25420,#25421,#25422));
#5963=EDGE_LOOP('',(#25423,#25424,#25425,#25426));
#5964=EDGE_LOOP('',(#25427,#25428,#25429,#25430));
#5965=EDGE_LOOP('',(#25431,#25432,#25433,#25434,#25435));
#5966=EDGE_LOOP('',(#25436,#25437,#25438,#25439));
#5967=EDGE_LOOP('',(#25440,#25441,#25442,#25443,#25444,#25445));
#5968=EDGE_LOOP('',(#25446,#25447,#25448,#25449,#25450));
#5969=EDGE_LOOP('',(#25451,#25452,#25453,#25454));
#5970=EDGE_LOOP('',(#25455,#25456,#25457,#25458));
#5971=EDGE_LOOP('',(#25459,#25460,#25461));
#5972=EDGE_LOOP('',(#25462,#25463,#25464));
#5973=EDGE_LOOP('',(#25465,#25466,#25467));
#5974=EDGE_LOOP('',(#25468,#25469,#25470,#25471));
#5975=EDGE_LOOP('',(#25472,#25473,#25474));
#5976=EDGE_LOOP('',(#25475,#25476,#25477,#25478));
#5977=EDGE_LOOP('',(#25479,#25480,#25481,#25482));
#5978=EDGE_LOOP('',(#25483,#25484,#25485,#25486));
#5979=EDGE_LOOP('',(#25487,#25488,#25489,#25490));
#5980=EDGE_LOOP('',(#25491,#25492,#25493,#25494));
#5981=EDGE_LOOP('',(#25495,#25496,#25497,#25498));
#5982=EDGE_LOOP('',(#25499,#25500,#25501,#25502));
#5983=EDGE_LOOP('',(#25503,#25504,#25505,#25506));
#5984=EDGE_LOOP('',(#25507,#25508,#25509,#25510));
#5985=EDGE_LOOP('',(#25511,#25512,#25513,#25514));
#5986=EDGE_LOOP('',(#25515,#25516,#25517));
#5987=EDGE_LOOP('',(#25518,#25519,#25520));
#5988=EDGE_LOOP('',(#25521,#25522,#25523));
#5989=EDGE_LOOP('',(#25524,#25525,#25526,#25527));
#5990=EDGE_LOOP('',(#25528,#25529,#25530));
#5991=EDGE_LOOP('',(#25531,#25532,#25533,#25534));
#5992=EDGE_LOOP('',(#25535,#25536,#25537,#25538));
#5993=EDGE_LOOP('',(#25539,#25540,#25541,#25542));
#5994=EDGE_LOOP('',(#25543,#25544,#25545,#25546));
#5995=EDGE_LOOP('',(#25547,#25548,#25549,#25550));
#5996=EDGE_LOOP('',(#25551,#25552,#25553,#25554));
#5997=EDGE_LOOP('',(#25555,#25556,#25557,#25558));
#5998=EDGE_LOOP('',(#25559,#25560,#25561,#25562));
#5999=EDGE_LOOP('',(#25563,#25564,#25565,#25566));
#6000=EDGE_LOOP('',(#25567,#25568,#25569,#25570));
#6001=EDGE_LOOP('',(#25571,#25572,#25573,#25574,#25575));
#6002=EDGE_LOOP('',(#25576,#25577,#25578,#25579));
#6003=EDGE_LOOP('',(#25580,#25581,#25582,#25583,#25584));
#6004=EDGE_LOOP('',(#25585,#25586,#25587,#25588,#25589));
#6005=EDGE_LOOP('',(#25590,#25591,#25592));
#6006=EDGE_LOOP('',(#25593,#25594,#25595));
#6007=EDGE_LOOP('',(#25596,#25597,#25598,#25599));
#6008=EDGE_LOOP('',(#25600,#25601,#25602));
#6009=EDGE_LOOP('',(#25603,#25604,#25605,#25606));
#6010=EDGE_LOOP('',(#25607,#25608,#25609,#25610));
#6011=EDGE_LOOP('',(#25611,#25612,#25613,#25614));
#6012=EDGE_LOOP('',(#25615,#25616,#25617,#25618));
#6013=EDGE_LOOP('',(#25619,#25620,#25621,#25622));
#6014=EDGE_LOOP('',(#25623,#25624,#25625,#25626));
#6015=EDGE_LOOP('',(#25627,#25628,#25629));
#6016=EDGE_LOOP('',(#25630,#25631,#25632));
#6017=EDGE_LOOP('',(#25633,#25634,#25635));
#6018=EDGE_LOOP('',(#25636,#25637,#25638,#25639));
#6019=EDGE_LOOP('',(#25640,#25641,#25642));
#6020=EDGE_LOOP('',(#25643,#25644,#25645,#25646));
#6021=EDGE_LOOP('',(#25647,#25648,#25649,#25650));
#6022=EDGE_LOOP('',(#25651,#25652,#25653,#25654));
#6023=EDGE_LOOP('',(#25655,#25656,#25657,#25658));
#6024=EDGE_LOOP('',(#25659,#25660,#25661,#25662));
#6025=EDGE_LOOP('',(#25663,#25664,#25665,#25666));
#6026=EDGE_LOOP('',(#25667,#25668,#25669,#25670));
#6027=EDGE_LOOP('',(#25671,#25672,#25673,#25674));
#6028=EDGE_LOOP('',(#25675,#25676,#25677,#25678));
#6029=EDGE_LOOP('',(#25679,#25680,#25681,#25682));
#6030=EDGE_LOOP('',(#25683,#25684,#25685));
#6031=EDGE_LOOP('',(#25686,#25687,#25688,#25689,#25690));
#6032=EDGE_LOOP('',(#25691,#25692,#25693,#25694));
#6033=EDGE_LOOP('',(#25695,#25696,#25697));
#6034=EDGE_LOOP('',(#25698,#25699,#25700,#25701,#25702));
#6035=EDGE_LOOP('',(#25703,#25704,#25705,#25706));
#6036=EDGE_LOOP('',(#25707,#25708,#25709,#25710));
#6037=EDGE_LOOP('',(#25711,#25712,#25713,#25714,#25715));
#6038=EDGE_LOOP('',(#25716,#25717,#25718,#25719));
#6039=EDGE_LOOP('',(#25720,#25721,#25722,#25723,#25724,#25725));
#6040=EDGE_LOOP('',(#25726,#25727,#25728,#25729,#25730));
#6041=EDGE_LOOP('',(#25731,#25732,#25733,#25734));
#6042=EDGE_LOOP('',(#25735,#25736,#25737,#25738));
#6043=EDGE_LOOP('',(#25739,#25740,#25741));
#6044=EDGE_LOOP('',(#25742,#25743,#25744));
#6045=EDGE_LOOP('',(#25745,#25746,#25747));
#6046=EDGE_LOOP('',(#25748,#25749,#25750,#25751));
#6047=EDGE_LOOP('',(#25752,#25753,#25754));
#6048=EDGE_LOOP('',(#25755,#25756,#25757,#25758));
#6049=EDGE_LOOP('',(#25759,#25760,#25761,#25762));
#6050=EDGE_LOOP('',(#25763,#25764,#25765,#25766));
#6051=EDGE_LOOP('',(#25767,#25768,#25769,#25770));
#6052=EDGE_LOOP('',(#25771,#25772,#25773,#25774));
#6053=EDGE_LOOP('',(#25775,#25776,#25777,#25778));
#6054=EDGE_LOOP('',(#25779,#25780,#25781,#25782));
#6055=EDGE_LOOP('',(#25783,#25784,#25785,#25786));
#6056=EDGE_LOOP('',(#25787,#25788,#25789,#25790));
#6057=EDGE_LOOP('',(#25791,#25792,#25793,#25794));
#6058=EDGE_LOOP('',(#25795,#25796,#25797));
#6059=EDGE_LOOP('',(#25798,#25799,#25800));
#6060=EDGE_LOOP('',(#25801,#25802,#25803));
#6061=EDGE_LOOP('',(#25804,#25805,#25806,#25807));
#6062=EDGE_LOOP('',(#25808,#25809,#25810));
#6063=EDGE_LOOP('',(#25811,#25812,#25813,#25814));
#6064=EDGE_LOOP('',(#25815,#25816,#25817,#25818));
#6065=EDGE_LOOP('',(#25819,#25820,#25821,#25822));
#6066=EDGE_LOOP('',(#25823,#25824,#25825,#25826));
#6067=EDGE_LOOP('',(#25827,#25828,#25829,#25830));
#6068=EDGE_LOOP('',(#25831,#25832,#25833,#25834));
#6069=EDGE_LOOP('',(#25835,#25836,#25837,#25838));
#6070=EDGE_LOOP('',(#25839,#25840,#25841,#25842));
#6071=EDGE_LOOP('',(#25843,#25844,#25845,#25846));
#6072=EDGE_LOOP('',(#25847,#25848,#25849,#25850));
#6073=EDGE_LOOP('',(#25851,#25852,#25853,#25854,#25855));
#6074=EDGE_LOOP('',(#25856,#25857,#25858,#25859));
#6075=EDGE_LOOP('',(#25860,#25861,#25862,#25863,#25864));
#6076=EDGE_LOOP('',(#25865,#25866,#25867,#25868,#25869));
#6077=EDGE_LOOP('',(#25870,#25871,#25872));
#6078=EDGE_LOOP('',(#25873,#25874,#25875));
#6079=EDGE_LOOP('',(#25876,#25877,#25878,#25879));
#6080=EDGE_LOOP('',(#25880,#25881,#25882));
#6081=EDGE_LOOP('',(#25883,#25884,#25885,#25886));
#6082=EDGE_LOOP('',(#25887,#25888,#25889,#25890));
#6083=EDGE_LOOP('',(#25891,#25892,#25893,#25894));
#6084=EDGE_LOOP('',(#25895,#25896,#25897,#25898));
#6085=EDGE_LOOP('',(#25899,#25900,#25901,#25902));
#6086=EDGE_LOOP('',(#25903,#25904,#25905,#25906));
#6087=EDGE_LOOP('',(#25907,#25908,#25909));
#6088=EDGE_LOOP('',(#25910,#25911,#25912));
#6089=EDGE_LOOP('',(#25913,#25914,#25915));
#6090=EDGE_LOOP('',(#25916,#25917,#25918,#25919));
#6091=EDGE_LOOP('',(#25920,#25921,#25922));
#6092=EDGE_LOOP('',(#25923,#25924,#25925,#25926));
#6093=EDGE_LOOP('',(#25927,#25928,#25929,#25930));
#6094=EDGE_LOOP('',(#25931,#25932,#25933,#25934));
#6095=EDGE_LOOP('',(#25935,#25936,#25937,#25938));
#6096=EDGE_LOOP('',(#25939,#25940,#25941,#25942));
#6097=EDGE_LOOP('',(#25943,#25944,#25945,#25946));
#6098=EDGE_LOOP('',(#25947,#25948,#25949,#25950));
#6099=EDGE_LOOP('',(#25951,#25952,#25953,#25954));
#6100=EDGE_LOOP('',(#25955,#25956,#25957,#25958));
#6101=EDGE_LOOP('',(#25959,#25960,#25961,#25962));
#6102=EDGE_LOOP('',(#25963,#25964,#25965));
#6103=EDGE_LOOP('',(#25966,#25967,#25968,#25969,#25970));
#6104=EDGE_LOOP('',(#25971,#25972,#25973,#25974));
#6105=EDGE_LOOP('',(#25975,#25976,#25977));
#6106=EDGE_LOOP('',(#25978,#25979,#25980,#25981,#25982));
#6107=EDGE_LOOP('',(#25983,#25984,#25985,#25986));
#6108=EDGE_LOOP('',(#25987,#25988,#25989,#25990));
#6109=EDGE_LOOP('',(#25991,#25992,#25993,#25994,#25995));
#6110=EDGE_LOOP('',(#25996,#25997,#25998,#25999));
#6111=EDGE_LOOP('',(#26000,#26001,#26002,#26003,#26004,#26005));
#6112=EDGE_LOOP('',(#26006,#26007,#26008,#26009,#26010));
#6113=EDGE_LOOP('',(#26011,#26012,#26013,#26014));
#6114=EDGE_LOOP('',(#26015,#26016,#26017,#26018));
#6115=EDGE_LOOP('',(#26019,#26020,#26021));
#6116=EDGE_LOOP('',(#26022,#26023,#26024));
#6117=EDGE_LOOP('',(#26025,#26026,#26027));
#6118=EDGE_LOOP('',(#26028,#26029,#26030,#26031));
#6119=EDGE_LOOP('',(#26032,#26033,#26034));
#6120=EDGE_LOOP('',(#26035,#26036,#26037,#26038));
#6121=EDGE_LOOP('',(#26039,#26040,#26041,#26042));
#6122=EDGE_LOOP('',(#26043,#26044,#26045,#26046));
#6123=EDGE_LOOP('',(#26047,#26048,#26049,#26050));
#6124=EDGE_LOOP('',(#26051,#26052,#26053,#26054));
#6125=EDGE_LOOP('',(#26055,#26056,#26057,#26058));
#6126=EDGE_LOOP('',(#26059,#26060,#26061,#26062));
#6127=EDGE_LOOP('',(#26063,#26064,#26065,#26066));
#6128=EDGE_LOOP('',(#26067,#26068,#26069,#26070));
#6129=EDGE_LOOP('',(#26071,#26072,#26073,#26074));
#6130=EDGE_LOOP('',(#26075,#26076,#26077));
#6131=EDGE_LOOP('',(#26078,#26079,#26080));
#6132=EDGE_LOOP('',(#26081,#26082,#26083));
#6133=EDGE_LOOP('',(#26084,#26085,#26086,#26087));
#6134=EDGE_LOOP('',(#26088,#26089,#26090));
#6135=EDGE_LOOP('',(#26091,#26092,#26093,#26094));
#6136=EDGE_LOOP('',(#26095,#26096,#26097,#26098));
#6137=EDGE_LOOP('',(#26099,#26100,#26101,#26102));
#6138=EDGE_LOOP('',(#26103,#26104,#26105,#26106));
#6139=EDGE_LOOP('',(#26107,#26108,#26109,#26110));
#6140=EDGE_LOOP('',(#26111,#26112,#26113,#26114));
#6141=EDGE_LOOP('',(#26115,#26116,#26117,#26118));
#6142=EDGE_LOOP('',(#26119,#26120,#26121,#26122));
#6143=EDGE_LOOP('',(#26123,#26124,#26125,#26126));
#6144=EDGE_LOOP('',(#26127,#26128,#26129,#26130));
#6145=EDGE_LOOP('',(#26131,#26132,#26133,#26134,#26135));
#6146=EDGE_LOOP('',(#26136,#26137,#26138,#26139));
#6147=EDGE_LOOP('',(#26140,#26141,#26142,#26143,#26144));
#6148=EDGE_LOOP('',(#26145,#26146,#26147,#26148,#26149));
#6149=EDGE_LOOP('',(#26150,#26151,#26152));
#6150=EDGE_LOOP('',(#26153,#26154,#26155));
#6151=EDGE_LOOP('',(#26156,#26157,#26158,#26159));
#6152=EDGE_LOOP('',(#26160,#26161,#26162));
#6153=EDGE_LOOP('',(#26163,#26164,#26165,#26166));
#6154=EDGE_LOOP('',(#26167,#26168,#26169,#26170));
#6155=EDGE_LOOP('',(#26171,#26172,#26173,#26174));
#6156=EDGE_LOOP('',(#26175,#26176,#26177,#26178));
#6157=EDGE_LOOP('',(#26179,#26180,#26181,#26182));
#6158=EDGE_LOOP('',(#26183,#26184,#26185,#26186));
#6159=EDGE_LOOP('',(#26187,#26188,#26189));
#6160=EDGE_LOOP('',(#26190,#26191,#26192));
#6161=EDGE_LOOP('',(#26193,#26194,#26195));
#6162=EDGE_LOOP('',(#26196,#26197,#26198,#26199));
#6163=EDGE_LOOP('',(#26200,#26201,#26202));
#6164=EDGE_LOOP('',(#26203,#26204,#26205,#26206));
#6165=EDGE_LOOP('',(#26207,#26208,#26209,#26210));
#6166=EDGE_LOOP('',(#26211,#26212,#26213,#26214));
#6167=EDGE_LOOP('',(#26215,#26216,#26217,#26218));
#6168=EDGE_LOOP('',(#26219,#26220,#26221,#26222));
#6169=EDGE_LOOP('',(#26223,#26224,#26225,#26226));
#6170=EDGE_LOOP('',(#26227,#26228,#26229,#26230));
#6171=EDGE_LOOP('',(#26231,#26232,#26233,#26234));
#6172=EDGE_LOOP('',(#26235,#26236,#26237,#26238));
#6173=EDGE_LOOP('',(#26239,#26240,#26241,#26242));
#6174=EDGE_LOOP('',(#26243,#26244,#26245));
#6175=EDGE_LOOP('',(#26246,#26247,#26248,#26249,#26250));
#6176=EDGE_LOOP('',(#26251,#26252,#26253,#26254));
#6177=EDGE_LOOP('',(#26255,#26256,#26257));
#6178=EDGE_LOOP('',(#26258,#26259,#26260,#26261,#26262));
#6179=EDGE_LOOP('',(#26263,#26264,#26265,#26266));
#6180=EDGE_LOOP('',(#26267,#26268,#26269,#26270));
#6181=EDGE_LOOP('',(#26271,#26272,#26273,#26274,#26275));
#6182=EDGE_LOOP('',(#26276,#26277,#26278,#26279));
#6183=EDGE_LOOP('',(#26280,#26281,#26282,#26283,#26284,#26285));
#6184=EDGE_LOOP('',(#26286,#26287,#26288,#26289,#26290));
#6185=EDGE_LOOP('',(#26291,#26292,#26293,#26294));
#6186=EDGE_LOOP('',(#26295,#26296,#26297,#26298));
#6187=EDGE_LOOP('',(#26299,#26300,#26301));
#6188=EDGE_LOOP('',(#26302,#26303,#26304));
#6189=EDGE_LOOP('',(#26305,#26306,#26307));
#6190=EDGE_LOOP('',(#26308,#26309,#26310,#26311));
#6191=EDGE_LOOP('',(#26312,#26313,#26314));
#6192=EDGE_LOOP('',(#26315,#26316,#26317,#26318));
#6193=EDGE_LOOP('',(#26319,#26320,#26321,#26322));
#6194=EDGE_LOOP('',(#26323,#26324,#26325,#26326));
#6195=EDGE_LOOP('',(#26327,#26328,#26329,#26330));
#6196=EDGE_LOOP('',(#26331,#26332,#26333,#26334));
#6197=EDGE_LOOP('',(#26335,#26336,#26337,#26338));
#6198=EDGE_LOOP('',(#26339,#26340,#26341,#26342));
#6199=EDGE_LOOP('',(#26343,#26344,#26345,#26346));
#6200=EDGE_LOOP('',(#26347,#26348,#26349,#26350));
#6201=EDGE_LOOP('',(#26351,#26352,#26353,#26354));
#6202=EDGE_LOOP('',(#26355,#26356,#26357));
#6203=EDGE_LOOP('',(#26358,#26359,#26360));
#6204=EDGE_LOOP('',(#26361,#26362,#26363));
#6205=EDGE_LOOP('',(#26364,#26365,#26366,#26367));
#6206=EDGE_LOOP('',(#26368,#26369,#26370));
#6207=EDGE_LOOP('',(#26371,#26372,#26373,#26374));
#6208=EDGE_LOOP('',(#26375,#26376,#26377,#26378));
#6209=EDGE_LOOP('',(#26379,#26380,#26381,#26382));
#6210=EDGE_LOOP('',(#26383,#26384,#26385,#26386));
#6211=EDGE_LOOP('',(#26387,#26388,#26389,#26390));
#6212=EDGE_LOOP('',(#26391,#26392,#26393,#26394));
#6213=EDGE_LOOP('',(#26395,#26396,#26397,#26398));
#6214=EDGE_LOOP('',(#26399,#26400,#26401,#26402));
#6215=EDGE_LOOP('',(#26403,#26404,#26405,#26406));
#6216=EDGE_LOOP('',(#26407,#26408,#26409,#26410));
#6217=EDGE_LOOP('',(#26411,#26412,#26413,#26414,#26415));
#6218=EDGE_LOOP('',(#26416,#26417,#26418,#26419));
#6219=EDGE_LOOP('',(#26420,#26421,#26422,#26423,#26424));
#6220=EDGE_LOOP('',(#26425,#26426,#26427,#26428,#26429));
#6221=EDGE_LOOP('',(#26430,#26431,#26432));
#6222=EDGE_LOOP('',(#26433,#26434,#26435));
#6223=EDGE_LOOP('',(#26436,#26437,#26438,#26439));
#6224=EDGE_LOOP('',(#26440,#26441,#26442));
#6225=EDGE_LOOP('',(#26443,#26444,#26445,#26446));
#6226=EDGE_LOOP('',(#26447,#26448,#26449,#26450));
#6227=EDGE_LOOP('',(#26451,#26452,#26453,#26454));
#6228=EDGE_LOOP('',(#26455,#26456,#26457,#26458));
#6229=EDGE_LOOP('',(#26459,#26460,#26461,#26462));
#6230=EDGE_LOOP('',(#26463,#26464,#26465,#26466));
#6231=EDGE_LOOP('',(#26467,#26468,#26469));
#6232=EDGE_LOOP('',(#26470,#26471,#26472));
#6233=EDGE_LOOP('',(#26473,#26474,#26475));
#6234=EDGE_LOOP('',(#26476,#26477,#26478,#26479));
#6235=EDGE_LOOP('',(#26480,#26481,#26482));
#6236=EDGE_LOOP('',(#26483,#26484,#26485,#26486));
#6237=EDGE_LOOP('',(#26487,#26488,#26489,#26490));
#6238=EDGE_LOOP('',(#26491,#26492,#26493,#26494));
#6239=EDGE_LOOP('',(#26495,#26496,#26497,#26498));
#6240=EDGE_LOOP('',(#26499,#26500,#26501,#26502));
#6241=EDGE_LOOP('',(#26503,#26504,#26505,#26506));
#6242=EDGE_LOOP('',(#26507,#26508,#26509,#26510));
#6243=EDGE_LOOP('',(#26511,#26512,#26513,#26514));
#6244=EDGE_LOOP('',(#26515,#26516,#26517,#26518));
#6245=EDGE_LOOP('',(#26519,#26520,#26521,#26522));
#6246=EDGE_LOOP('',(#26523,#26524,#26525));
#6247=EDGE_LOOP('',(#26526,#26527,#26528,#26529,#26530));
#6248=EDGE_LOOP('',(#26531,#26532,#26533,#26534));
#6249=EDGE_LOOP('',(#26535,#26536,#26537));
#6250=EDGE_LOOP('',(#26538,#26539,#26540,#26541,#26542));
#6251=EDGE_LOOP('',(#26543,#26544,#26545,#26546));
#6252=EDGE_LOOP('',(#26547,#26548,#26549,#26550));
#6253=EDGE_LOOP('',(#26551,#26552,#26553,#26554,#26555));
#6254=EDGE_LOOP('',(#26556,#26557,#26558,#26559));
#6255=EDGE_LOOP('',(#26560,#26561,#26562,#26563,#26564,#26565));
#6256=EDGE_LOOP('',(#26566,#26567,#26568,#26569,#26570));
#6257=EDGE_LOOP('',(#26571,#26572,#26573,#26574));
#6258=EDGE_LOOP('',(#26575,#26576,#26577,#26578));
#6259=EDGE_LOOP('',(#26579,#26580,#26581));
#6260=EDGE_LOOP('',(#26582,#26583,#26584));
#6261=EDGE_LOOP('',(#26585,#26586,#26587));
#6262=EDGE_LOOP('',(#26588,#26589,#26590,#26591));
#6263=EDGE_LOOP('',(#26592,#26593,#26594));
#6264=EDGE_LOOP('',(#26595,#26596,#26597,#26598));
#6265=EDGE_LOOP('',(#26599,#26600,#26601,#26602));
#6266=EDGE_LOOP('',(#26603,#26604,#26605,#26606));
#6267=EDGE_LOOP('',(#26607,#26608,#26609,#26610));
#6268=EDGE_LOOP('',(#26611,#26612,#26613,#26614));
#6269=EDGE_LOOP('',(#26615,#26616,#26617,#26618));
#6270=EDGE_LOOP('',(#26619,#26620,#26621,#26622));
#6271=EDGE_LOOP('',(#26623,#26624,#26625,#26626));
#6272=EDGE_LOOP('',(#26627,#26628,#26629,#26630));
#6273=EDGE_LOOP('',(#26631,#26632,#26633,#26634));
#6274=EDGE_LOOP('',(#26635,#26636,#26637));
#6275=EDGE_LOOP('',(#26638,#26639,#26640));
#6276=EDGE_LOOP('',(#26641,#26642,#26643));
#6277=EDGE_LOOP('',(#26644,#26645,#26646,#26647));
#6278=EDGE_LOOP('',(#26648,#26649,#26650));
#6279=EDGE_LOOP('',(#26651,#26652,#26653,#26654));
#6280=EDGE_LOOP('',(#26655,#26656,#26657,#26658));
#6281=EDGE_LOOP('',(#26659,#26660,#26661,#26662));
#6282=EDGE_LOOP('',(#26663,#26664,#26665,#26666));
#6283=EDGE_LOOP('',(#26667,#26668,#26669,#26670));
#6284=EDGE_LOOP('',(#26671,#26672,#26673,#26674));
#6285=EDGE_LOOP('',(#26675,#26676,#26677,#26678));
#6286=EDGE_LOOP('',(#26679,#26680,#26681,#26682));
#6287=EDGE_LOOP('',(#26683,#26684,#26685,#26686));
#6288=EDGE_LOOP('',(#26687,#26688,#26689,#26690));
#6289=EDGE_LOOP('',(#26691,#26692,#26693,#26694,#26695));
#6290=EDGE_LOOP('',(#26696,#26697,#26698,#26699));
#6291=EDGE_LOOP('',(#26700,#26701,#26702,#26703,#26704));
#6292=EDGE_LOOP('',(#26705,#26706,#26707,#26708,#26709));
#6293=EDGE_LOOP('',(#26710,#26711,#26712));
#6294=EDGE_LOOP('',(#26713,#26714,#26715));
#6295=EDGE_LOOP('',(#26716,#26717,#26718,#26719));
#6296=EDGE_LOOP('',(#26720,#26721,#26722));
#6297=EDGE_LOOP('',(#26723,#26724,#26725,#26726));
#6298=EDGE_LOOP('',(#26727,#26728,#26729,#26730));
#6299=EDGE_LOOP('',(#26731,#26732,#26733,#26734));
#6300=EDGE_LOOP('',(#26735,#26736,#26737,#26738));
#6301=EDGE_LOOP('',(#26739,#26740,#26741,#26742));
#6302=EDGE_LOOP('',(#26743,#26744,#26745,#26746));
#6303=EDGE_LOOP('',(#26747,#26748,#26749));
#6304=EDGE_LOOP('',(#26750,#26751,#26752));
#6305=EDGE_LOOP('',(#26753,#26754,#26755));
#6306=EDGE_LOOP('',(#26756,#26757,#26758,#26759));
#6307=EDGE_LOOP('',(#26760,#26761,#26762));
#6308=EDGE_LOOP('',(#26763,#26764,#26765,#26766));
#6309=EDGE_LOOP('',(#26767,#26768,#26769,#26770));
#6310=EDGE_LOOP('',(#26771,#26772,#26773,#26774));
#6311=EDGE_LOOP('',(#26775,#26776,#26777,#26778));
#6312=EDGE_LOOP('',(#26779,#26780,#26781,#26782));
#6313=EDGE_LOOP('',(#26783,#26784,#26785,#26786));
#6314=EDGE_LOOP('',(#26787,#26788,#26789,#26790));
#6315=EDGE_LOOP('',(#26791,#26792,#26793,#26794));
#6316=EDGE_LOOP('',(#26795,#26796,#26797,#26798));
#6317=EDGE_LOOP('',(#26799,#26800,#26801,#26802));
#6318=EDGE_LOOP('',(#26803,#26804,#26805));
#6319=EDGE_LOOP('',(#26806,#26807,#26808,#26809,#26810));
#6320=EDGE_LOOP('',(#26811,#26812,#26813,#26814));
#6321=EDGE_LOOP('',(#26815,#26816,#26817));
#6322=EDGE_LOOP('',(#26818,#26819,#26820,#26821,#26822));
#6323=EDGE_LOOP('',(#26823,#26824,#26825,#26826));
#6324=EDGE_LOOP('',(#26827,#26828,#26829,#26830));
#6325=EDGE_LOOP('',(#26831,#26832,#26833,#26834,#26835));
#6326=EDGE_LOOP('',(#26836,#26837,#26838,#26839));
#6327=EDGE_LOOP('',(#26840,#26841,#26842,#26843,#26844,#26845));
#6328=EDGE_LOOP('',(#26846,#26847,#26848,#26849,#26850));
#6329=EDGE_LOOP('',(#26851,#26852,#26853,#26854));
#6330=EDGE_LOOP('',(#26855,#26856,#26857,#26858));
#6331=EDGE_LOOP('',(#26859,#26860,#26861));
#6332=EDGE_LOOP('',(#26862,#26863,#26864));
#6333=EDGE_LOOP('',(#26865,#26866,#26867));
#6334=EDGE_LOOP('',(#26868,#26869,#26870,#26871));
#6335=EDGE_LOOP('',(#26872,#26873,#26874));
#6336=EDGE_LOOP('',(#26875,#26876,#26877,#26878));
#6337=EDGE_LOOP('',(#26879,#26880,#26881,#26882));
#6338=EDGE_LOOP('',(#26883,#26884,#26885,#26886));
#6339=EDGE_LOOP('',(#26887,#26888,#26889,#26890));
#6340=EDGE_LOOP('',(#26891,#26892,#26893,#26894));
#6341=EDGE_LOOP('',(#26895,#26896,#26897,#26898));
#6342=EDGE_LOOP('',(#26899,#26900,#26901,#26902));
#6343=EDGE_LOOP('',(#26903,#26904,#26905,#26906));
#6344=EDGE_LOOP('',(#26907,#26908,#26909,#26910));
#6345=EDGE_LOOP('',(#26911,#26912,#26913,#26914));
#6346=EDGE_LOOP('',(#26915,#26916,#26917));
#6347=EDGE_LOOP('',(#26918,#26919,#26920));
#6348=EDGE_LOOP('',(#26921,#26922,#26923));
#6349=EDGE_LOOP('',(#26924,#26925,#26926,#26927));
#6350=EDGE_LOOP('',(#26928,#26929,#26930));
#6351=EDGE_LOOP('',(#26931,#26932,#26933,#26934));
#6352=EDGE_LOOP('',(#26935,#26936,#26937,#26938));
#6353=EDGE_LOOP('',(#26939,#26940,#26941,#26942));
#6354=EDGE_LOOP('',(#26943,#26944,#26945,#26946));
#6355=EDGE_LOOP('',(#26947,#26948,#26949,#26950));
#6356=EDGE_LOOP('',(#26951,#26952,#26953,#26954));
#6357=EDGE_LOOP('',(#26955,#26956,#26957,#26958));
#6358=EDGE_LOOP('',(#26959,#26960,#26961,#26962));
#6359=EDGE_LOOP('',(#26963,#26964,#26965,#26966));
#6360=EDGE_LOOP('',(#26967,#26968,#26969,#26970));
#6361=EDGE_LOOP('',(#26971,#26972,#26973,#26974,#26975,#26976));
#6362=EDGE_LOOP('',(#26977,#26978,#26979,#26980,#26981,#26982));
#6363=EDGE_LOOP('',(#26983,#26984,#26985,#26986,#26987));
#6364=EDGE_LOOP('',(#26988,#26989,#26990));
#6365=EDGE_LOOP('',(#26991,#26992,#26993));
#6366=EDGE_LOOP('',(#26994,#26995,#26996));
#6367=EDGE_LOOP('',(#26997,#26998,#26999,#27000));
#6368=EDGE_LOOP('',(#27001,#27002,#27003));
#6369=EDGE_LOOP('',(#27004,#27005,#27006,#27007));
#6370=EDGE_LOOP('',(#27008,#27009,#27010,#27011));
#6371=EDGE_LOOP('',(#27012,#27013,#27014,#27015));
#6372=EDGE_LOOP('',(#27016,#27017,#27018,#27019));
#6373=EDGE_LOOP('',(#27020,#27021,#27022,#27023));
#6374=EDGE_LOOP('',(#27024,#27025,#27026,#27027));
#6375=EDGE_LOOP('',(#27028,#27029,#27030,#27031));
#6376=EDGE_LOOP('',(#27032,#27033,#27034,#27035));
#6377=EDGE_LOOP('',(#27036,#27037,#27038,#27039));
#6378=EDGE_LOOP('',(#27040,#27041,#27042,#27043));
#6379=EDGE_LOOP('',(#27044,#27045,#27046));
#6380=EDGE_LOOP('',(#27047,#27048,#27049));
#6381=EDGE_LOOP('',(#27050,#27051,#27052));
#6382=EDGE_LOOP('',(#27053,#27054,#27055,#27056));
#6383=EDGE_LOOP('',(#27057,#27058,#27059));
#6384=EDGE_LOOP('',(#27060,#27061,#27062,#27063));
#6385=EDGE_LOOP('',(#27064,#27065,#27066,#27067));
#6386=EDGE_LOOP('',(#27068,#27069,#27070,#27071));
#6387=EDGE_LOOP('',(#27072,#27073,#27074,#27075));
#6388=EDGE_LOOP('',(#27076,#27077,#27078,#27079));
#6389=EDGE_LOOP('',(#27080,#27081,#27082,#27083));
#6390=EDGE_LOOP('',(#27084,#27085,#27086,#27087));
#6391=EDGE_LOOP('',(#27088,#27089,#27090,#27091));
#6392=EDGE_LOOP('',(#27092,#27093,#27094,#27095));
#6393=EDGE_LOOP('',(#27096,#27097,#27098,#27099));
#6394=EDGE_LOOP('',(#27100,#27101,#27102,#27103,#27104,#27105));
#6395=EDGE_LOOP('',(#27106,#27107,#27108,#27109,#27110,#27111));
#6396=EDGE_LOOP('',(#27112,#27113,#27114,#27115,#27116));
#6397=EDGE_LOOP('',(#27117,#27118,#27119,#27120,#27121));
#6398=EDGE_LOOP('',(#27122));
#6399=EDGE_LOOP('',(#27123));
#6400=EDGE_LOOP('',(#27124,#27125,#27126,#27127,#27128));
#6401=EDGE_LOOP('',(#27129,#27130,#27131,#27132));
#6402=EDGE_LOOP('',(#27133,#27134,#27135,#27136));
#6403=EDGE_LOOP('',(#27137,#27138,#27139,#27140));
#6404=EDGE_LOOP('',(#27141,#27142,#27143,#27144));
#6405=EDGE_LOOP('',(#27145,#27146,#27147,#27148));
#6406=EDGE_LOOP('',(#27149,#27150,#27151,#27152));
#6407=EDGE_LOOP('',(#27153,#27154,#27155,#27156));
#6408=EDGE_LOOP('',(#27157,#27158,#27159,#27160));
#6409=EDGE_LOOP('',(#27161,#27162,#27163,#27164));
#6410=EDGE_LOOP('',(#27165,#27166,#27167,#27168));
#6411=EDGE_LOOP('',(#27169,#27170,#27171,#27172));
#6412=EDGE_LOOP('',(#27173,#27174,#27175,#27176));
#6413=EDGE_LOOP('',(#27177,#27178,#27179,#27180));
#6414=EDGE_LOOP('',(#27181,#27182,#27183,#27184));
#6415=EDGE_LOOP('',(#27185,#27186,#27187,#27188));
#6416=EDGE_LOOP('',(#27189,#27190,#27191,#27192));
#6417=EDGE_LOOP('',(#27193,#27194,#27195,#27196));
#6418=EDGE_LOOP('',(#27197,#27198,#27199,#27200));
#6419=EDGE_LOOP('',(#27201,#27202,#27203,#27204));
#6420=EDGE_LOOP('',(#27205,#27206,#27207,#27208));
#6421=EDGE_LOOP('',(#27209,#27210,#27211,#27212));
#6422=EDGE_LOOP('',(#27213,#27214,#27215,#27216));
#6423=EDGE_LOOP('',(#27217,#27218,#27219,#27220));
#6424=EDGE_LOOP('',(#27221,#27222,#27223,#27224));
#6425=EDGE_LOOP('',(#27225,#27226,#27227,#27228));
#6426=EDGE_LOOP('',(#27229,#27230,#27231,#27232));
#6427=EDGE_LOOP('',(#27233,#27234,#27235,#27236));
#6428=EDGE_LOOP('',(#27237,#27238,#27239,#27240));
#6429=EDGE_LOOP('',(#27241,#27242,#27243,#27244));
#6430=EDGE_LOOP('',(#27245,#27246,#27247,#27248));
#6431=EDGE_LOOP('',(#27249,#27250,#27251,#27252));
#6432=EDGE_LOOP('',(#27253,#27254,#27255,#27256));
#6433=EDGE_LOOP('',(#27257,#27258,#27259,#27260));
#6434=EDGE_LOOP('',(#27261,#27262,#27263,#27264));
#6435=EDGE_LOOP('',(#27265,#27266,#27267,#27268));
#6436=EDGE_LOOP('',(#27269,#27270,#27271,#27272));
#6437=EDGE_LOOP('',(#27273,#27274,#27275,#27276));
#6438=EDGE_LOOP('',(#27277,#27278,#27279,#27280));
#6439=EDGE_LOOP('',(#27281,#27282,#27283,#27284));
#6440=EDGE_LOOP('',(#27285,#27286,#27287,#27288));
#6441=EDGE_LOOP('',(#27289,#27290,#27291,#27292));
#6442=EDGE_LOOP('',(#27293,#27294,#27295,#27296));
#6443=EDGE_LOOP('',(#27297,#27298,#27299,#27300));
#6444=EDGE_LOOP('',(#27301,#27302,#27303,#27304));
#6445=EDGE_LOOP('',(#27305,#27306,#27307,#27308));
#6446=EDGE_LOOP('',(#27309,#27310,#27311,#27312));
#6447=EDGE_LOOP('',(#27313,#27314,#27315,#27316));
#6448=EDGE_LOOP('',(#27317,#27318,#27319,#27320));
#6449=EDGE_LOOP('',(#27321,#27322,#27323,#27324));
#6450=EDGE_LOOP('',(#27325,#27326,#27327,#27328));
#6451=EDGE_LOOP('',(#27329,#27330,#27331,#27332));
#6452=EDGE_LOOP('',(#27333,#27334,#27335,#27336));
#6453=EDGE_LOOP('',(#27337,#27338,#27339,#27340));
#6454=EDGE_LOOP('',(#27341,#27342,#27343,#27344));
#6455=EDGE_LOOP('',(#27345,#27346,#27347,#27348));
#6456=EDGE_LOOP('',(#27349,#27350,#27351,#27352));
#6457=EDGE_LOOP('',(#27353,#27354,#27355,#27356));
#6458=EDGE_LOOP('',(#27357,#27358,#27359,#27360));
#6459=EDGE_LOOP('',(#27361,#27362,#27363,#27364));
#6460=EDGE_LOOP('',(#27365,#27366,#27367,#27368));
#6461=EDGE_LOOP('',(#27369,#27370,#27371,#27372));
#6462=EDGE_LOOP('',(#27373,#27374,#27375,#27376));
#6463=EDGE_LOOP('',(#27377,#27378,#27379,#27380));
#6464=EDGE_LOOP('',(#27381,#27382,#27383,#27384));
#6465=EDGE_LOOP('',(#27385,#27386,#27387,#27388));
#6466=EDGE_LOOP('',(#27389,#27390,#27391,#27392));
#6467=EDGE_LOOP('',(#27393,#27394,#27395,#27396));
#6468=EDGE_LOOP('',(#27397,#27398,#27399,#27400));
#6469=EDGE_LOOP('',(#27401,#27402,#27403,#27404));
#6470=EDGE_LOOP('',(#27405,#27406,#27407,#27408));
#6471=EDGE_LOOP('',(#27409,#27410,#27411,#27412));
#6472=EDGE_LOOP('',(#27413,#27414,#27415,#27416));
#6473=EDGE_LOOP('',(#27417,#27418,#27419,#27420));
#6474=EDGE_LOOP('',(#27421,#27422,#27423,#27424));
#6475=EDGE_LOOP('',(#27425,#27426,#27427,#27428));
#6476=EDGE_LOOP('',(#27429,#27430,#27431,#27432));
#6477=EDGE_LOOP('',(#27433,#27434,#27435,#27436));
#6478=EDGE_LOOP('',(#27437,#27438,#27439,#27440));
#6479=EDGE_LOOP('',(#27441,#27442,#27443,#27444));
#6480=EDGE_LOOP('',(#27445,#27446,#27447,#27448));
#6481=EDGE_LOOP('',(#27449,#27450,#27451,#27452));
#6482=EDGE_LOOP('',(#27453,#27454,#27455,#27456));
#6483=EDGE_LOOP('',(#27457,#27458,#27459,#27460));
#6484=EDGE_LOOP('',(#27461,#27462,#27463,#27464));
#6485=EDGE_LOOP('',(#27465,#27466,#27467,#27468));
#6486=EDGE_LOOP('',(#27469,#27470,#27471,#27472));
#6487=EDGE_LOOP('',(#27473,#27474,#27475,#27476));
#6488=EDGE_LOOP('',(#27477,#27478,#27479,#27480));
#6489=EDGE_LOOP('',(#27481,#27482,#27483,#27484));
#6490=EDGE_LOOP('',(#27485,#27486,#27487,#27488));
#6491=EDGE_LOOP('',(#27489,#27490,#27491,#27492));
#6492=EDGE_LOOP('',(#27493,#27494,#27495,#27496));
#6493=EDGE_LOOP('',(#27497,#27498,#27499,#27500));
#6494=EDGE_LOOP('',(#27501,#27502,#27503,#27504));
#6495=EDGE_LOOP('',(#27505,#27506,#27507,#27508));
#6496=EDGE_LOOP('',(#27509,#27510,#27511,#27512));
#6497=EDGE_LOOP('',(#27513,#27514,#27515,#27516));
#6498=EDGE_LOOP('',(#27517,#27518,#27519,#27520));
#6499=EDGE_LOOP('',(#27521,#27522,#27523,#27524));
#6500=EDGE_LOOP('',(#27525,#27526,#27527,#27528));
#6501=EDGE_LOOP('',(#27529,#27530,#27531,#27532));
#6502=EDGE_LOOP('',(#27533,#27534,#27535,#27536));
#6503=EDGE_LOOP('',(#27537,#27538,#27539,#27540));
#6504=EDGE_LOOP('',(#27541,#27542,#27543,#27544));
#6505=EDGE_LOOP('',(#27545,#27546,#27547,#27548));
#6506=EDGE_LOOP('',(#27549,#27550,#27551,#27552));
#6507=EDGE_LOOP('',(#27553,#27554,#27555,#27556));
#6508=EDGE_LOOP('',(#27557,#27558,#27559,#27560));
#6509=EDGE_LOOP('',(#27561,#27562,#27563,#27564));
#6510=EDGE_LOOP('',(#27565,#27566,#27567,#27568,#27569));
#6511=EDGE_LOOP('',(#27570,#27571,#27572,#27573));
#6512=EDGE_LOOP('',(#27574,#27575,#27576,#27577));
#6513=EDGE_LOOP('',(#27578,#27579,#27580,#27581));
#6514=EDGE_LOOP('',(#27582,#27583,#27584,#27585));
#6515=EDGE_LOOP('',(#27586,#27587,#27588,#27589));
#6516=EDGE_LOOP('',(#27590,#27591,#27592,#27593));
#6517=EDGE_LOOP('',(#27594,#27595,#27596,#27597));
#6518=EDGE_LOOP('',(#27598,#27599,#27600,#27601));
#6519=EDGE_LOOP('',(#27602,#27603,#27604,#27605));
#6520=EDGE_LOOP('',(#27606,#27607,#27608,#27609));
#6521=EDGE_LOOP('',(#27610,#27611,#27612,#27613));
#6522=EDGE_LOOP('',(#27614,#27615,#27616,#27617));
#6523=EDGE_LOOP('',(#27618,#27619,#27620,#27621));
#6524=EDGE_LOOP('',(#27622,#27623,#27624,#27625));
#6525=EDGE_LOOP('',(#27626,#27627,#27628,#27629));
#6526=EDGE_LOOP('',(#27630,#27631,#27632,#27633));
#6527=EDGE_LOOP('',(#27634,#27635,#27636,#27637));
#6528=EDGE_LOOP('',(#27638,#27639,#27640,#27641));
#6529=EDGE_LOOP('',(#27642,#27643,#27644,#27645));
#6530=EDGE_LOOP('',(#27646,#27647,#27648,#27649));
#6531=EDGE_LOOP('',(#27650,#27651,#27652,#27653));
#6532=EDGE_LOOP('',(#27654,#27655,#27656,#27657));
#6533=EDGE_LOOP('',(#27658,#27659,#27660,#27661));
#6534=EDGE_LOOP('',(#27662,#27663,#27664,#27665));
#6535=EDGE_LOOP('',(#27666,#27667,#27668,#27669));
#6536=EDGE_LOOP('',(#27670,#27671,#27672,#27673));
#6537=EDGE_LOOP('',(#27674,#27675,#27676,#27677));
#6538=EDGE_LOOP('',(#27678,#27679,#27680,#27681));
#6539=EDGE_LOOP('',(#27682,#27683,#27684,#27685));
#6540=EDGE_LOOP('',(#27686,#27687,#27688,#27689));
#6541=EDGE_LOOP('',(#27690,#27691,#27692,#27693));
#6542=EDGE_LOOP('',(#27694,#27695,#27696,#27697));
#6543=EDGE_LOOP('',(#27698,#27699,#27700,#27701));
#6544=EDGE_LOOP('',(#27702,#27703,#27704,#27705));
#6545=EDGE_LOOP('',(#27706,#27707,#27708,#27709));
#6546=EDGE_LOOP('',(#27710,#27711,#27712,#27713));
#6547=EDGE_LOOP('',(#27714,#27715,#27716,#27717));
#6548=EDGE_LOOP('',(#27718,#27719,#27720,#27721));
#6549=EDGE_LOOP('',(#27722,#27723,#27724,#27725));
#6550=EDGE_LOOP('',(#27726,#27727,#27728,#27729));
#6551=EDGE_LOOP('',(#27730,#27731,#27732,#27733));
#6552=EDGE_LOOP('',(#27734,#27735,#27736,#27737));
#6553=EDGE_LOOP('',(#27738,#27739,#27740,#27741));
#6554=EDGE_LOOP('',(#27742,#27743,#27744,#27745));
#6555=EDGE_LOOP('',(#27746,#27747,#27748,#27749));
#6556=EDGE_LOOP('',(#27750,#27751,#27752,#27753));
#6557=EDGE_LOOP('',(#27754,#27755,#27756,#27757));
#6558=EDGE_LOOP('',(#27758));
#6559=EDGE_LOOP('',(#27759,#27760,#27761,#27762,#27763,#27764,#27765,#27766,
#27767,#27768));
#6560=EDGE_LOOP('',(#27769,#27770,#27771,#27772));
#6561=EDGE_LOOP('',(#27773));
#6562=EDGE_LOOP('',(#27774));
#6563=EDGE_LOOP('',(#27775,#27776,#27777,#27778));
#6564=EDGE_LOOP('',(#27779));
#6565=EDGE_LOOP('',(#27780));
#6566=EDGE_LOOP('',(#27781,#27782,#27783,#27784));
#6567=EDGE_LOOP('',(#27785));
#6568=EDGE_LOOP('',(#27786));
#6569=EDGE_LOOP('',(#27787,#27788,#27789,#27790));
#6570=EDGE_LOOP('',(#27791,#27792,#27793,#27794));
#6571=EDGE_LOOP('',(#27795,#27796,#27797,#27798));
#6572=EDGE_LOOP('',(#27799));
#6573=EDGE_LOOP('',(#27800));
#6574=EDGE_LOOP('',(#27801));
#6575=EDGE_LOOP('',(#27802));
#6576=EDGE_LOOP('',(#27803));
#6577=EDGE_LOOP('',(#27804));
#6578=EDGE_LOOP('',(#27805));
#6579=EDGE_LOOP('',(#27806,#27807,#27808,#27809));
#6580=EDGE_LOOP('',(#27810,#27811,#27812,#27813));
#6581=EDGE_LOOP('',(#27814,#27815,#27816,#27817,#27818,#27819,#27820));
#6582=EDGE_LOOP('',(#27821,#27822,#27823,#27824));
#6583=EDGE_LOOP('',(#27825,#27826,#27827,#27828));
#6584=EDGE_LOOP('',(#27829,#27830,#27831,#27832));
#6585=EDGE_LOOP('',(#27833,#27834,#27835,#27836));
#6586=EDGE_LOOP('',(#27837,#27838,#27839,#27840));
#6587=EDGE_LOOP('',(#27841,#27842,#27843,#27844));
#6588=EDGE_LOOP('',(#27845,#27846,#27847,#27848));
#6589=EDGE_LOOP('',(#27849,#27850,#27851,#27852));
#6590=EDGE_LOOP('',(#27853,#27854,#27855,#27856));
#6591=EDGE_LOOP('',(#27857,#27858,#27859));
#6592=EDGE_LOOP('',(#27860));
#6593=EDGE_LOOP('',(#27861));
#6594=EDGE_LOOP('',(#27862,#27863,#27864,#27865));
#6595=EDGE_LOOP('',(#27866,#27867,#27868,#27869));
#6596=EDGE_LOOP('',(#27870,#27871,#27872,#27873,#27874,#27875));
#6597=EDGE_LOOP('',(#27876,#27877,#27878,#27879));
#6598=EDGE_LOOP('',(#27880,#27881,#27882,#27883,#27884));
#6599=EDGE_LOOP('',(#27885,#27886,#27887,#27888,#27889,#27890));
#6600=EDGE_LOOP('',(#27891,#27892,#27893));
#6601=EDGE_LOOP('',(#27894,#27895,#27896,#27897,#27898));
#6602=EDGE_LOOP('',(#27899,#27900,#27901,#27902,#27903));
#6603=EDGE_LOOP('',(#27904,#27905,#27906));
#6604=EDGE_LOOP('',(#27907,#27908,#27909,#27910,#27911));
#6605=EDGE_LOOP('',(#27912,#27913,#27914,#27915));
#6606=EDGE_LOOP('',(#27916,#27917,#27918));
#6607=EDGE_LOOP('',(#27919,#27920,#27921,#27922,#27923));
#6608=EDGE_LOOP('',(#27924,#27925,#27926,#27927));
#6609=EDGE_LOOP('',(#27928,#27929,#27930));
#6610=EDGE_LOOP('',(#27931,#27932,#27933,#27934,#27935));
#6611=EDGE_LOOP('',(#27936,#27937,#27938,#27939));
#6612=EDGE_LOOP('',(#27940,#27941,#27942));
#6613=EDGE_LOOP('',(#27943,#27944,#27945,#27946,#27947));
#6614=EDGE_LOOP('',(#27948,#27949,#27950,#27951));
#6615=EDGE_LOOP('',(#27952,#27953,#27954));
#6616=EDGE_LOOP('',(#27955,#27956,#27957,#27958,#27959));
#6617=EDGE_LOOP('',(#27960,#27961,#27962,#27963));
#6618=EDGE_LOOP('',(#27964,#27965,#27966,#27967,#27968));
#6619=EDGE_LOOP('',(#27969,#27970,#27971,#27972,#27973,#27974));
#6620=EDGE_LOOP('',(#27975,#27976,#27977,#27978));
#6621=EDGE_LOOP('',(#27979,#27980,#27981,#27982,#27983,#27984));
#6622=EDGE_LOOP('',(#27985,#27986,#27987,#27988));
#6623=EDGE_LOOP('',(#27989,#27990,#27991,#27992,#27993,#27994));
#6624=EDGE_LOOP('',(#27995,#27996,#27997,#27998));
#6625=EDGE_LOOP('',(#27999,#28000,#28001,#28002,#28003,#28004));
#6626=EDGE_LOOP('',(#28005,#28006,#28007,#28008,#28009));
#6627=EDGE_LOOP('',(#28010,#28011,#28012,#28013));
#6628=EDGE_LOOP('',(#28014,#28015,#28016,#28017,#28018));
#6629=EDGE_LOOP('',(#28019,#28020,#28021,#28022));
#6630=EDGE_LOOP('',(#28023,#28024,#28025,#28026,#28027,#28028,#28029,#28030));
#6631=EDGE_LOOP('',(#28031));
#6632=EDGE_LOOP('',(#28032));
#6633=EDGE_LOOP('',(#28033));
#6634=EDGE_LOOP('',(#28034));
#6635=EDGE_LOOP('',(#28035));
#6636=EDGE_LOOP('',(#28036,#28037,#28038,#28039));
#6637=EDGE_LOOP('',(#28040,#28041,#28042,#28043));
#6638=EDGE_LOOP('',(#28044,#28045,#28046,#28047));
#6639=EDGE_LOOP('',(#28048,#28049,#28050,#28051));
#6640=EDGE_LOOP('',(#28052,#28053,#28054,#28055));
#6641=EDGE_LOOP('',(#28056,#28057,#28058,#28059));
#6642=EDGE_LOOP('',(#28060,#28061,#28062,#28063));
#6643=EDGE_LOOP('',(#28064,#28065,#28066,#28067));
#6644=EDGE_LOOP('',(#28068,#28069,#28070,#28071,#28072,#28073,#28074,#28075));
#6645=EDGE_LOOP('',(#28076));
#6646=EDGE_LOOP('',(#28077));
#6647=EDGE_LOOP('',(#28078));
#6648=EDGE_LOOP('',(#28079));
#6649=EDGE_LOOP('',(#28080));
#6650=EDGE_LOOP('',(#28081,#28082,#28083,#28084));
#6651=EDGE_LOOP('',(#28085,#28086,#28087,#28088));
#6652=EDGE_LOOP('',(#28089,#28090,#28091,#28092));
#6653=EDGE_LOOP('',(#28093,#28094,#28095,#28096,#28097,#28098));
#6654=EDGE_LOOP('',(#28099,#28100,#28101));
#6655=EDGE_LOOP('',(#28102,#28103,#28104,#28105,#28106,#28107));
#6656=EDGE_LOOP('',(#28108,#28109,#28110,#28111));
#6657=EDGE_LOOP('',(#28112,#28113,#28114,#28115));
#6658=EDGE_LOOP('',(#28116,#28117,#28118,#28119));
#6659=EDGE_LOOP('',(#28120,#28121,#28122,#28123,#28124,#28125));
#6660=EDGE_LOOP('',(#28126,#28127,#28128,#28129,#28130,#28131));
#6661=EDGE_LOOP('',(#28132,#28133,#28134,#28135,#28136));
#6662=EDGE_LOOP('',(#28137,#28138,#28139,#28140,#28141));
#6663=EDGE_LOOP('',(#28142));
#6664=EDGE_LOOP('',(#28143,#28144,#28145,#28146,#28147));
#6665=EDGE_LOOP('',(#28148,#28149,#28150,#28151,#28152,#28153,#28154,#28155,
#28156,#28157,#28158,#28159,#28160,#28161));
#6666=EDGE_LOOP('',(#28162,#28163,#28164,#28165,#28166,#28167,#28168,#28169,
#28170,#28171,#28172,#28173,#28174,#28175,#28176,#28177,#28178,#28179,#28180,
#28181,#28182,#28183,#28184));
#6667=EDGE_LOOP('',(#28185,#28186,#28187,#28188));
#6668=EDGE_LOOP('',(#28189,#28190,#28191,#28192));
#6669=EDGE_LOOP('',(#28193,#28194,#28195,#28196));
#6670=EDGE_LOOP('',(#28197,#28198,#28199,#28200,#28201,#28202,#28203,#28204,
#28205,#28206,#28207,#28208,#28209));
#6671=EDGE_LOOP('',(#28210,#28211,#28212,#28213));
#6672=EDGE_LOOP('',(#28214,#28215,#28216,#28217));
#6673=EDGE_LOOP('',(#28218,#28219,#28220,#28221,#28222,#28223,#28224,#28225,
#28226,#28227,#28228,#28229,#28230,#28231,#28232,#28233,#28234,#28235,#28236,
#28237,#28238,#28239));
#6674=EDGE_LOOP('',(#28240,#28241,#28242,#28243));
#6675=EDGE_LOOP('',(#28244,#28245,#28246,#28247,#28248,#28249));
#6676=EDGE_LOOP('',(#28250,#28251,#28252,#28253));
#6677=EDGE_LOOP('',(#28254,#28255,#28256,#28257));
#6678=EDGE_LOOP('',(#28258,#28259,#28260,#28261));
#6679=EDGE_LOOP('',(#28262,#28263,#28264,#28265));
#6680=EDGE_LOOP('',(#28266,#28267,#28268,#28269,#28270));
#6681=EDGE_LOOP('',(#28271,#28272,#28273,#28274,#28275,#28276,#28277));
#6682=EDGE_LOOP('',(#28278,#28279,#28280,#28281));
#6683=EDGE_LOOP('',(#28282,#28283,#28284));
#6684=EDGE_LOOP('',(#28285,#28286,#28287,#28288));
#6685=EDGE_LOOP('',(#28289,#28290,#28291,#28292));
#6686=EDGE_LOOP('',(#28293,#28294,#28295,#28296));
#6687=EDGE_LOOP('',(#28297,#28298,#28299,#28300));
#6688=EDGE_LOOP('',(#28301,#28302,#28303,#28304));
#6689=EDGE_LOOP('',(#28305,#28306,#28307,#28308));
#6690=EDGE_LOOP('',(#28309,#28310,#28311,#28312));
#6691=EDGE_LOOP('',(#28313,#28314,#28315,#28316));
#6692=EDGE_LOOP('',(#28317,#28318,#28319,#28320));
#6693=EDGE_LOOP('',(#28321,#28322,#28323,#28324,#28325,#28326));
#6694=EDGE_LOOP('',(#28327,#28328,#28329,#28330));
#6695=EDGE_LOOP('',(#28331,#28332,#28333,#28334));
#6696=EDGE_LOOP('',(#28335,#28336,#28337,#28338));
#6697=EDGE_LOOP('',(#28339,#28340,#28341,#28342,#28343));
#6698=EDGE_LOOP('',(#28344,#28345,#28346));
#6699=EDGE_LOOP('',(#28347,#28348,#28349,#28350));
#6700=EDGE_LOOP('',(#28351,#28352,#28353,#28354));
#6701=EDGE_LOOP('',(#28355,#28356,#28357,#28358));
#6702=EDGE_LOOP('',(#28359,#28360,#28361,#28362));
#6703=EDGE_LOOP('',(#28363,#28364,#28365,#28366));
#6704=EDGE_LOOP('',(#28367,#28368,#28369,#28370));
#6705=EDGE_LOOP('',(#28371,#28372,#28373,#28374));
#6706=EDGE_LOOP('',(#28375,#28376,#28377,#28378,#28379,#28380,#28381,#28382));
#6707=EDGE_LOOP('',(#28383,#28384,#28385,#28386));
#6708=EDGE_LOOP('',(#28387,#28388,#28389,#28390,#28391,#28392,#28393,#28394,
#28395,#28396,#28397,#28398,#28399,#28400,#28401,#28402,#28403,#28404,#28405,
#28406,#28407,#28408,#28409,#28410,#28411,#28412,#28413,#28414,#28415,#28416,
#28417,#28418,#28419,#28420,#28421,#28422,#28423,#28424,#28425,#28426,#28427,
#28428,#28429,#28430,#28431));
#6709=EDGE_LOOP('',(#28432,#28433,#28434,#28435));
#6710=EDGE_LOOP('',(#28436,#28437,#28438,#28439));
#6711=EDGE_LOOP('',(#28440));
#6712=EDGE_LOOP('',(#28441));
#6713=EDGE_LOOP('',(#28442,#28443,#28444,#28445));
#6714=EDGE_LOOP('',(#28446,#28447,#28448,#28449));
#6715=EDGE_LOOP('',(#28450,#28451,#28452,#28453));
#6716=EDGE_LOOP('',(#28454,#28455,#28456,#28457));
#6717=EDGE_LOOP('',(#28458,#28459,#28460,#28461));
#6718=EDGE_LOOP('',(#28462,#28463,#28464,#28465,#28466));
#6719=EDGE_LOOP('',(#28467,#28468,#28469,#28470,#28471,#28472,#28473,#28474));
#6720=EDGE_LOOP('',(#28475,#28476,#28477,#28478,#28479));
#6721=EDGE_LOOP('',(#28480,#28481,#28482,#28483,#28484));
#6722=EDGE_LOOP('',(#28485));
#6723=EDGE_LOOP('',(#28486,#28487,#28488,#28489));
#6724=EDGE_LOOP('',(#28490,#28491,#28492,#28493,#28494,#28495,#28496,#28497));
#6725=EDGE_LOOP('',(#28498,#28499,#28500,#28501,#28502,#28503,#28504,#28505));
#6726=EDGE_LOOP('',(#28506,#28507));
#6727=EDGE_LOOP('',(#28508,#28509,#28510,#28511));
#6728=EDGE_LOOP('',(#28512,#28513,#28514,#28515,#28516));
#6729=EDGE_LOOP('',(#28517));
#6730=EDGE_LOOP('',(#28518));
#6731=EDGE_LOOP('',(#28519,#28520,#28521,#28522,#28523));
#6732=EDGE_LOOP('',(#28524,#28525,#28526,#28527,#28528));
#6733=EDGE_LOOP('',(#28529));
#6734=EDGE_LOOP('',(#28530));
#6735=EDGE_LOOP('',(#28531,#28532,#28533,#28534,#28535));
#6736=EDGE_LOOP('',(#28536,#28537,#28538,#28539));
#6737=EDGE_LOOP('',(#28540));
#6738=EDGE_LOOP('',(#28541));
#6739=EDGE_LOOP('',(#28542,#28543,#28544,#28545));
#6740=EDGE_LOOP('',(#28546,#28547,#28548,#28549));
#6741=EDGE_LOOP('',(#28550,#28551,#28552,#28553));
#6742=EDGE_LOOP('',(#28554,#28555,#28556,#28557));
#6743=EDGE_LOOP('',(#28558,#28559,#28560,#28561));
#6744=EDGE_LOOP('',(#28562,#28563,#28564,#28565));
#6745=EDGE_LOOP('',(#28566,#28567,#28568,#28569));
#6746=EDGE_LOOP('',(#28570));
#6747=EDGE_LOOP('',(#28571));
#6748=EDGE_LOOP('',(#28572,#28573,#28574,#28575));
#6749=EDGE_LOOP('',(#28576,#28577,#28578,#28579));
#6750=EDGE_LOOP('',(#28580,#28581,#28582,#28583));
#6751=EDGE_LOOP('',(#28584));
#6752=EDGE_LOOP('',(#28585));
#6753=EDGE_LOOP('',(#28586,#28587,#28588,#28589));
#6754=EDGE_LOOP('',(#28590,#28591,#28592,#28593));
#6755=EDGE_LOOP('',(#28594,#28595,#28596,#28597));
#6756=EDGE_LOOP('',(#28598));
#6757=EDGE_LOOP('',(#28599));
#6758=EDGE_LOOP('',(#28600,#28601,#28602,#28603,#28604));
#6759=EDGE_LOOP('',(#28605));
#6760=EDGE_LOOP('',(#28606));
#6761=EDGE_LOOP('',(#28607,#28608,#28609,#28610,#28611));
#6762=EDGE_LOOP('',(#28612,#28613,#28614,#28615,#28616));
#6763=EDGE_LOOP('',(#28617,#28618,#28619,#28620,#28621));
#6764=EDGE_LOOP('',(#28622));
#6765=EDGE_LOOP('',(#28623));
#6766=EDGE_LOOP('',(#28624,#28625,#28626,#28627,#28628,#28629));
#6767=EDGE_LOOP('',(#28630,#28631,#28632,#28633,#28634,#28635));
#6768=EDGE_LOOP('',(#28636,#28637,#28638,#28639,#28640,#28641));
#6769=EDGE_LOOP('',(#28642));
#6770=EDGE_LOOP('',(#28643));
#6771=EDGE_LOOP('',(#28644,#28645,#28646,#28647,#28648,#28649));
#6772=EDGE_LOOP('',(#28650,#28651,#28652,#28653,#28654,#28655));
#6773=EDGE_LOOP('',(#28656,#28657,#28658,#28659,#28660,#28661));
#6774=EDGE_LOOP('',(#28662));
#6775=EDGE_LOOP('',(#28663));
#6776=EDGE_LOOP('',(#28664,#28665,#28666,#28667,#28668,#28669));
#6777=EDGE_LOOP('',(#28670,#28671,#28672,#28673,#28674,#28675));
#6778=EDGE_LOOP('',(#28676,#28677,#28678,#28679,#28680,#28681));
#6779=EDGE_LOOP('',(#28682));
#6780=EDGE_LOOP('',(#28683));
#6781=EDGE_LOOP('',(#28684,#28685,#28686,#28687,#28688,#28689));
#6782=EDGE_LOOP('',(#28690,#28691,#28692,#28693,#28694,#28695));
#6783=EDGE_LOOP('',(#28696,#28697,#28698,#28699,#28700,#28701));
#6784=EDGE_LOOP('',(#28702));
#6785=EDGE_LOOP('',(#28703));
#6786=EDGE_LOOP('',(#28704,#28705,#28706,#28707,#28708,#28709));
#6787=EDGE_LOOP('',(#28710,#28711,#28712,#28713,#28714,#28715));
#6788=EDGE_LOOP('',(#28716,#28717,#28718,#28719,#28720,#28721));
#6789=EDGE_LOOP('',(#28722));
#6790=EDGE_LOOP('',(#28723));
#6791=EDGE_LOOP('',(#28724,#28725,#28726,#28727,#28728,#28729));
#6792=EDGE_LOOP('',(#28730,#28731,#28732,#28733,#28734,#28735));
#6793=EDGE_LOOP('',(#28736,#28737,#28738,#28739,#28740,#28741));
#6794=EDGE_LOOP('',(#28742));
#6795=EDGE_LOOP('',(#28743));
#6796=EDGE_LOOP('',(#28744,#28745,#28746,#28747,#28748,#28749));
#6797=EDGE_LOOP('',(#28750,#28751,#28752,#28753,#28754,#28755));
#6798=EDGE_LOOP('',(#28756,#28757,#28758,#28759,#28760,#28761));
#6799=EDGE_LOOP('',(#28762));
#6800=EDGE_LOOP('',(#28763));
#6801=EDGE_LOOP('',(#28764,#28765,#28766,#28767,#28768,#28769));
#6802=EDGE_LOOP('',(#28770,#28771,#28772,#28773,#28774,#28775));
#6803=EDGE_LOOP('',(#28776,#28777,#28778,#28779,#28780,#28781));
#6804=EDGE_LOOP('',(#28782));
#6805=EDGE_LOOP('',(#28783));
#6806=EDGE_LOOP('',(#28784,#28785,#28786,#28787,#28788,#28789));
#6807=EDGE_LOOP('',(#28790,#28791,#28792,#28793,#28794,#28795));
#6808=EDGE_LOOP('',(#28796,#28797,#28798,#28799,#28800,#28801));
#6809=EDGE_LOOP('',(#28802));
#6810=EDGE_LOOP('',(#28803));
#6811=EDGE_LOOP('',(#28804,#28805,#28806,#28807,#28808,#28809));
#6812=EDGE_LOOP('',(#28810,#28811,#28812,#28813,#28814,#28815));
#6813=EDGE_LOOP('',(#28816,#28817,#28818,#28819,#28820,#28821));
#6814=EDGE_LOOP('',(#28822));
#6815=EDGE_LOOP('',(#28823));
#6816=EDGE_LOOP('',(#28824,#28825,#28826,#28827,#28828,#28829,#28830));
#6817=EDGE_LOOP('',(#28831,#28832,#28833,#28834,#28835,#28836));
#6818=EDGE_LOOP('',(#28837,#28838,#28839,#28840,#28841,#28842,#28843));
#6819=EDGE_LOOP('',(#28844));
#6820=EDGE_LOOP('',(#28845));
#6821=EDGE_LOOP('',(#28846,#28847,#28848,#28849,#28850,#28851));
#6822=EDGE_LOOP('',(#28852,#28853,#28854,#28855,#28856,#28857));
#6823=EDGE_LOOP('',(#28858,#28859,#28860,#28861,#28862,#28863));
#6824=EDGE_LOOP('',(#28864));
#6825=EDGE_LOOP('',(#28865));
#6826=EDGE_LOOP('',(#28866,#28867,#28868,#28869,#28870,#28871));
#6827=EDGE_LOOP('',(#28872,#28873,#28874,#28875,#28876,#28877));
#6828=EDGE_LOOP('',(#28878,#28879,#28880,#28881,#28882,#28883));
#6829=EDGE_LOOP('',(#28884));
#6830=EDGE_LOOP('',(#28885));
#6831=EDGE_LOOP('',(#28886,#28887,#28888,#28889,#28890,#28891));
#6832=EDGE_LOOP('',(#28892,#28893,#28894,#28895,#28896,#28897));
#6833=EDGE_LOOP('',(#28898,#28899,#28900,#28901,#28902,#28903));
#6834=EDGE_LOOP('',(#28904));
#6835=EDGE_LOOP('',(#28905));
#6836=EDGE_LOOP('',(#28906,#28907,#28908,#28909,#28910,#28911));
#6837=EDGE_LOOP('',(#28912,#28913,#28914,#28915,#28916,#28917));
#6838=EDGE_LOOP('',(#28918,#28919,#28920,#28921,#28922,#28923));
#6839=EDGE_LOOP('',(#28924));
#6840=EDGE_LOOP('',(#28925));
#6841=EDGE_LOOP('',(#28926,#28927,#28928,#28929,#28930,#28931));
#6842=EDGE_LOOP('',(#28932,#28933,#28934,#28935,#28936,#28937));
#6843=EDGE_LOOP('',(#28938,#28939,#28940,#28941,#28942,#28943));
#6844=EDGE_LOOP('',(#28944));
#6845=EDGE_LOOP('',(#28945));
#6846=EDGE_LOOP('',(#28946,#28947,#28948,#28949,#28950,#28951));
#6847=EDGE_LOOP('',(#28952,#28953,#28954,#28955,#28956,#28957));
#6848=EDGE_LOOP('',(#28958,#28959,#28960,#28961,#28962,#28963));
#6849=EDGE_LOOP('',(#28964));
#6850=EDGE_LOOP('',(#28965));
#6851=EDGE_LOOP('',(#28966,#28967,#28968,#28969,#28970,#28971));
#6852=EDGE_LOOP('',(#28972,#28973,#28974,#28975,#28976,#28977));
#6853=EDGE_LOOP('',(#28978,#28979,#28980,#28981,#28982,#28983));
#6854=EDGE_LOOP('',(#28984));
#6855=EDGE_LOOP('',(#28985));
#6856=EDGE_LOOP('',(#28986,#28987,#28988,#28989,#28990,#28991));
#6857=EDGE_LOOP('',(#28992,#28993,#28994,#28995,#28996,#28997));
#6858=EDGE_LOOP('',(#28998,#28999,#29000,#29001,#29002,#29003));
#6859=EDGE_LOOP('',(#29004));
#6860=EDGE_LOOP('',(#29005));
#6861=EDGE_LOOP('',(#29006,#29007,#29008,#29009,#29010,#29011));
#6862=EDGE_LOOP('',(#29012,#29013,#29014,#29015,#29016,#29017));
#6863=EDGE_LOOP('',(#29018,#29019,#29020,#29021,#29022,#29023));
#6864=EDGE_LOOP('',(#29024));
#6865=EDGE_LOOP('',(#29025));
#6866=EDGE_LOOP('',(#29026,#29027,#29028,#29029,#29030,#29031));
#6867=EDGE_LOOP('',(#29032,#29033,#29034,#29035,#29036,#29037));
#6868=EDGE_LOOP('',(#29038,#29039,#29040,#29041,#29042,#29043));
#6869=EDGE_LOOP('',(#29044));
#6870=EDGE_LOOP('',(#29045));
#6871=EDGE_LOOP('',(#29046,#29047,#29048,#29049,#29050,#29051));
#6872=EDGE_LOOP('',(#29052,#29053,#29054,#29055,#29056,#29057));
#6873=EDGE_LOOP('',(#29058,#29059,#29060,#29061,#29062,#29063));
#6874=EDGE_LOOP('',(#29064));
#6875=EDGE_LOOP('',(#29065));
#6876=EDGE_LOOP('',(#29066,#29067,#29068,#29069));
#6877=EDGE_LOOP('',(#29070,#29071,#29072,#29073,#29074,#29075,#29076,#29077,
#29078,#29079,#29080,#29081));
#6878=EDGE_LOOP('',(#29082,#29083,#29084,#29085));
#6879=EDGE_LOOP('',(#29086,#29087,#29088,#29089));
#6880=EDGE_LOOP('',(#29090,#29091,#29092,#29093));
#6881=EDGE_LOOP('',(#29094,#29095,#29096,#29097));
#6882=EDGE_LOOP('',(#29098,#29099,#29100,#29101));
#6883=EDGE_LOOP('',(#29102,#29103,#29104,#29105));
#6884=EDGE_LOOP('',(#29106,#29107,#29108,#29109));
#6885=EDGE_LOOP('',(#29110,#29111,#29112,#29113));
#6886=EDGE_LOOP('',(#29114,#29115,#29116,#29117));
#6887=EDGE_LOOP('',(#29118,#29119,#29120,#29121));
#6888=EDGE_LOOP('',(#29122,#29123,#29124,#29125));
#6889=EDGE_LOOP('',(#29126,#29127,#29128,#29129));
#6890=EDGE_LOOP('',(#29130,#29131,#29132,#29133));
#6891=EDGE_LOOP('',(#29134,#29135,#29136,#29137));
#6892=EDGE_LOOP('',(#29138,#29139,#29140,#29141));
#6893=EDGE_LOOP('',(#29142,#29143,#29144,#29145));
#6894=EDGE_LOOP('',(#29146,#29147,#29148,#29149));
#6895=EDGE_LOOP('',(#29150,#29151,#29152,#29153));
#6896=EDGE_LOOP('',(#29154,#29155,#29156,#29157));
#6897=EDGE_LOOP('',(#29158,#29159,#29160,#29161));
#6898=EDGE_LOOP('',(#29162,#29163,#29164,#29165));
#6899=EDGE_LOOP('',(#29166,#29167,#29168,#29169));
#6900=EDGE_LOOP('',(#29170));
#6901=EDGE_LOOP('',(#29171));
#6902=EDGE_LOOP('',(#29172,#29173,#29174,#29175));
#6903=EDGE_LOOP('',(#29176,#29177,#29178,#29179));
#6904=EDGE_LOOP('',(#29180,#29181,#29182,#29183));
#6905=EDGE_LOOP('',(#29184));
#6906=EDGE_LOOP('',(#29185));
#6907=EDGE_LOOP('',(#29186,#29187,#29188,#29189));
#6908=EDGE_LOOP('',(#29190,#29191,#29192,#29193));
#6909=EDGE_LOOP('',(#29194,#29195,#29196,#29197));
#6910=EDGE_LOOP('',(#29198));
#6911=EDGE_LOOP('',(#29199));
#6912=EDGE_LOOP('',(#29200,#29201,#29202,#29203));
#6913=EDGE_LOOP('',(#29204,#29205,#29206,#29207));
#6914=EDGE_LOOP('',(#29208,#29209,#29210,#29211));
#6915=EDGE_LOOP('',(#29212));
#6916=EDGE_LOOP('',(#29213));
#6917=EDGE_LOOP('',(#29214,#29215,#29216,#29217,#29218));
#6918=EDGE_LOOP('',(#29219));
#6919=EDGE_LOOP('',(#29220));
#6920=EDGE_LOOP('',(#29221,#29222,#29223,#29224,#29225));
#6921=EDGE_LOOP('',(#29226,#29227,#29228,#29229,#29230));
#6922=EDGE_LOOP('',(#29231,#29232,#29233,#29234,#29235));
#6923=EDGE_LOOP('',(#29236));
#6924=EDGE_LOOP('',(#29237));
#6925=EDGE_LOOP('',(#29238,#29239,#29240,#29241,#29242,#29243));
#6926=EDGE_LOOP('',(#29244,#29245,#29246,#29247,#29248,#29249));
#6927=EDGE_LOOP('',(#29250,#29251,#29252,#29253,#29254,#29255));
#6928=EDGE_LOOP('',(#29256));
#6929=EDGE_LOOP('',(#29257));
#6930=EDGE_LOOP('',(#29258,#29259,#29260,#29261,#29262,#29263));
#6931=EDGE_LOOP('',(#29264,#29265,#29266,#29267,#29268,#29269));
#6932=EDGE_LOOP('',(#29270,#29271,#29272,#29273,#29274,#29275));
#6933=EDGE_LOOP('',(#29276));
#6934=EDGE_LOOP('',(#29277));
#6935=EDGE_LOOP('',(#29278,#29279,#29280,#29281,#29282,#29283));
#6936=EDGE_LOOP('',(#29284,#29285,#29286,#29287,#29288,#29289));
#6937=EDGE_LOOP('',(#29290,#29291,#29292,#29293,#29294,#29295));
#6938=EDGE_LOOP('',(#29296));
#6939=EDGE_LOOP('',(#29297));
#6940=EDGE_LOOP('',(#29298,#29299,#29300,#29301,#29302,#29303));
#6941=EDGE_LOOP('',(#29304,#29305,#29306,#29307,#29308,#29309));
#6942=EDGE_LOOP('',(#29310,#29311,#29312,#29313,#29314,#29315));
#6943=EDGE_LOOP('',(#29316));
#6944=EDGE_LOOP('',(#29317));
#6945=EDGE_LOOP('',(#29318,#29319,#29320,#29321,#29322,#29323));
#6946=EDGE_LOOP('',(#29324,#29325,#29326,#29327,#29328,#29329));
#6947=EDGE_LOOP('',(#29330,#29331,#29332,#29333,#29334,#29335));
#6948=EDGE_LOOP('',(#29336));
#6949=EDGE_LOOP('',(#29337));
#6950=EDGE_LOOP('',(#29338,#29339,#29340,#29341,#29342,#29343));
#6951=EDGE_LOOP('',(#29344,#29345,#29346,#29347,#29348,#29349));
#6952=EDGE_LOOP('',(#29350,#29351,#29352,#29353,#29354,#29355));
#6953=EDGE_LOOP('',(#29356));
#6954=EDGE_LOOP('',(#29357));
#6955=EDGE_LOOP('',(#29358,#29359,#29360,#29361,#29362,#29363));
#6956=EDGE_LOOP('',(#29364,#29365,#29366,#29367,#29368,#29369));
#6957=EDGE_LOOP('',(#29370,#29371,#29372,#29373,#29374,#29375));
#6958=EDGE_LOOP('',(#29376));
#6959=EDGE_LOOP('',(#29377));
#6960=EDGE_LOOP('',(#29378,#29379,#29380,#29381,#29382,#29383));
#6961=EDGE_LOOP('',(#29384,#29385,#29386,#29387,#29388,#29389));
#6962=EDGE_LOOP('',(#29390,#29391,#29392,#29393,#29394,#29395));
#6963=EDGE_LOOP('',(#29396));
#6964=EDGE_LOOP('',(#29397));
#6965=EDGE_LOOP('',(#29398,#29399,#29400,#29401,#29402,#29403));
#6966=EDGE_LOOP('',(#29404,#29405,#29406,#29407,#29408,#29409));
#6967=EDGE_LOOP('',(#29410,#29411,#29412,#29413,#29414,#29415));
#6968=EDGE_LOOP('',(#29416));
#6969=EDGE_LOOP('',(#29417));
#6970=EDGE_LOOP('',(#29418,#29419,#29420,#29421,#29422,#29423,#29424));
#6971=EDGE_LOOP('',(#29425,#29426,#29427,#29428,#29429,#29430));
#6972=EDGE_LOOP('',(#29431,#29432,#29433,#29434,#29435,#29436,#29437));
#6973=EDGE_LOOP('',(#29438));
#6974=EDGE_LOOP('',(#29439));
#6975=EDGE_LOOP('',(#29440,#29441,#29442,#29443,#29444,#29445));
#6976=EDGE_LOOP('',(#29446,#29447,#29448,#29449,#29450,#29451));
#6977=EDGE_LOOP('',(#29452,#29453,#29454,#29455,#29456,#29457));
#6978=EDGE_LOOP('',(#29458));
#6979=EDGE_LOOP('',(#29459));
#6980=EDGE_LOOP('',(#29460,#29461,#29462,#29463,#29464,#29465));
#6981=EDGE_LOOP('',(#29466,#29467,#29468,#29469,#29470,#29471));
#6982=EDGE_LOOP('',(#29472,#29473,#29474,#29475,#29476,#29477));
#6983=EDGE_LOOP('',(#29478));
#6984=EDGE_LOOP('',(#29479));
#6985=EDGE_LOOP('',(#29480,#29481,#29482,#29483,#29484,#29485));
#6986=EDGE_LOOP('',(#29486,#29487,#29488,#29489,#29490,#29491));
#6987=EDGE_LOOP('',(#29492,#29493,#29494,#29495,#29496,#29497));
#6988=EDGE_LOOP('',(#29498));
#6989=EDGE_LOOP('',(#29499));
#6990=EDGE_LOOP('',(#29500,#29501,#29502,#29503,#29504,#29505));
#6991=EDGE_LOOP('',(#29506,#29507,#29508,#29509,#29510,#29511));
#6992=EDGE_LOOP('',(#29512,#29513,#29514,#29515,#29516,#29517));
#6993=EDGE_LOOP('',(#29518));
#6994=EDGE_LOOP('',(#29519));
#6995=EDGE_LOOP('',(#29520,#29521,#29522,#29523,#29524,#29525));
#6996=EDGE_LOOP('',(#29526,#29527,#29528,#29529,#29530,#29531));
#6997=EDGE_LOOP('',(#29532,#29533,#29534,#29535,#29536,#29537));
#6998=EDGE_LOOP('',(#29538));
#6999=EDGE_LOOP('',(#29539));
#7000=EDGE_LOOP('',(#29540,#29541,#29542,#29543,#29544,#29545));
#7001=EDGE_LOOP('',(#29546,#29547,#29548,#29549,#29550,#29551));
#7002=EDGE_LOOP('',(#29552,#29553,#29554,#29555,#29556,#29557));
#7003=EDGE_LOOP('',(#29558));
#7004=EDGE_LOOP('',(#29559));
#7005=EDGE_LOOP('',(#29560,#29561,#29562,#29563,#29564,#29565));
#7006=EDGE_LOOP('',(#29566,#29567,#29568,#29569,#29570,#29571));
#7007=EDGE_LOOP('',(#29572,#29573,#29574,#29575,#29576,#29577));
#7008=EDGE_LOOP('',(#29578));
#7009=EDGE_LOOP('',(#29579));
#7010=EDGE_LOOP('',(#29580,#29581,#29582,#29583,#29584,#29585));
#7011=EDGE_LOOP('',(#29586,#29587,#29588,#29589,#29590,#29591));
#7012=EDGE_LOOP('',(#29592,#29593,#29594,#29595,#29596,#29597));
#7013=EDGE_LOOP('',(#29598));
#7014=EDGE_LOOP('',(#29599));
#7015=EDGE_LOOP('',(#29600,#29601,#29602,#29603,#29604,#29605));
#7016=EDGE_LOOP('',(#29606,#29607,#29608,#29609,#29610,#29611));
#7017=EDGE_LOOP('',(#29612,#29613,#29614,#29615,#29616,#29617));
#7018=EDGE_LOOP('',(#29618));
#7019=EDGE_LOOP('',(#29619));
#7020=EDGE_LOOP('',(#29620,#29621,#29622,#29623,#29624,#29625));
#7021=EDGE_LOOP('',(#29626,#29627,#29628,#29629,#29630,#29631));
#7022=EDGE_LOOP('',(#29632,#29633,#29634,#29635,#29636,#29637));
#7023=EDGE_LOOP('',(#29638));
#7024=EDGE_LOOP('',(#29639));
#7025=EDGE_LOOP('',(#29640,#29641,#29642,#29643));
#7026=EDGE_LOOP('',(#29644,#29645,#29646,#29647,#29648,#29649,#29650,#29651,
#29652,#29653,#29654,#29655));
#7027=EDGE_LOOP('',(#29656,#29657,#29658,#29659));
#7028=EDGE_LOOP('',(#29660,#29661,#29662,#29663));
#7029=EDGE_LOOP('',(#29664,#29665,#29666,#29667));
#7030=EDGE_LOOP('',(#29668,#29669,#29670,#29671));
#7031=EDGE_LOOP('',(#29672,#29673,#29674,#29675));
#7032=EDGE_LOOP('',(#29676,#29677,#29678,#29679));
#7033=EDGE_LOOP('',(#29680,#29681,#29682,#29683));
#7034=EDGE_LOOP('',(#29684,#29685,#29686,#29687));
#7035=EDGE_LOOP('',(#29688,#29689,#29690,#29691));
#7036=EDGE_LOOP('',(#29692,#29693,#29694,#29695));
#7037=EDGE_LOOP('',(#29696,#29697,#29698,#29699));
#7038=EDGE_LOOP('',(#29700,#29701,#29702,#29703));
#7039=EDGE_LOOP('',(#29704,#29705,#29706,#29707));
#7040=EDGE_LOOP('',(#29708,#29709,#29710,#29711));
#7041=EDGE_LOOP('',(#29712,#29713,#29714,#29715));
#7042=EDGE_LOOP('',(#29716,#29717,#29718,#29719));
#7043=EDGE_LOOP('',(#29720,#29721,#29722,#29723));
#7044=EDGE_LOOP('',(#29724,#29725,#29726,#29727));
#7045=EDGE_LOOP('',(#29728,#29729,#29730,#29731));
#7046=EDGE_LOOP('',(#29732,#29733,#29734,#29735));
#7047=EDGE_LOOP('',(#29736));
#7048=EDGE_LOOP('',(#29737));
#7049=EDGE_LOOP('',(#29738,#29739,#29740,#29741));
#7050=EDGE_LOOP('',(#29742,#29743,#29744,#29745));
#7051=EDGE_LOOP('',(#29746,#29747,#29748,#29749));
#7052=EDGE_LOOP('',(#29750));
#7053=EDGE_LOOP('',(#29751));
#7054=EDGE_LOOP('',(#29752,#29753,#29754,#29755));
#7055=EDGE_LOOP('',(#29756,#29757,#29758,#29759,#29760,#29761));
#7056=EDGE_LOOP('',(#29762,#29763,#29764,#29765));
#7057=EDGE_LOOP('',(#29766,#29767,#29768,#29769));
#7058=EDGE_LOOP('',(#29770,#29771,#29772,#29773,#29774,#29775));
#7059=EDGE_LOOP('',(#29776));
#7060=EDGE_LOOP('',(#29777,#29778,#29779,#29780));
#7061=EDGE_LOOP('',(#29781,#29782,#29783,#29784));
#7062=EDGE_LOOP('',(#29785));
#7063=EDGE_LOOP('',(#29786,#29787,#29788,#29789));
#7064=EDGE_LOOP('',(#29790,#29791,#29792,#29793));
#7065=EDGE_LOOP('',(#29794,#29795,#29796,#29797));
#7066=EDGE_LOOP('',(#29798,#29799,#29800,#29801));
#7067=EDGE_LOOP('',(#29802,#29803,#29804,#29805,#29806));
#7068=EDGE_LOOP('',(#29807,#29808,#29809,#29810));
#7069=EDGE_LOOP('',(#29811,#29812,#29813,#29814,#29815,#29816,#29817,#29818));
#7070=EDGE_LOOP('',(#29819,#29820,#29821,#29822,#29823,#29824,#29825));
#7071=EDGE_LOOP('',(#29826,#29827,#29828,#29829));
#7072=EDGE_LOOP('',(#29830,#29831,#29832,#29833));
#7073=EDGE_LOOP('',(#29834,#29835,#29836,#29837,#29838,#29839));
#7074=EDGE_LOOP('',(#29840,#29841,#29842,#29843,#29844,#29845,#29846));
#7075=EDGE_LOOP('',(#29847,#29848,#29849,#29850,#29851));
#7076=EDGE_LOOP('',(#29852,#29853,#29854,#29855,#29856,#29857));
#7077=EDGE_LOOP('',(#29858,#29859,#29860,#29861,#29862));
#7078=EDGE_LOOP('',(#29863,#29864,#29865,#29866,#29867,#29868));
#7079=EDGE_LOOP('',(#29869,#29870,#29871,#29872,#29873));
#7080=EDGE_LOOP('',(#29874,#29875,#29876,#29877,#29878,#29879,#29880,#29881));
#7081=EDGE_LOOP('',(#29882,#29883,#29884,#29885,#29886,#29887));
#7082=EDGE_LOOP('',(#29888,#29889,#29890,#29891,#29892,#29893));
#7083=EDGE_LOOP('',(#29894,#29895,#29896,#29897,#29898));
#7084=EDGE_LOOP('',(#29899,#29900,#29901,#29902,#29903,#29904));
#7085=EDGE_LOOP('',(#29905,#29906,#29907,#29908));
#7086=EDGE_LOOP('',(#29909,#29910,#29911,#29912,#29913,#29914,#29915,#29916));
#7087=EDGE_LOOP('',(#29917,#29918,#29919,#29920));
#7088=EDGE_LOOP('',(#29921,#29922,#29923,#29924,#29925));
#7089=EDGE_LOOP('',(#29926,#29927,#29928,#29929,#29930,#29931,#29932,#29933));
#7090=EDGE_LOOP('',(#29934,#29935,#29936,#29937,#29938,#29939,#29940,#29941,
#29942,#29943,#29944,#29945,#29946,#29947,#29948,#29949));
#7091=EDGE_LOOP('',(#29950,#29951,#29952,#29953,#29954));
#7092=EDGE_LOOP('',(#29955,#29956,#29957,#29958));
#7093=EDGE_LOOP('',(#29959,#29960,#29961,#29962,#29963,#29964,#29965,#29966));
#7094=EDGE_LOOP('',(#29967,#29968,#29969,#29970,#29971,#29972,#29973));
#7095=EDGE_LOOP('',(#29974,#29975,#29976,#29977));
#7096=EDGE_LOOP('',(#29978,#29979,#29980));
#7097=EDGE_LOOP('',(#29981,#29982,#29983,#29984,#29985));
#7098=EDGE_LOOP('',(#29986,#29987,#29988,#29989));
#7099=EDGE_LOOP('',(#29990,#29991,#29992,#29993,#29994));
#7100=EDGE_LOOP('',(#29995,#29996,#29997,#29998));
#7101=EDGE_LOOP('',(#29999,#30000,#30001,#30002,#30003,#30004,#30005,#30006));
#7102=EDGE_LOOP('',(#30007,#30008,#30009,#30010,#30011));
#7103=EDGE_LOOP('',(#30012,#30013,#30014,#30015));
#7104=EDGE_LOOP('',(#30016,#30017,#30018,#30019,#30020,#30021));
#7105=EDGE_LOOP('',(#30022,#30023,#30024,#30025,#30026,#30027,#30028));
#7106=EDGE_LOOP('',(#30029,#30030,#30031,#30032,#30033));
#7107=EDGE_LOOP('',(#30034,#30035,#30036,#30037,#30038,#30039));
#7108=EDGE_LOOP('',(#30040,#30041,#30042,#30043,#30044));
#7109=EDGE_LOOP('',(#30045,#30046,#30047,#30048,#30049,#30050));
#7110=EDGE_LOOP('',(#30051,#30052,#30053,#30054,#30055,#30056));
#7111=EDGE_LOOP('',(#30057,#30058,#30059,#30060,#30061));
#7112=EDGE_LOOP('',(#30062,#30063,#30064,#30065));
#7113=EDGE_LOOP('',(#30066,#30067,#30068,#30069,#30070,#30071,#30072,#30073));
#7114=EDGE_LOOP('',(#30074,#30075,#30076,#30077,#30078,#30079,#30080));
#7115=EDGE_LOOP('',(#30081,#30082,#30083,#30084,#30085));
#7116=EDGE_LOOP('',(#30086,#30087,#30088,#30089,#30090,#30091,#30092,#30093));
#7117=EDGE_LOOP('',(#30094,#30095,#30096,#30097,#30098,#30099));
#7118=EDGE_LOOP('',(#30100,#30101,#30102,#30103));
#7119=EDGE_LOOP('',(#30104,#30105,#30106,#30107,#30108,#30109,#30110));
#7120=EDGE_LOOP('',(#30111,#30112,#30113,#30114));
#7121=EDGE_LOOP('',(#30115,#30116,#30117,#30118,#30119,#30120,#30121));
#7122=EDGE_LOOP('',(#30122,#30123,#30124,#30125,#30126));
#7123=EDGE_LOOP('',(#30127,#30128,#30129,#30130,#30131));
#7124=EDGE_LOOP('',(#30132,#30133,#30134,#30135));
#7125=EDGE_LOOP('',(#30136,#30137,#30138));
#7126=EDGE_LOOP('',(#30139,#30140,#30141,#30142));
#7127=EDGE_LOOP('',(#30143,#30144,#30145,#30146));
#7128=EDGE_LOOP('',(#30147,#30148,#30149,#30150,#30151));
#7129=EDGE_LOOP('',(#30152,#30153,#30154,#30155,#30156));
#7130=EDGE_LOOP('',(#30157,#30158,#30159,#30160,#30161));
#7131=EDGE_LOOP('',(#30162,#30163,#30164,#30165,#30166));
#7132=EDGE_LOOP('',(#30167,#30168,#30169,#30170,#30171));
#7133=EDGE_LOOP('',(#30172,#30173,#30174,#30175,#30176));
#7134=EDGE_LOOP('',(#30177,#30178,#30179,#30180,#30181,#30182));
#7135=EDGE_LOOP('',(#30183,#30184,#30185,#30186,#30187,#30188));
#7136=EDGE_LOOP('',(#30189,#30190,#30191,#30192,#30193));
#7137=EDGE_LOOP('',(#30194,#30195,#30196,#30197,#30198,#30199));
#7138=EDGE_LOOP('',(#30200,#30201,#30202,#30203,#30204,#30205));
#7139=EDGE_LOOP('',(#30206,#30207,#30208,#30209,#30210));
#7140=EDGE_LOOP('',(#30211,#30212,#30213,#30214,#30215,#30216,#30217,#30218,
#30219,#30220,#30221,#30222,#30223,#30224,#30225,#30226,#30227,#30228,#30229,
#30230,#30231,#30232,#30233,#30234,#30235,#30236,#30237,#30238,#30239));
#7141=EDGE_LOOP('',(#30240,#30241,#30242,#30243,#30244));
#7142=EDGE_LOOP('',(#30245,#30246,#30247,#30248,#30249));
#7143=EDGE_LOOP('',(#30250,#30251,#30252,#30253));
#7144=EDGE_LOOP('',(#30254,#30255,#30256,#30257,#30258));
#7145=EDGE_LOOP('',(#30259,#30260,#30261,#30262,#30263,#30264,#30265,#30266));
#7146=EDGE_LOOP('',(#30267,#30268,#30269,#30270,#30271,#30272,#30273,#30274));
#7147=EDGE_LOOP('',(#30275,#30276,#30277));
#7148=EDGE_LOOP('',(#30278,#30279,#30280));
#7149=EDGE_LOOP('',(#30281,#30282,#30283,#30284));
#7150=EDGE_LOOP('',(#30285,#30286,#30287));
#7151=EDGE_LOOP('',(#30288,#30289,#30290,#30291));
#7152=EDGE_LOOP('',(#30292,#30293,#30294,#30295));
#7153=EDGE_LOOP('',(#30296,#30297,#30298,#30299,#30300,#30301));
#7154=EDGE_LOOP('',(#30302,#30303,#30304,#30305));
#7155=EDGE_LOOP('',(#30306,#30307,#30308,#30309));
#7156=EDGE_LOOP('',(#30310,#30311,#30312,#30313));
#7157=EDGE_LOOP('',(#30314,#30315,#30316,#30317));
#7158=EDGE_LOOP('',(#30318,#30319,#30320,#30321,#30322,#30323,#30324));
#7159=EDGE_LOOP('',(#30325,#30326,#30327,#30328,#30329,#30330,#30331));
#7160=EDGE_LOOP('',(#30332,#30333,#30334,#30335,#30336));
#7161=EDGE_LOOP('',(#30337,#30338,#30339,#30340));
#7162=EDGE_LOOP('',(#30341,#30342,#30343));
#7163=EDGE_LOOP('',(#30344,#30345,#30346,#30347,#30348));
#7164=EDGE_LOOP('',(#30349,#30350,#30351,#30352));
#7165=EDGE_LOOP('',(#30353,#30354,#30355,#30356,#30357));
#7166=EDGE_LOOP('',(#30358,#30359,#30360,#30361));
#7167=EDGE_LOOP('',(#30362,#30363,#30364,#30365,#30366,#30367,#30368,#30369));
#7168=EDGE_LOOP('',(#30370,#30371,#30372,#30373,#30374));
#7169=EDGE_LOOP('',(#30375,#30376,#30377,#30378,#30379,#30380,#30381));
#7170=EDGE_LOOP('',(#30382,#30383,#30384,#30385,#30386,#30387,#30388));
#7171=EDGE_LOOP('',(#30389,#30390,#30391,#30392,#30393));
#7172=EDGE_LOOP('',(#30394,#30395,#30396,#30397));
#7173=EDGE_LOOP('',(#30398,#30399,#30400,#30401));
#7174=EDGE_LOOP('',(#30402,#30403,#30404,#30405,#30406,#30407,#30408));
#7175=EDGE_LOOP('',(#30409,#30410,#30411,#30412,#30413));
#7176=EDGE_LOOP('',(#30414,#30415,#30416,#30417,#30418,#30419,#30420));
#7177=EDGE_LOOP('',(#30421,#30422,#30423,#30424,#30425,#30426,#30427,#30428,
#30429));
#7178=EDGE_LOOP('',(#30430));
#7179=EDGE_LOOP('',(#30431));
#7180=EDGE_LOOP('',(#30432,#30433,#30434,#30435,#30436));
#7181=EDGE_LOOP('',(#30437,#30438,#30439,#30440,#30441,#30442,#30443,#30444,
#30445,#30446,#30447,#30448,#30449,#30450));
#7182=EDGE_LOOP('',(#30451,#30452,#30453,#30454,#30455));
#7183=EDGE_LOOP('',(#30456,#30457,#30458,#30459,#30460,#30461));
#7184=EDGE_LOOP('',(#30462,#30463,#30464,#30465,#30466,#30467));
#7185=EDGE_LOOP('',(#30468,#30469,#30470,#30471));
#7186=EDGE_LOOP('',(#30472,#30473,#30474,#30475,#30476));
#7187=EDGE_LOOP('',(#30477,#30478,#30479,#30480));
#7188=EDGE_LOOP('',(#30481,#30482,#30483,#30484,#30485,#30486));
#7189=EDGE_LOOP('',(#30487,#30488,#30489,#30490,#30491));
#7190=EDGE_LOOP('',(#30492,#30493,#30494,#30495,#30496));
#7191=EDGE_LOOP('',(#30497,#30498));
#7192=EDGE_LOOP('',(#30499,#30500,#30501,#30502,#30503,#30504));
#7193=EDGE_LOOP('',(#30505,#30506));
#7194=EDGE_LOOP('',(#30507,#30508,#30509,#30510,#30511,#30512,#30513,#30514,
#30515));
#7195=EDGE_LOOP('',(#30516,#30517,#30518,#30519));
#7196=EDGE_LOOP('',(#30520,#30521,#30522,#30523));
#7197=EDGE_LOOP('',(#30524,#30525));
#7198=EDGE_LOOP('',(#30526,#30527,#30528,#30529,#30530,#30531));
#7199=EDGE_LOOP('',(#30532,#30533,#30534,#30535,#30536,#30537));
#7200=EDGE_LOOP('',(#30538,#30539,#30540,#30541,#30542));
#7201=EDGE_LOOP('',(#30543,#30544,#30545,#30546,#30547,#30548));
#7202=EDGE_LOOP('',(#30549,#30550,#30551,#30552,#30553,#30554));
#7203=EDGE_LOOP('',(#30555,#30556,#30557,#30558,#30559,#30560));
#7204=EDGE_LOOP('',(#30561,#30562,#30563,#30564,#30565,#30566));
#7205=EDGE_LOOP('',(#30567,#30568,#30569,#30570,#30571,#30572));
#7206=EDGE_LOOP('',(#30573,#30574,#30575,#30576,#30577));
#7207=EDGE_LOOP('',(#30578));
#7208=EDGE_LOOP('',(#30579));
#7209=EDGE_LOOP('',(#30580,#30581,#30582,#30583));
#7210=EDGE_LOOP('',(#30584,#30585,#30586,#30587));
#7211=EDGE_LOOP('',(#30588));
#7212=EDGE_LOOP('',(#30589));
#7213=EDGE_LOOP('',(#30590,#30591,#30592,#30593));
#7214=EDGE_LOOP('',(#30594,#30595,#30596,#30597));
#7215=EDGE_LOOP('',(#30598));
#7216=EDGE_LOOP('',(#30599));
#7217=EDGE_LOOP('',(#30600,#30601,#30602,#30603));
#7218=EDGE_LOOP('',(#30604,#30605,#30606,#30607));
#7219=EDGE_LOOP('',(#30608,#30609,#30610,#30611));
#7220=EDGE_LOOP('',(#30612,#30613,#30614,#30615));
#7221=EDGE_LOOP('',(#30616,#30617,#30618,#30619));
#7222=EDGE_LOOP('',(#30620,#30621,#30622,#30623));
#7223=EDGE_LOOP('',(#30624,#30625,#30626,#30627));
#7224=EDGE_LOOP('',(#30628,#30629,#30630,#30631));
#7225=EDGE_LOOP('',(#30632,#30633,#30634,#30635));
#7226=EDGE_LOOP('',(#30636,#30637,#30638,#30639));
#7227=EDGE_LOOP('',(#30640,#30641,#30642,#30643));
#7228=EDGE_LOOP('',(#30644,#30645,#30646,#30647));
#7229=EDGE_LOOP('',(#30648,#30649,#30650,#30651));
#7230=EDGE_LOOP('',(#30652,#30653,#30654,#30655));
#7231=EDGE_LOOP('',(#30656,#30657,#30658,#30659));
#7232=EDGE_LOOP('',(#30660,#30661,#30662,#30663));
#7233=EDGE_LOOP('',(#30664,#30665,#30666,#30667));
#7234=EDGE_LOOP('',(#30668,#30669,#30670,#30671));
#7235=EDGE_LOOP('',(#30672,#30673,#30674,#30675));
#7236=EDGE_LOOP('',(#30676,#30677,#30678,#30679));
#7237=EDGE_LOOP('',(#30680,#30681,#30682,#30683));
#7238=EDGE_LOOP('',(#30684,#30685,#30686,#30687));
#7239=EDGE_LOOP('',(#30688,#30689,#30690,#30691));
#7240=EDGE_LOOP('',(#30692,#30693,#30694,#30695));
#7241=EDGE_LOOP('',(#30696,#30697,#30698,#30699));
#7242=EDGE_LOOP('',(#30700,#30701,#30702,#30703));
#7243=EDGE_LOOP('',(#30704,#30705,#30706,#30707));
#7244=EDGE_LOOP('',(#30708,#30709,#30710,#30711));
#7245=EDGE_LOOP('',(#30712,#30713,#30714,#30715));
#7246=EDGE_LOOP('',(#30716,#30717,#30718,#30719));
#7247=EDGE_LOOP('',(#30720,#30721,#30722,#30723));
#7248=EDGE_LOOP('',(#30724,#30725,#30726,#30727));
#7249=EDGE_LOOP('',(#30728,#30729,#30730,#30731));
#7250=EDGE_LOOP('',(#30732,#30733,#30734,#30735));
#7251=EDGE_LOOP('',(#30736,#30737,#30738,#30739));
#7252=EDGE_LOOP('',(#30740,#30741,#30742));
#7253=EDGE_LOOP('',(#30743,#30744,#30745,#30746,#30747));
#7254=EDGE_LOOP('',(#30748,#30749,#30750,#30751));
#7255=EDGE_LOOP('',(#30752,#30753,#30754,#30755));
#7256=EDGE_LOOP('',(#30756,#30757,#30758,#30759));
#7257=EDGE_LOOP('',(#30760,#30761,#30762,#30763));
#7258=EDGE_LOOP('',(#30764,#30765,#30766,#30767));
#7259=EDGE_LOOP('',(#30768,#30769,#30770,#30771));
#7260=EDGE_LOOP('',(#30772,#30773,#30774,#30775));
#7261=EDGE_LOOP('',(#30776,#30777,#30778,#30779));
#7262=EDGE_LOOP('',(#30780,#30781,#30782,#30783));
#7263=EDGE_LOOP('',(#30784,#30785,#30786,#30787));
#7264=EDGE_LOOP('',(#30788,#30789,#30790,#30791));
#7265=EDGE_LOOP('',(#30792,#30793,#30794,#30795));
#7266=EDGE_LOOP('',(#30796,#30797,#30798,#30799));
#7267=EDGE_LOOP('',(#30800,#30801,#30802,#30803));
#7268=EDGE_LOOP('',(#30804,#30805,#30806,#30807));
#7269=EDGE_LOOP('',(#30808,#30809,#30810,#30811));
#7270=EDGE_LOOP('',(#30812,#30813,#30814,#30815));
#7271=EDGE_LOOP('',(#30816,#30817,#30818,#30819));
#7272=EDGE_LOOP('',(#30820,#30821,#30822,#30823));
#7273=EDGE_LOOP('',(#30824,#30825,#30826,#30827));
#7274=EDGE_LOOP('',(#30828,#30829,#30830,#30831));
#7275=EDGE_LOOP('',(#30832,#30833,#30834,#30835));
#7276=EDGE_LOOP('',(#30836,#30837,#30838,#30839));
#7277=EDGE_LOOP('',(#30840,#30841,#30842,#30843));
#7278=EDGE_LOOP('',(#30844,#30845,#30846,#30847));
#7279=EDGE_LOOP('',(#30848,#30849,#30850,#30851));
#7280=EDGE_LOOP('',(#30852,#30853,#30854,#30855));
#7281=EDGE_LOOP('',(#30856,#30857,#30858,#30859,#30860));
#7282=EDGE_LOOP('',(#30861,#30862,#30863,#30864,#30865,#30866,#30867));
#7283=EDGE_LOOP('',(#30868));
#7284=EDGE_LOOP('',(#30869,#30870,#30871,#30872,#30873,#30874));
#7285=EDGE_LOOP('',(#30875,#30876));
#7286=EDGE_LOOP('',(#30877));
#7287=EDGE_LOOP('',(#30878,#30879,#30880,#30881,#30882,#30883));
#7288=EDGE_LOOP('',(#30884,#30885,#30886,#30887));
#7289=EDGE_LOOP('',(#30888,#30889,#30890,#30891,#30892,#30893));
#7290=EDGE_LOOP('',(#30894,#30895,#30896,#30897,#30898,#30899));
#7291=EDGE_LOOP('',(#30900,#30901,#30902,#30903));
#7292=EDGE_LOOP('',(#30904,#30905));
#7293=EDGE_LOOP('',(#30906,#30907,#30908,#30909,#30910,#30911));
#7294=EDGE_LOOP('',(#30912,#30913,#30914,#30915,#30916,#30917));
#7295=EDGE_LOOP('',(#30918,#30919,#30920,#30921,#30922,#30923));
#7296=EDGE_LOOP('',(#30924,#30925,#30926,#30927,#30928,#30929,#30930,#30931,
#30932,#30933,#30934,#30935,#30936,#30937,#30938,#30939,#30940,#30941,#30942,
#30943,#30944,#30945,#30946,#30947,#30948,#30949,#30950,#30951,#30952,#30953,
#30954,#30955,#30956,#30957,#30958,#30959,#30960,#30961,#30962,#30963,#30964,
#30965,#30966,#30967,#30968,#30969,#30970,#30971,#30972,#30973,#30974,#30975,
#30976,#30977,#30978,#30979,#30980,#30981,#30982,#30983,#30984));
#7297=EDGE_LOOP('',(#30985,#30986,#30987,#30988,#30989));
#7298=EDGE_LOOP('',(#30990,#30991,#30992,#30993));
#7299=EDGE_LOOP('',(#30994,#30995,#30996,#30997,#30998,#30999,#31000,#31001,
#31002,#31003,#31004,#31005,#31006,#31007,#31008,#31009,#31010,#31011,#31012,
#31013,#31014,#31015,#31016,#31017,#31018,#31019,#31020,#31021,#31022,#31023,
#31024,#31025,#31026,#31027,#31028,#31029,#31030,#31031,#31032,#31033,#31034,
#31035,#31036,#31037,#31038,#31039,#31040,#31041,#31042,#31043,#31044,#31045,
#31046,#31047,#31048,#31049,#31050,#31051,#31052,#31053,#31054,#31055));
#7300=EDGE_LOOP('',(#31056,#31057,#31058,#31059));
#7301=EDGE_LOOP('',(#31060,#31061,#31062,#31063));
#7302=EDGE_LOOP('',(#31064,#31065,#31066));
#7303=EDGE_LOOP('',(#31067,#31068,#31069,#31070));
#7304=EDGE_LOOP('',(#31071,#31072,#31073));
#7305=EDGE_LOOP('',(#31074,#31075,#31076,#31077));
#7306=EDGE_LOOP('',(#31078,#31079,#31080));
#7307=EDGE_LOOP('',(#31081,#31082,#31083,#31084));
#7308=EDGE_LOOP('',(#31085,#31086,#31087));
#7309=EDGE_LOOP('',(#31088,#31089,#31090,#31091));
#7310=EDGE_LOOP('',(#31092,#31093,#31094));
#7311=EDGE_LOOP('',(#31095,#31096,#31097,#31098));
#7312=EDGE_LOOP('',(#31099,#31100,#31101));
#7313=EDGE_LOOP('',(#31102,#31103,#31104,#31105));
#7314=EDGE_LOOP('',(#31106,#31107,#31108));
#7315=EDGE_LOOP('',(#31109,#31110,#31111,#31112));
#7316=EDGE_LOOP('',(#31113,#31114,#31115));
#7317=EDGE_LOOP('',(#31116,#31117,#31118,#31119));
#7318=EDGE_LOOP('',(#31120,#31121,#31122));
#7319=EDGE_LOOP('',(#31123,#31124,#31125,#31126));
#7320=EDGE_LOOP('',(#31127,#31128,#31129));
#7321=EDGE_LOOP('',(#31130,#31131,#31132,#31133));
#7322=EDGE_LOOP('',(#31134,#31135,#31136));
#7323=EDGE_LOOP('',(#31137,#31138,#31139,#31140));
#7324=EDGE_LOOP('',(#31141,#31142,#31143));
#7325=EDGE_LOOP('',(#31144,#31145,#31146,#31147));
#7326=EDGE_LOOP('',(#31148,#31149,#31150));
#7327=EDGE_LOOP('',(#31151,#31152,#31153,#31154));
#7328=EDGE_LOOP('',(#31155,#31156,#31157));
#7329=EDGE_LOOP('',(#31158,#31159,#31160,#31161));
#7330=EDGE_LOOP('',(#31162,#31163,#31164));
#7331=EDGE_LOOP('',(#31165,#31166,#31167,#31168));
#7332=EDGE_LOOP('',(#31169,#31170,#31171));
#7333=EDGE_LOOP('',(#31172,#31173,#31174,#31175));
#7334=EDGE_LOOP('',(#31176,#31177,#31178));
#7335=EDGE_LOOP('',(#31179,#31180,#31181,#31182));
#7336=EDGE_LOOP('',(#31183,#31184,#31185));
#7337=EDGE_LOOP('',(#31186,#31187,#31188,#31189));
#7338=EDGE_LOOP('',(#31190,#31191,#31192));
#7339=EDGE_LOOP('',(#31193,#31194,#31195,#31196));
#7340=EDGE_LOOP('',(#31197,#31198,#31199));
#7341=EDGE_LOOP('',(#31200,#31201,#31202,#31203));
#7342=EDGE_LOOP('',(#31204,#31205,#31206));
#7343=EDGE_LOOP('',(#31207,#31208,#31209,#31210));
#7344=EDGE_LOOP('',(#31211,#31212,#31213));
#7345=EDGE_LOOP('',(#31214,#31215,#31216,#31217));
#7346=EDGE_LOOP('',(#31218,#31219,#31220));
#7347=EDGE_LOOP('',(#31221,#31222,#31223,#31224));
#7348=EDGE_LOOP('',(#31225,#31226,#31227));
#7349=EDGE_LOOP('',(#31228,#31229,#31230,#31231));
#7350=EDGE_LOOP('',(#31232,#31233,#31234));
#7351=EDGE_LOOP('',(#31235,#31236,#31237,#31238));
#7352=EDGE_LOOP('',(#31239,#31240,#31241));
#7353=EDGE_LOOP('',(#31242,#31243,#31244,#31245));
#7354=EDGE_LOOP('',(#31246,#31247,#31248));
#7355=EDGE_LOOP('',(#31249,#31250,#31251,#31252));
#7356=EDGE_LOOP('',(#31253,#31254,#31255));
#7357=EDGE_LOOP('',(#31256,#31257,#31258,#31259));
#7358=EDGE_LOOP('',(#31260,#31261,#31262));
#7359=EDGE_LOOP('',(#31263,#31264,#31265,#31266));
#7360=EDGE_LOOP('',(#31267,#31268,#31269));
#7361=EDGE_LOOP('',(#31270,#31271,#31272,#31273));
#7362=EDGE_LOOP('',(#31274,#31275,#31276));
#7363=EDGE_LOOP('',(#31277,#31278,#31279,#31280));
#7364=EDGE_LOOP('',(#31281,#31282,#31283));
#7365=EDGE_LOOP('',(#31284,#31285,#31286,#31287));
#7366=EDGE_LOOP('',(#31288,#31289,#31290));
#7367=EDGE_LOOP('',(#31291,#31292,#31293,#31294));
#7368=EDGE_LOOP('',(#31295,#31296,#31297));
#7369=EDGE_LOOP('',(#31298,#31299,#31300,#31301));
#7370=EDGE_LOOP('',(#31302,#31303,#31304,#31305));
#7371=EDGE_LOOP('',(#31306,#31307,#31308,#31309));
#7372=EDGE_LOOP('',(#31310,#31311,#31312,#31313));
#7373=EDGE_LOOP('',(#31314,#31315,#31316,#31317));
#7374=EDGE_LOOP('',(#31318,#31319,#31320));
#7375=EDGE_LOOP('',(#31321,#31322,#31323,#31324));
#7376=EDGE_LOOP('',(#31325,#31326,#31327));
#7377=EDGE_LOOP('',(#31328,#31329,#31330,#31331));
#7378=EDGE_LOOP('',(#31332,#31333,#31334));
#7379=EDGE_LOOP('',(#31335,#31336,#31337,#31338));
#7380=EDGE_LOOP('',(#31339,#31340,#31341));
#7381=EDGE_LOOP('',(#31342,#31343,#31344,#31345));
#7382=EDGE_LOOP('',(#31346,#31347,#31348));
#7383=EDGE_LOOP('',(#31349,#31350,#31351,#31352));
#7384=EDGE_LOOP('',(#31353,#31354,#31355));
#7385=EDGE_LOOP('',(#31356,#31357,#31358,#31359));
#7386=EDGE_LOOP('',(#31360,#31361,#31362));
#7387=EDGE_LOOP('',(#31363,#31364,#31365,#31366));
#7388=EDGE_LOOP('',(#31367,#31368,#31369));
#7389=EDGE_LOOP('',(#31370,#31371,#31372,#31373));
#7390=EDGE_LOOP('',(#31374,#31375,#31376));
#7391=EDGE_LOOP('',(#31377,#31378,#31379,#31380));
#7392=EDGE_LOOP('',(#31381,#31382,#31383));
#7393=EDGE_LOOP('',(#31384,#31385,#31386,#31387));
#7394=EDGE_LOOP('',(#31388,#31389,#31390));
#7395=EDGE_LOOP('',(#31391,#31392,#31393,#31394));
#7396=EDGE_LOOP('',(#31395,#31396,#31397));
#7397=EDGE_LOOP('',(#31398,#31399,#31400,#31401));
#7398=EDGE_LOOP('',(#31402,#31403,#31404));
#7399=EDGE_LOOP('',(#31405,#31406,#31407,#31408));
#7400=EDGE_LOOP('',(#31409,#31410,#31411));
#7401=EDGE_LOOP('',(#31412,#31413,#31414,#31415));
#7402=EDGE_LOOP('',(#31416,#31417,#31418));
#7403=EDGE_LOOP('',(#31419,#31420,#31421,#31422));
#7404=EDGE_LOOP('',(#31423,#31424,#31425));
#7405=EDGE_LOOP('',(#31426,#31427,#31428,#31429));
#7406=EDGE_LOOP('',(#31430,#31431,#31432));
#7407=EDGE_LOOP('',(#31433,#31434,#31435,#31436));
#7408=EDGE_LOOP('',(#31437,#31438,#31439));
#7409=EDGE_LOOP('',(#31440,#31441,#31442,#31443));
#7410=EDGE_LOOP('',(#31444,#31445,#31446));
#7411=EDGE_LOOP('',(#31447,#31448,#31449,#31450));
#7412=EDGE_LOOP('',(#31451,#31452,#31453));
#7413=EDGE_LOOP('',(#31454,#31455,#31456,#31457));
#7414=EDGE_LOOP('',(#31458,#31459,#31460));
#7415=EDGE_LOOP('',(#31461,#31462,#31463,#31464));
#7416=EDGE_LOOP('',(#31465,#31466,#31467));
#7417=EDGE_LOOP('',(#31468,#31469,#31470,#31471));
#7418=EDGE_LOOP('',(#31472,#31473,#31474));
#7419=EDGE_LOOP('',(#31475,#31476,#31477,#31478));
#7420=EDGE_LOOP('',(#31479,#31480,#31481));
#7421=EDGE_LOOP('',(#31482,#31483,#31484,#31485));
#7422=EDGE_LOOP('',(#31486,#31487,#31488));
#7423=EDGE_LOOP('',(#31489,#31490,#31491,#31492));
#7424=EDGE_LOOP('',(#31493,#31494,#31495));
#7425=EDGE_LOOP('',(#31496,#31497,#31498,#31499));
#7426=EDGE_LOOP('',(#31500,#31501,#31502));
#7427=EDGE_LOOP('',(#31503,#31504,#31505,#31506));
#7428=EDGE_LOOP('',(#31507,#31508,#31509));
#7429=EDGE_LOOP('',(#31510,#31511,#31512,#31513));
#7430=EDGE_LOOP('',(#31514,#31515,#31516));
#7431=EDGE_LOOP('',(#31517,#31518,#31519,#31520));
#7432=EDGE_LOOP('',(#31521,#31522,#31523));
#7433=EDGE_LOOP('',(#31524,#31525,#31526,#31527));
#7434=EDGE_LOOP('',(#31528,#31529,#31530));
#7435=EDGE_LOOP('',(#31531,#31532,#31533,#31534));
#7436=EDGE_LOOP('',(#31535,#31536,#31537));
#7437=EDGE_LOOP('',(#31538,#31539,#31540,#31541));
#7438=EDGE_LOOP('',(#31542,#31543,#31544));
#7439=EDGE_LOOP('',(#31545,#31546,#31547,#31548));
#7440=EDGE_LOOP('',(#31549,#31550,#31551));
#7441=EDGE_LOOP('',(#31552,#31553,#31554,#31555));
#7442=EDGE_LOOP('',(#31556,#31557,#31558));
#7443=EDGE_LOOP('',(#31559,#31560,#31561,#31562));
#7444=EDGE_LOOP('',(#31563,#31564,#31565));
#7445=EDGE_LOOP('',(#31566,#31567,#31568,#31569,#31570,#31571,#31572,#31573,
#31574,#31575,#31576,#31577));
#7446=EDGE_LOOP('',(#31578,#31579,#31580,#31581));
#7447=EDGE_LOOP('',(#31582,#31583,#31584,#31585));
#7448=EDGE_LOOP('',(#31586,#31587,#31588,#31589));
#7449=EDGE_LOOP('',(#31590,#31591,#31592,#31593));
#7450=EDGE_LOOP('',(#31594,#31595,#31596,#31597));
#7451=EDGE_LOOP('',(#31598,#31599,#31600,#31601));
#7452=EDGE_LOOP('',(#31602,#31603,#31604,#31605));
#7453=EDGE_LOOP('',(#31606,#31607,#31608,#31609));
#7454=EDGE_LOOP('',(#31610,#31611,#31612,#31613));
#7455=EDGE_LOOP('',(#31614,#31615,#31616,#31617));
#7456=EDGE_LOOP('',(#31618,#31619,#31620,#31621));
#7457=EDGE_LOOP('',(#31622,#31623,#31624,#31625));
#7458=EDGE_LOOP('',(#31626,#31627,#31628,#31629));
#7459=EDGE_LOOP('',(#31630,#31631,#31632,#31633));
#7460=EDGE_LOOP('',(#31634,#31635,#31636,#31637));
#7461=EDGE_LOOP('',(#31638,#31639,#31640,#31641));
#7462=EDGE_LOOP('',(#31642,#31643,#31644,#31645));
#7463=EDGE_LOOP('',(#31646,#31647,#31648,#31649));
#7464=EDGE_LOOP('',(#31650,#31651,#31652,#31653));
#7465=EDGE_LOOP('',(#31654,#31655,#31656,#31657));
#7466=EDGE_LOOP('',(#31658,#31659,#31660,#31661));
#7467=EDGE_LOOP('',(#31662,#31663,#31664,#31665));
#7468=EDGE_LOOP('',(#31666,#31667,#31668,#31669));
#7469=EDGE_LOOP('',(#31670,#31671,#31672,#31673));
#7470=EDGE_LOOP('',(#31674,#31675,#31676,#31677));
#7471=EDGE_LOOP('',(#31678,#31679,#31680,#31681));
#7472=EDGE_LOOP('',(#31682,#31683,#31684,#31685));
#7473=EDGE_LOOP('',(#31686,#31687,#31688,#31689));
#7474=EDGE_LOOP('',(#31690,#31691,#31692,#31693));
#7475=EDGE_LOOP('',(#31694,#31695,#31696,#31697));
#7476=EDGE_LOOP('',(#31698,#31699,#31700,#31701));
#7477=EDGE_LOOP('',(#31702,#31703,#31704,#31705));
#7478=EDGE_LOOP('',(#31706,#31707,#31708,#31709));
#7479=EDGE_LOOP('',(#31710,#31711,#31712,#31713));
#7480=EDGE_LOOP('',(#31714,#31715,#31716,#31717));
#7481=EDGE_LOOP('',(#31718,#31719,#31720,#31721,#31722,#31723));
#7482=EDGE_LOOP('',(#31724,#31725,#31726,#31727,#31728,#31729,#31730,#31731,
#31732,#31733,#31734,#31735,#31736,#31737,#31738,#31739));
#7483=EDGE_LOOP('',(#31740,#31741,#31742,#31743,#31744,#31745));
#7484=EDGE_LOOP('',(#31746,#31747,#31748,#31749,#31750,#31751,#31752));
#7485=EDGE_LOOP('',(#31753,#31754,#31755));
#7486=EDGE_LOOP('',(#31756,#31757,#31758));
#7487=EDGE_LOOP('',(#31759,#31760,#31761));
#7488=EDGE_LOOP('',(#31762,#31763,#31764));
#7489=EDGE_LOOP('',(#31765,#31766,#31767));
#7490=EDGE_LOOP('',(#31768,#31769,#31770));
#7491=EDGE_LOOP('',(#31771,#31772,#31773,#31774,#31775,#31776));
#7492=EDGE_LOOP('',(#31777));
#7493=EDGE_LOOP('',(#31778));
#7494=EDGE_LOOP('',(#31779,#31780,#31781));
#7495=EDGE_LOOP('',(#31782,#31783,#31784));
#7496=EDGE_LOOP('',(#31785,#31786,#31787));
#7497=EDGE_LOOP('',(#31788,#31789,#31790,#31791));
#7498=EDGE_LOOP('',(#31792,#31793,#31794));
#7499=EDGE_LOOP('',(#31795,#31796,#31797));
#7500=EDGE_LOOP('',(#31798,#31799,#31800));
#7501=EDGE_LOOP('',(#31801,#31802,#31803));
#7502=EDGE_LOOP('',(#31804,#31805,#31806,#31807));
#7503=EDGE_LOOP('',(#31808,#31809,#31810));
#7504=EDGE_LOOP('',(#31811,#31812,#31813));
#7505=EDGE_LOOP('',(#31814,#31815,#31816,#31817));
#7506=EDGE_LOOP('',(#31818,#31819,#31820));
#7507=EDGE_LOOP('',(#31821,#31822,#31823));
#7508=EDGE_LOOP('',(#31824,#31825,#31826));
#7509=EDGE_LOOP('',(#31827,#31828,#31829,#31830,#31831,#31832));
#7510=EDGE_LOOP('',(#31833,#31834,#31835,#31836));
#7511=EDGE_LOOP('',(#31837,#31838,#31839,#31840,#31841,#31842));
#7512=EDGE_LOOP('',(#31843,#31844,#31845,#31846));
#7513=EDGE_LOOP('',(#31847,#31848,#31849,#31850));
#7514=EDGE_LOOP('',(#31851,#31852,#31853,#31854,#31855,#31856));
#7515=EDGE_LOOP('',(#31857,#31858,#31859,#31860));
#7516=EDGE_LOOP('',(#31861,#31862,#31863,#31864));
#7517=EDGE_LOOP('',(#31865,#31866,#31867,#31868));
#7518=EDGE_LOOP('',(#31869,#31870,#31871,#31872));
#7519=EDGE_LOOP('',(#31873,#31874,#31875,#31876));
#7520=EDGE_LOOP('',(#31877,#31878,#31879,#31880));
#7521=EDGE_LOOP('',(#31881,#31882,#31883,#31884));
#7522=EDGE_LOOP('',(#31885,#31886,#31887,#31888,#31889,#31890));
#7523=EDGE_LOOP('',(#31891));
#7524=EDGE_LOOP('',(#31892,#31893,#31894,#31895));
#7525=EDGE_LOOP('',(#31896,#31897,#31898,#31899));
#7526=EDGE_LOOP('',(#31900,#31901,#31902,#31903));
#7527=EDGE_LOOP('',(#31904,#31905,#31906,#31907));
#7528=EDGE_LOOP('',(#31908,#31909,#31910,#31911));
#7529=EDGE_LOOP('',(#31912,#31913,#31914,#31915,#31916));
#7530=EDGE_LOOP('',(#31917,#31918,#31919,#31920));
#7531=EDGE_LOOP('',(#31921));
#7532=EDGE_LOOP('',(#31922));
#7533=EDGE_LOOP('',(#31923,#31924,#31925,#31926,#31927));
#7534=LINE('',#47311,#10584);
#7535=LINE('',#47317,#10585);
#7536=LINE('',#47324,#10586);
#7537=LINE('',#47327,#10587);
#7538=LINE('',#47336,#10588);
#7539=LINE('',#47343,#10589);
#7540=LINE('',#47351,#10590);
#7541=LINE('',#47357,#10591);
#7542=LINE('',#47366,#10592);
#7543=LINE('',#47372,#10593);
#7544=LINE('',#47380,#10594);
#7545=LINE('',#47386,#10595);
#7546=LINE('',#47393,#10596);
#7547=LINE('',#47396,#10597);
#7548=LINE('',#47402,#10598);
#7549=LINE('',#47408,#10599);
#7550=LINE('',#47414,#10600);
#7551=LINE('',#47420,#10601);
#7552=LINE('',#47426,#10602);
#7553=LINE('',#47432,#10603);
#7554=LINE('',#47438,#10604);
#7555=LINE('',#47445,#10605);
#7556=LINE('',#47451,#10606);
#7557=LINE('',#47459,#10607);
#7558=LINE('',#47467,#10608);
#7559=LINE('',#47475,#10609);
#7560=LINE('',#47483,#10610);
#7561=LINE('',#47491,#10611);
#7562=LINE('',#47499,#10612);
#7563=LINE('',#47507,#10613);
#7564=LINE('',#47515,#10614);
#7565=LINE('',#47523,#10615);
#7566=LINE('',#47531,#10616);
#7567=LINE('',#47539,#10617);
#7568=LINE('',#47547,#10618);
#7569=LINE('',#47555,#10619);
#7570=LINE('',#47563,#10620);
#7571=LINE('',#47571,#10621);
#7572=LINE('',#47579,#10622);
#7573=LINE('',#47587,#10623);
#7574=LINE('',#47595,#10624);
#7575=LINE('',#47603,#10625);
#7576=LINE('',#47611,#10626);
#7577=LINE('',#47619,#10627);
#7578=LINE('',#47627,#10628);
#7579=LINE('',#47635,#10629);
#7580=LINE('',#47643,#10630);
#7581=LINE('',#47651,#10631);
#7582=LINE('',#47659,#10632);
#7583=LINE('',#47667,#10633);
#7584=LINE('',#47675,#10634);
#7585=LINE('',#47683,#10635);
#7586=LINE('',#47691,#10636);
#7587=LINE('',#47699,#10637);
#7588=LINE('',#47707,#10638);
#7589=LINE('',#47715,#10639);
#7590=LINE('',#47723,#10640);
#7591=LINE('',#47731,#10641);
#7592=LINE('',#47739,#10642);
#7593=LINE('',#47747,#10643);
#7594=LINE('',#47755,#10644);
#7595=LINE('',#47763,#10645);
#7596=LINE('',#47771,#10646);
#7597=LINE('',#47779,#10647);
#7598=LINE('',#47787,#10648);
#7599=LINE('',#47795,#10649);
#7600=LINE('',#47803,#10650);
#7601=LINE('',#47811,#10651);
#7602=LINE('',#47819,#10652);
#7603=LINE('',#47827,#10653);
#7604=LINE('',#47835,#10654);
#7605=LINE('',#47843,#10655);
#7606=LINE('',#47851,#10656);
#7607=LINE('',#47859,#10657);
#7608=LINE('',#47867,#10658);
#7609=LINE('',#47875,#10659);
#7610=LINE('',#47883,#10660);
#7611=LINE('',#47891,#10661);
#7612=LINE('',#47899,#10662);
#7613=LINE('',#47907,#10663);
#7614=LINE('',#47915,#10664);
#7615=LINE('',#47923,#10665);
#7616=LINE('',#47931,#10666);
#7617=LINE('',#47939,#10667);
#7618=LINE('',#47947,#10668);
#7619=LINE('',#47955,#10669);
#7620=LINE('',#47963,#10670);
#7621=LINE('',#47971,#10671);
#7622=LINE('',#47979,#10672);
#7623=LINE('',#47987,#10673);
#7624=LINE('',#47995,#10674);
#7625=LINE('',#48003,#10675);
#7626=LINE('',#48011,#10676);
#7627=LINE('',#48019,#10677);
#7628=LINE('',#48027,#10678);
#7629=LINE('',#48035,#10679);
#7630=LINE('',#48043,#10680);
#7631=LINE('',#48051,#10681);
#7632=LINE('',#48059,#10682);
#7633=LINE('',#48067,#10683);
#7634=LINE('',#48075,#10684);
#7635=LINE('',#48083,#10685);
#7636=LINE('',#48091,#10686);
#7637=LINE('',#48099,#10687);
#7638=LINE('',#48107,#10688);
#7639=LINE('',#48115,#10689);
#7640=LINE('',#48123,#10690);
#7641=LINE('',#48131,#10691);
#7642=LINE('',#48139,#10692);
#7643=LINE('',#48147,#10693);
#7644=LINE('',#48155,#10694);
#7645=LINE('',#48163,#10695);
#7646=LINE('',#48171,#10696);
#7647=LINE('',#48179,#10697);
#7648=LINE('',#48187,#10698);
#7649=LINE('',#48195,#10699);
#7650=LINE('',#48203,#10700);
#7651=LINE('',#48211,#10701);
#7652=LINE('',#48219,#10702);
#7653=LINE('',#48227,#10703);
#7654=LINE('',#48235,#10704);
#7655=LINE('',#48243,#10705);
#7656=LINE('',#48251,#10706);
#7657=LINE('',#48259,#10707);
#7658=LINE('',#48267,#10708);
#7659=LINE('',#48275,#10709);
#7660=LINE('',#48283,#10710);
#7661=LINE('',#48291,#10711);
#7662=LINE('',#48299,#10712);
#7663=LINE('',#48307,#10713);
#7664=LINE('',#48315,#10714);
#7665=LINE('',#48323,#10715);
#7666=LINE('',#48331,#10716);
#7667=LINE('',#48339,#10717);
#7668=LINE('',#48347,#10718);
#7669=LINE('',#48355,#10719);
#7670=LINE('',#48363,#10720);
#7671=LINE('',#48371,#10721);
#7672=LINE('',#48379,#10722);
#7673=LINE('',#48387,#10723);
#7674=LINE('',#48395,#10724);
#7675=LINE('',#48403,#10725);
#7676=LINE('',#48411,#10726);
#7677=LINE('',#48419,#10727);
#7678=LINE('',#48427,#10728);
#7679=LINE('',#48435,#10729);
#7680=LINE('',#48443,#10730);
#7681=LINE('',#48451,#10731);
#7682=LINE('',#48459,#10732);
#7683=LINE('',#48467,#10733);
#7684=LINE('',#48475,#10734);
#7685=LINE('',#48483,#10735);
#7686=LINE('',#48491,#10736);
#7687=LINE('',#48499,#10737);
#7688=LINE('',#48507,#10738);
#7689=LINE('',#48515,#10739);
#7690=LINE('',#48523,#10740);
#7691=LINE('',#48531,#10741);
#7692=LINE('',#48539,#10742);
#7693=LINE('',#48547,#10743);
#7694=LINE('',#48555,#10744);
#7695=LINE('',#48563,#10745);
#7696=LINE('',#48571,#10746);
#7697=LINE('',#48579,#10747);
#7698=LINE('',#48677,#10748);
#7699=LINE('',#48680,#10749);
#7700=LINE('',#48683,#10750);
#7701=LINE('',#48687,#10751);
#7702=LINE('',#48691,#10752);
#7703=LINE('',#48695,#10753);
#7704=LINE('',#48699,#10754);
#7705=LINE('',#48715,#10755);
#7706=LINE('',#48716,#10756);
#7707=LINE('',#48718,#10757);
#7708=LINE('',#48719,#10758);
#7709=LINE('',#48722,#10759);
#7710=LINE('',#48723,#10760);
#7711=LINE('',#48726,#10761);
#7712=LINE('',#48728,#10762);
#7713=LINE('',#48729,#10763);
#7714=LINE('',#48732,#10764);
#7715=LINE('',#48734,#10765);
#7716=LINE('',#48735,#10766);
#7717=LINE('',#48738,#10767);
#7718=LINE('',#48739,#10768);
#7719=LINE('',#48742,#10769);
#7720=LINE('',#48743,#10770);
#7721=LINE('',#48745,#10771);
#7722=LINE('',#48746,#10772);
#7723=LINE('',#48750,#10773);
#7724=LINE('',#48752,#10774);
#7725=LINE('',#48753,#10775);
#7726=LINE('',#48755,#10776);
#7727=LINE('',#48756,#10777);
#7728=LINE('',#48758,#10778);
#7729=LINE('',#48759,#10779);
#7730=LINE('',#48761,#10780);
#7731=LINE('',#48762,#10781);
#7732=LINE('',#48764,#10782);
#7733=LINE('',#48770,#10783);
#7734=LINE('',#48772,#10784);
#7735=LINE('',#48773,#10785);
#7736=LINE('',#48777,#10786);
#7737=LINE('',#48779,#10787);
#7738=LINE('',#48780,#10788);
#7739=LINE('',#48784,#10789);
#7740=LINE('',#48786,#10790);
#7741=LINE('',#48787,#10791);
#7742=LINE('',#48789,#10792);
#7743=LINE('',#48790,#10793);
#7744=LINE('',#48794,#10794);
#7745=LINE('',#48796,#10795);
#7746=LINE('',#48797,#10796);
#7747=LINE('',#48799,#10797);
#7748=LINE('',#48800,#10798);
#7749=LINE('',#48802,#10799);
#7750=LINE('',#48803,#10800);
#7751=LINE('',#48805,#10801);
#7752=LINE('',#48806,#10802);
#7753=LINE('',#48808,#10803);
#7754=LINE('',#48809,#10804);
#7755=LINE('',#48811,#10805);
#7756=LINE('',#48812,#10806);
#7757=LINE('',#48814,#10807);
#7758=LINE('',#48815,#10808);
#7759=LINE('',#48817,#10809);
#7760=LINE('',#48818,#10810);
#7761=LINE('',#48825,#10811);
#7762=LINE('',#48827,#10812);
#7763=LINE('',#48828,#10813);
#7764=LINE('',#48832,#10814);
#7765=LINE('',#48833,#10815);
#7766=LINE('',#48835,#10816);
#7767=LINE('',#48836,#10817);
#7768=LINE('',#48838,#10818);
#7769=LINE('',#48839,#10819);
#7770=LINE('',#48843,#10820);
#7771=LINE('',#48845,#10821);
#7772=LINE('',#48846,#10822);
#7773=LINE('',#48850,#10823);
#7774=LINE('',#48851,#10824);
#7775=LINE('',#48853,#10825);
#7776=LINE('',#48854,#10826);
#7777=LINE('',#48856,#10827);
#7778=LINE('',#48857,#10828);
#7779=LINE('',#48859,#10829);
#7780=LINE('',#48860,#10830);
#7781=LINE('',#48863,#10831);
#7782=LINE('',#48864,#10832);
#7783=LINE('',#48865,#10833);
#7784=LINE('',#48867,#10834);
#7785=LINE('',#48870,#10835);
#7786=LINE('',#48871,#10836);
#7787=LINE('',#48873,#10837);
#7788=LINE('',#48874,#10838);
#7789=LINE('',#48880,#10839);
#7790=LINE('',#48882,#10840);
#7791=LINE('',#48883,#10841);
#7792=LINE('',#48887,#10842);
#7793=LINE('',#48889,#10843);
#7794=LINE('',#48890,#10844);
#7795=LINE('',#48894,#10845);
#7796=LINE('',#48896,#10846);
#7797=LINE('',#48897,#10847);
#7798=LINE('',#48899,#10848);
#7799=LINE('',#48900,#10849);
#7800=LINE('',#48904,#10850);
#7801=LINE('',#48906,#10851);
#7802=LINE('',#48907,#10852);
#7803=LINE('',#48909,#10853);
#7804=LINE('',#48910,#10854);
#7805=LINE('',#48912,#10855);
#7806=LINE('',#48913,#10856);
#7807=LINE('',#48915,#10857);
#7808=LINE('',#48916,#10858);
#7809=LINE('',#48918,#10859);
#7810=LINE('',#48919,#10860);
#7811=LINE('',#48921,#10861);
#7812=LINE('',#48922,#10862);
#7813=LINE('',#48924,#10863);
#7814=LINE('',#48925,#10864);
#7815=LINE('',#48927,#10865);
#7816=LINE('',#48928,#10866);
#7817=LINE('',#48935,#10867);
#7818=LINE('',#48937,#10868);
#7819=LINE('',#48938,#10869);
#7820=LINE('',#48942,#10870);
#7821=LINE('',#48944,#10871);
#7822=LINE('',#48945,#10872);
#7823=LINE('',#48949,#10873);
#7824=LINE('',#48951,#10874);
#7825=LINE('',#48952,#10875);
#7826=LINE('',#48954,#10876);
#7827=LINE('',#48955,#10877);
#7828=LINE('',#48959,#10878);
#7829=LINE('',#48961,#10879);
#7830=LINE('',#48962,#10880);
#7831=LINE('',#48964,#10881);
#7832=LINE('',#48965,#10882);
#7833=LINE('',#48967,#10883);
#7834=LINE('',#48968,#10884);
#7835=LINE('',#48970,#10885);
#7836=LINE('',#48971,#10886);
#7837=LINE('',#48973,#10887);
#7838=LINE('',#48974,#10888);
#7839=LINE('',#48976,#10889);
#7840=LINE('',#48977,#10890);
#7841=LINE('',#48979,#10891);
#7842=LINE('',#48980,#10892);
#7843=LINE('',#48982,#10893);
#7844=LINE('',#48983,#10894);
#7845=LINE('',#48990,#10895);
#7846=LINE('',#48991,#10896);
#7847=LINE('',#48993,#10897);
#7848=LINE('',#48994,#10898);
#7849=LINE('',#48997,#10899);
#7850=LINE('',#48998,#10900);
#7851=LINE('',#49001,#10901);
#7852=LINE('',#49003,#10902);
#7853=LINE('',#49004,#10903);
#7854=LINE('',#49007,#10904);
#7855=LINE('',#49009,#10905);
#7856=LINE('',#49010,#10906);
#7857=LINE('',#49013,#10907);
#7858=LINE('',#49014,#10908);
#7859=LINE('',#49017,#10909);
#7860=LINE('',#49018,#10910);
#7861=LINE('',#49020,#10911);
#7862=LINE('',#49021,#10912);
#7863=LINE('',#49025,#10913);
#7864=LINE('',#49027,#10914);
#7865=LINE('',#49028,#10915);
#7866=LINE('',#49030,#10916);
#7867=LINE('',#49031,#10917);
#7868=LINE('',#49033,#10918);
#7869=LINE('',#49034,#10919);
#7870=LINE('',#49036,#10920);
#7871=LINE('',#49037,#10921);
#7872=LINE('',#49039,#10922);
#7873=LINE('',#49045,#10923);
#7874=LINE('',#49047,#10924);
#7875=LINE('',#49048,#10925);
#7876=LINE('',#49052,#10926);
#7877=LINE('',#49054,#10927);
#7878=LINE('',#49055,#10928);
#7879=LINE('',#49059,#10929);
#7880=LINE('',#49061,#10930);
#7881=LINE('',#49062,#10931);
#7882=LINE('',#49064,#10932);
#7883=LINE('',#49065,#10933);
#7884=LINE('',#49069,#10934);
#7885=LINE('',#49071,#10935);
#7886=LINE('',#49072,#10936);
#7887=LINE('',#49074,#10937);
#7888=LINE('',#49075,#10938);
#7889=LINE('',#49077,#10939);
#7890=LINE('',#49078,#10940);
#7891=LINE('',#49080,#10941);
#7892=LINE('',#49081,#10942);
#7893=LINE('',#49083,#10943);
#7894=LINE('',#49084,#10944);
#7895=LINE('',#49086,#10945);
#7896=LINE('',#49087,#10946);
#7897=LINE('',#49089,#10947);
#7898=LINE('',#49090,#10948);
#7899=LINE('',#49092,#10949);
#7900=LINE('',#49093,#10950);
#7901=LINE('',#49100,#10951);
#7902=LINE('',#49102,#10952);
#7903=LINE('',#49103,#10953);
#7904=LINE('',#49107,#10954);
#7905=LINE('',#49108,#10955);
#7906=LINE('',#49110,#10956);
#7907=LINE('',#49111,#10957);
#7908=LINE('',#49113,#10958);
#7909=LINE('',#49114,#10959);
#7910=LINE('',#49118,#10960);
#7911=LINE('',#49120,#10961);
#7912=LINE('',#49121,#10962);
#7913=LINE('',#49125,#10963);
#7914=LINE('',#49126,#10964);
#7915=LINE('',#49128,#10965);
#7916=LINE('',#49129,#10966);
#7917=LINE('',#49131,#10967);
#7918=LINE('',#49132,#10968);
#7919=LINE('',#49134,#10969);
#7920=LINE('',#49135,#10970);
#7921=LINE('',#49138,#10971);
#7922=LINE('',#49139,#10972);
#7923=LINE('',#49140,#10973);
#7924=LINE('',#49142,#10974);
#7925=LINE('',#49145,#10975);
#7926=LINE('',#49146,#10976);
#7927=LINE('',#49148,#10977);
#7928=LINE('',#49149,#10978);
#7929=LINE('',#49155,#10979);
#7930=LINE('',#49157,#10980);
#7931=LINE('',#49158,#10981);
#7932=LINE('',#49162,#10982);
#7933=LINE('',#49164,#10983);
#7934=LINE('',#49165,#10984);
#7935=LINE('',#49169,#10985);
#7936=LINE('',#49171,#10986);
#7937=LINE('',#49172,#10987);
#7938=LINE('',#49174,#10988);
#7939=LINE('',#49175,#10989);
#7940=LINE('',#49179,#10990);
#7941=LINE('',#49181,#10991);
#7942=LINE('',#49182,#10992);
#7943=LINE('',#49184,#10993);
#7944=LINE('',#49185,#10994);
#7945=LINE('',#49187,#10995);
#7946=LINE('',#49188,#10996);
#7947=LINE('',#49190,#10997);
#7948=LINE('',#49191,#10998);
#7949=LINE('',#49193,#10999);
#7950=LINE('',#49194,#11000);
#7951=LINE('',#49196,#11001);
#7952=LINE('',#49197,#11002);
#7953=LINE('',#49199,#11003);
#7954=LINE('',#49200,#11004);
#7955=LINE('',#49202,#11005);
#7956=LINE('',#49203,#11006);
#7957=LINE('',#49210,#11007);
#7958=LINE('',#49212,#11008);
#7959=LINE('',#49213,#11009);
#7960=LINE('',#49217,#11010);
#7961=LINE('',#49219,#11011);
#7962=LINE('',#49220,#11012);
#7963=LINE('',#49224,#11013);
#7964=LINE('',#49226,#11014);
#7965=LINE('',#49227,#11015);
#7966=LINE('',#49229,#11016);
#7967=LINE('',#49230,#11017);
#7968=LINE('',#49234,#11018);
#7969=LINE('',#49236,#11019);
#7970=LINE('',#49237,#11020);
#7971=LINE('',#49239,#11021);
#7972=LINE('',#49240,#11022);
#7973=LINE('',#49242,#11023);
#7974=LINE('',#49243,#11024);
#7975=LINE('',#49245,#11025);
#7976=LINE('',#49246,#11026);
#7977=LINE('',#49248,#11027);
#7978=LINE('',#49249,#11028);
#7979=LINE('',#49251,#11029);
#7980=LINE('',#49252,#11030);
#7981=LINE('',#49254,#11031);
#7982=LINE('',#49255,#11032);
#7983=LINE('',#49257,#11033);
#7984=LINE('',#49258,#11034);
#7985=LINE('',#49265,#11035);
#7986=LINE('',#49266,#11036);
#7987=LINE('',#49268,#11037);
#7988=LINE('',#49269,#11038);
#7989=LINE('',#49272,#11039);
#7990=LINE('',#49273,#11040);
#7991=LINE('',#49276,#11041);
#7992=LINE('',#49278,#11042);
#7993=LINE('',#49279,#11043);
#7994=LINE('',#49282,#11044);
#7995=LINE('',#49284,#11045);
#7996=LINE('',#49285,#11046);
#7997=LINE('',#49288,#11047);
#7998=LINE('',#49289,#11048);
#7999=LINE('',#49292,#11049);
#8000=LINE('',#49293,#11050);
#8001=LINE('',#49295,#11051);
#8002=LINE('',#49296,#11052);
#8003=LINE('',#49300,#11053);
#8004=LINE('',#49302,#11054);
#8005=LINE('',#49303,#11055);
#8006=LINE('',#49305,#11056);
#8007=LINE('',#49306,#11057);
#8008=LINE('',#49308,#11058);
#8009=LINE('',#49309,#11059);
#8010=LINE('',#49311,#11060);
#8011=LINE('',#49312,#11061);
#8012=LINE('',#49314,#11062);
#8013=LINE('',#49320,#11063);
#8014=LINE('',#49322,#11064);
#8015=LINE('',#49323,#11065);
#8016=LINE('',#49327,#11066);
#8017=LINE('',#49329,#11067);
#8018=LINE('',#49330,#11068);
#8019=LINE('',#49334,#11069);
#8020=LINE('',#49336,#11070);
#8021=LINE('',#49337,#11071);
#8022=LINE('',#49339,#11072);
#8023=LINE('',#49340,#11073);
#8024=LINE('',#49344,#11074);
#8025=LINE('',#49346,#11075);
#8026=LINE('',#49347,#11076);
#8027=LINE('',#49349,#11077);
#8028=LINE('',#49350,#11078);
#8029=LINE('',#49352,#11079);
#8030=LINE('',#49353,#11080);
#8031=LINE('',#49355,#11081);
#8032=LINE('',#49356,#11082);
#8033=LINE('',#49358,#11083);
#8034=LINE('',#49359,#11084);
#8035=LINE('',#49361,#11085);
#8036=LINE('',#49362,#11086);
#8037=LINE('',#49364,#11087);
#8038=LINE('',#49365,#11088);
#8039=LINE('',#49367,#11089);
#8040=LINE('',#49368,#11090);
#8041=LINE('',#49375,#11091);
#8042=LINE('',#49377,#11092);
#8043=LINE('',#49378,#11093);
#8044=LINE('',#49382,#11094);
#8045=LINE('',#49383,#11095);
#8046=LINE('',#49385,#11096);
#8047=LINE('',#49386,#11097);
#8048=LINE('',#49388,#11098);
#8049=LINE('',#49389,#11099);
#8050=LINE('',#49393,#11100);
#8051=LINE('',#49395,#11101);
#8052=LINE('',#49396,#11102);
#8053=LINE('',#49400,#11103);
#8054=LINE('',#49401,#11104);
#8055=LINE('',#49403,#11105);
#8056=LINE('',#49404,#11106);
#8057=LINE('',#49406,#11107);
#8058=LINE('',#49407,#11108);
#8059=LINE('',#49409,#11109);
#8060=LINE('',#49410,#11110);
#8061=LINE('',#49413,#11111);
#8062=LINE('',#49414,#11112);
#8063=LINE('',#49415,#11113);
#8064=LINE('',#49417,#11114);
#8065=LINE('',#49420,#11115);
#8066=LINE('',#49421,#11116);
#8067=LINE('',#49423,#11117);
#8068=LINE('',#49424,#11118);
#8069=LINE('',#49430,#11119);
#8070=LINE('',#49432,#11120);
#8071=LINE('',#49433,#11121);
#8072=LINE('',#49437,#11122);
#8073=LINE('',#49439,#11123);
#8074=LINE('',#49440,#11124);
#8075=LINE('',#49444,#11125);
#8076=LINE('',#49446,#11126);
#8077=LINE('',#49447,#11127);
#8078=LINE('',#49449,#11128);
#8079=LINE('',#49450,#11129);
#8080=LINE('',#49454,#11130);
#8081=LINE('',#49456,#11131);
#8082=LINE('',#49457,#11132);
#8083=LINE('',#49459,#11133);
#8084=LINE('',#49460,#11134);
#8085=LINE('',#49462,#11135);
#8086=LINE('',#49463,#11136);
#8087=LINE('',#49465,#11137);
#8088=LINE('',#49466,#11138);
#8089=LINE('',#49468,#11139);
#8090=LINE('',#49469,#11140);
#8091=LINE('',#49471,#11141);
#8092=LINE('',#49472,#11142);
#8093=LINE('',#49474,#11143);
#8094=LINE('',#49475,#11144);
#8095=LINE('',#49477,#11145);
#8096=LINE('',#49478,#11146);
#8097=LINE('',#49485,#11147);
#8098=LINE('',#49487,#11148);
#8099=LINE('',#49488,#11149);
#8100=LINE('',#49492,#11150);
#8101=LINE('',#49494,#11151);
#8102=LINE('',#49495,#11152);
#8103=LINE('',#49499,#11153);
#8104=LINE('',#49501,#11154);
#8105=LINE('',#49502,#11155);
#8106=LINE('',#49504,#11156);
#8107=LINE('',#49505,#11157);
#8108=LINE('',#49509,#11158);
#8109=LINE('',#49511,#11159);
#8110=LINE('',#49512,#11160);
#8111=LINE('',#49514,#11161);
#8112=LINE('',#49515,#11162);
#8113=LINE('',#49517,#11163);
#8114=LINE('',#49518,#11164);
#8115=LINE('',#49520,#11165);
#8116=LINE('',#49521,#11166);
#8117=LINE('',#49523,#11167);
#8118=LINE('',#49524,#11168);
#8119=LINE('',#49526,#11169);
#8120=LINE('',#49527,#11170);
#8121=LINE('',#49529,#11171);
#8122=LINE('',#49530,#11172);
#8123=LINE('',#49532,#11173);
#8124=LINE('',#49533,#11174);
#8125=LINE('',#49540,#11175);
#8126=LINE('',#49541,#11176);
#8127=LINE('',#49543,#11177);
#8128=LINE('',#49544,#11178);
#8129=LINE('',#49547,#11179);
#8130=LINE('',#49548,#11180);
#8131=LINE('',#49551,#11181);
#8132=LINE('',#49553,#11182);
#8133=LINE('',#49554,#11183);
#8134=LINE('',#49557,#11184);
#8135=LINE('',#49559,#11185);
#8136=LINE('',#49560,#11186);
#8137=LINE('',#49563,#11187);
#8138=LINE('',#49564,#11188);
#8139=LINE('',#49567,#11189);
#8140=LINE('',#49568,#11190);
#8141=LINE('',#49570,#11191);
#8142=LINE('',#49571,#11192);
#8143=LINE('',#49575,#11193);
#8144=LINE('',#49577,#11194);
#8145=LINE('',#49578,#11195);
#8146=LINE('',#49580,#11196);
#8147=LINE('',#49581,#11197);
#8148=LINE('',#49583,#11198);
#8149=LINE('',#49584,#11199);
#8150=LINE('',#49586,#11200);
#8151=LINE('',#49587,#11201);
#8152=LINE('',#49589,#11202);
#8153=LINE('',#49595,#11203);
#8154=LINE('',#49597,#11204);
#8155=LINE('',#49598,#11205);
#8156=LINE('',#49602,#11206);
#8157=LINE('',#49604,#11207);
#8158=LINE('',#49605,#11208);
#8159=LINE('',#49609,#11209);
#8160=LINE('',#49611,#11210);
#8161=LINE('',#49612,#11211);
#8162=LINE('',#49614,#11212);
#8163=LINE('',#49615,#11213);
#8164=LINE('',#49619,#11214);
#8165=LINE('',#49621,#11215);
#8166=LINE('',#49622,#11216);
#8167=LINE('',#49624,#11217);
#8168=LINE('',#49625,#11218);
#8169=LINE('',#49627,#11219);
#8170=LINE('',#49628,#11220);
#8171=LINE('',#49630,#11221);
#8172=LINE('',#49631,#11222);
#8173=LINE('',#49633,#11223);
#8174=LINE('',#49634,#11224);
#8175=LINE('',#49636,#11225);
#8176=LINE('',#49637,#11226);
#8177=LINE('',#49639,#11227);
#8178=LINE('',#49640,#11228);
#8179=LINE('',#49642,#11229);
#8180=LINE('',#49643,#11230);
#8181=LINE('',#49650,#11231);
#8182=LINE('',#49652,#11232);
#8183=LINE('',#49653,#11233);
#8184=LINE('',#49657,#11234);
#8185=LINE('',#49658,#11235);
#8186=LINE('',#49660,#11236);
#8187=LINE('',#49661,#11237);
#8188=LINE('',#49663,#11238);
#8189=LINE('',#49664,#11239);
#8190=LINE('',#49668,#11240);
#8191=LINE('',#49670,#11241);
#8192=LINE('',#49671,#11242);
#8193=LINE('',#49675,#11243);
#8194=LINE('',#49676,#11244);
#8195=LINE('',#49678,#11245);
#8196=LINE('',#49679,#11246);
#8197=LINE('',#49681,#11247);
#8198=LINE('',#49682,#11248);
#8199=LINE('',#49684,#11249);
#8200=LINE('',#49685,#11250);
#8201=LINE('',#49688,#11251);
#8202=LINE('',#49689,#11252);
#8203=LINE('',#49690,#11253);
#8204=LINE('',#49692,#11254);
#8205=LINE('',#49695,#11255);
#8206=LINE('',#49696,#11256);
#8207=LINE('',#49698,#11257);
#8208=LINE('',#49699,#11258);
#8209=LINE('',#49705,#11259);
#8210=LINE('',#49707,#11260);
#8211=LINE('',#49708,#11261);
#8212=LINE('',#49712,#11262);
#8213=LINE('',#49714,#11263);
#8214=LINE('',#49715,#11264);
#8215=LINE('',#49719,#11265);
#8216=LINE('',#49721,#11266);
#8217=LINE('',#49722,#11267);
#8218=LINE('',#49724,#11268);
#8219=LINE('',#49725,#11269);
#8220=LINE('',#49729,#11270);
#8221=LINE('',#49731,#11271);
#8222=LINE('',#49732,#11272);
#8223=LINE('',#49734,#11273);
#8224=LINE('',#49735,#11274);
#8225=LINE('',#49737,#11275);
#8226=LINE('',#49738,#11276);
#8227=LINE('',#49740,#11277);
#8228=LINE('',#49741,#11278);
#8229=LINE('',#49743,#11279);
#8230=LINE('',#49744,#11280);
#8231=LINE('',#49746,#11281);
#8232=LINE('',#49747,#11282);
#8233=LINE('',#49749,#11283);
#8234=LINE('',#49750,#11284);
#8235=LINE('',#49752,#11285);
#8236=LINE('',#49753,#11286);
#8237=LINE('',#49760,#11287);
#8238=LINE('',#49762,#11288);
#8239=LINE('',#49763,#11289);
#8240=LINE('',#49767,#11290);
#8241=LINE('',#49769,#11291);
#8242=LINE('',#49770,#11292);
#8243=LINE('',#49774,#11293);
#8244=LINE('',#49776,#11294);
#8245=LINE('',#49777,#11295);
#8246=LINE('',#49779,#11296);
#8247=LINE('',#49780,#11297);
#8248=LINE('',#49784,#11298);
#8249=LINE('',#49786,#11299);
#8250=LINE('',#49787,#11300);
#8251=LINE('',#49789,#11301);
#8252=LINE('',#49790,#11302);
#8253=LINE('',#49792,#11303);
#8254=LINE('',#49793,#11304);
#8255=LINE('',#49795,#11305);
#8256=LINE('',#49796,#11306);
#8257=LINE('',#49798,#11307);
#8258=LINE('',#49799,#11308);
#8259=LINE('',#49801,#11309);
#8260=LINE('',#49802,#11310);
#8261=LINE('',#49804,#11311);
#8262=LINE('',#49805,#11312);
#8263=LINE('',#49807,#11313);
#8264=LINE('',#49808,#11314);
#8265=LINE('',#49815,#11315);
#8266=LINE('',#49816,#11316);
#8267=LINE('',#49818,#11317);
#8268=LINE('',#49819,#11318);
#8269=LINE('',#49822,#11319);
#8270=LINE('',#49823,#11320);
#8271=LINE('',#49826,#11321);
#8272=LINE('',#49828,#11322);
#8273=LINE('',#49829,#11323);
#8274=LINE('',#49832,#11324);
#8275=LINE('',#49834,#11325);
#8276=LINE('',#49835,#11326);
#8277=LINE('',#49838,#11327);
#8278=LINE('',#49839,#11328);
#8279=LINE('',#49842,#11329);
#8280=LINE('',#49843,#11330);
#8281=LINE('',#49845,#11331);
#8282=LINE('',#49846,#11332);
#8283=LINE('',#49850,#11333);
#8284=LINE('',#49852,#11334);
#8285=LINE('',#49853,#11335);
#8286=LINE('',#49855,#11336);
#8287=LINE('',#49856,#11337);
#8288=LINE('',#49858,#11338);
#8289=LINE('',#49859,#11339);
#8290=LINE('',#49861,#11340);
#8291=LINE('',#49862,#11341);
#8292=LINE('',#49864,#11342);
#8293=LINE('',#49870,#11343);
#8294=LINE('',#49872,#11344);
#8295=LINE('',#49873,#11345);
#8296=LINE('',#49877,#11346);
#8297=LINE('',#49879,#11347);
#8298=LINE('',#49880,#11348);
#8299=LINE('',#49884,#11349);
#8300=LINE('',#49886,#11350);
#8301=LINE('',#49887,#11351);
#8302=LINE('',#49889,#11352);
#8303=LINE('',#49890,#11353);
#8304=LINE('',#49894,#11354);
#8305=LINE('',#49896,#11355);
#8306=LINE('',#49897,#11356);
#8307=LINE('',#49899,#11357);
#8308=LINE('',#49900,#11358);
#8309=LINE('',#49902,#11359);
#8310=LINE('',#49903,#11360);
#8311=LINE('',#49905,#11361);
#8312=LINE('',#49906,#11362);
#8313=LINE('',#49908,#11363);
#8314=LINE('',#49909,#11364);
#8315=LINE('',#49911,#11365);
#8316=LINE('',#49912,#11366);
#8317=LINE('',#49914,#11367);
#8318=LINE('',#49915,#11368);
#8319=LINE('',#49917,#11369);
#8320=LINE('',#49918,#11370);
#8321=LINE('',#49925,#11371);
#8322=LINE('',#49927,#11372);
#8323=LINE('',#49928,#11373);
#8324=LINE('',#49932,#11374);
#8325=LINE('',#49933,#11375);
#8326=LINE('',#49935,#11376);
#8327=LINE('',#49936,#11377);
#8328=LINE('',#49938,#11378);
#8329=LINE('',#49939,#11379);
#8330=LINE('',#49943,#11380);
#8331=LINE('',#49945,#11381);
#8332=LINE('',#49946,#11382);
#8333=LINE('',#49950,#11383);
#8334=LINE('',#49951,#11384);
#8335=LINE('',#49953,#11385);
#8336=LINE('',#49954,#11386);
#8337=LINE('',#49956,#11387);
#8338=LINE('',#49957,#11388);
#8339=LINE('',#49959,#11389);
#8340=LINE('',#49960,#11390);
#8341=LINE('',#49963,#11391);
#8342=LINE('',#49964,#11392);
#8343=LINE('',#49965,#11393);
#8344=LINE('',#49967,#11394);
#8345=LINE('',#49970,#11395);
#8346=LINE('',#49971,#11396);
#8347=LINE('',#49973,#11397);
#8348=LINE('',#49974,#11398);
#8349=LINE('',#49980,#11399);
#8350=LINE('',#49982,#11400);
#8351=LINE('',#49983,#11401);
#8352=LINE('',#49987,#11402);
#8353=LINE('',#49989,#11403);
#8354=LINE('',#49990,#11404);
#8355=LINE('',#49994,#11405);
#8356=LINE('',#49996,#11406);
#8357=LINE('',#49997,#11407);
#8358=LINE('',#49999,#11408);
#8359=LINE('',#50000,#11409);
#8360=LINE('',#50004,#11410);
#8361=LINE('',#50006,#11411);
#8362=LINE('',#50007,#11412);
#8363=LINE('',#50009,#11413);
#8364=LINE('',#50010,#11414);
#8365=LINE('',#50012,#11415);
#8366=LINE('',#50013,#11416);
#8367=LINE('',#50015,#11417);
#8368=LINE('',#50016,#11418);
#8369=LINE('',#50018,#11419);
#8370=LINE('',#50019,#11420);
#8371=LINE('',#50021,#11421);
#8372=LINE('',#50022,#11422);
#8373=LINE('',#50024,#11423);
#8374=LINE('',#50025,#11424);
#8375=LINE('',#50027,#11425);
#8376=LINE('',#50028,#11426);
#8377=LINE('',#50035,#11427);
#8378=LINE('',#50037,#11428);
#8379=LINE('',#50038,#11429);
#8380=LINE('',#50042,#11430);
#8381=LINE('',#50044,#11431);
#8382=LINE('',#50045,#11432);
#8383=LINE('',#50049,#11433);
#8384=LINE('',#50051,#11434);
#8385=LINE('',#50052,#11435);
#8386=LINE('',#50054,#11436);
#8387=LINE('',#50055,#11437);
#8388=LINE('',#50059,#11438);
#8389=LINE('',#50061,#11439);
#8390=LINE('',#50062,#11440);
#8391=LINE('',#50064,#11441);
#8392=LINE('',#50065,#11442);
#8393=LINE('',#50067,#11443);
#8394=LINE('',#50068,#11444);
#8395=LINE('',#50070,#11445);
#8396=LINE('',#50071,#11446);
#8397=LINE('',#50073,#11447);
#8398=LINE('',#50074,#11448);
#8399=LINE('',#50076,#11449);
#8400=LINE('',#50077,#11450);
#8401=LINE('',#50079,#11451);
#8402=LINE('',#50080,#11452);
#8403=LINE('',#50082,#11453);
#8404=LINE('',#50083,#11454);
#8405=LINE('',#50090,#11455);
#8406=LINE('',#50091,#11456);
#8407=LINE('',#50093,#11457);
#8408=LINE('',#50094,#11458);
#8409=LINE('',#50097,#11459);
#8410=LINE('',#50098,#11460);
#8411=LINE('',#50101,#11461);
#8412=LINE('',#50103,#11462);
#8413=LINE('',#50104,#11463);
#8414=LINE('',#50107,#11464);
#8415=LINE('',#50109,#11465);
#8416=LINE('',#50110,#11466);
#8417=LINE('',#50113,#11467);
#8418=LINE('',#50114,#11468);
#8419=LINE('',#50117,#11469);
#8420=LINE('',#50118,#11470);
#8421=LINE('',#50120,#11471);
#8422=LINE('',#50121,#11472);
#8423=LINE('',#50125,#11473);
#8424=LINE('',#50127,#11474);
#8425=LINE('',#50128,#11475);
#8426=LINE('',#50130,#11476);
#8427=LINE('',#50131,#11477);
#8428=LINE('',#50133,#11478);
#8429=LINE('',#50134,#11479);
#8430=LINE('',#50136,#11480);
#8431=LINE('',#50137,#11481);
#8432=LINE('',#50139,#11482);
#8433=LINE('',#50145,#11483);
#8434=LINE('',#50147,#11484);
#8435=LINE('',#50148,#11485);
#8436=LINE('',#50152,#11486);
#8437=LINE('',#50154,#11487);
#8438=LINE('',#50155,#11488);
#8439=LINE('',#50159,#11489);
#8440=LINE('',#50161,#11490);
#8441=LINE('',#50162,#11491);
#8442=LINE('',#50164,#11492);
#8443=LINE('',#50165,#11493);
#8444=LINE('',#50169,#11494);
#8445=LINE('',#50171,#11495);
#8446=LINE('',#50172,#11496);
#8447=LINE('',#50174,#11497);
#8448=LINE('',#50175,#11498);
#8449=LINE('',#50177,#11499);
#8450=LINE('',#50178,#11500);
#8451=LINE('',#50180,#11501);
#8452=LINE('',#50181,#11502);
#8453=LINE('',#50183,#11503);
#8454=LINE('',#50184,#11504);
#8455=LINE('',#50186,#11505);
#8456=LINE('',#50187,#11506);
#8457=LINE('',#50189,#11507);
#8458=LINE('',#50190,#11508);
#8459=LINE('',#50192,#11509);
#8460=LINE('',#50193,#11510);
#8461=LINE('',#50200,#11511);
#8462=LINE('',#50202,#11512);
#8463=LINE('',#50203,#11513);
#8464=LINE('',#50207,#11514);
#8465=LINE('',#50208,#11515);
#8466=LINE('',#50210,#11516);
#8467=LINE('',#50211,#11517);
#8468=LINE('',#50213,#11518);
#8469=LINE('',#50214,#11519);
#8470=LINE('',#50218,#11520);
#8471=LINE('',#50220,#11521);
#8472=LINE('',#50221,#11522);
#8473=LINE('',#50225,#11523);
#8474=LINE('',#50226,#11524);
#8475=LINE('',#50228,#11525);
#8476=LINE('',#50229,#11526);
#8477=LINE('',#50231,#11527);
#8478=LINE('',#50232,#11528);
#8479=LINE('',#50234,#11529);
#8480=LINE('',#50235,#11530);
#8481=LINE('',#50238,#11531);
#8482=LINE('',#50239,#11532);
#8483=LINE('',#50240,#11533);
#8484=LINE('',#50242,#11534);
#8485=LINE('',#50245,#11535);
#8486=LINE('',#50246,#11536);
#8487=LINE('',#50248,#11537);
#8488=LINE('',#50249,#11538);
#8489=LINE('',#50255,#11539);
#8490=LINE('',#50257,#11540);
#8491=LINE('',#50258,#11541);
#8492=LINE('',#50262,#11542);
#8493=LINE('',#50264,#11543);
#8494=LINE('',#50265,#11544);
#8495=LINE('',#50269,#11545);
#8496=LINE('',#50271,#11546);
#8497=LINE('',#50272,#11547);
#8498=LINE('',#50274,#11548);
#8499=LINE('',#50275,#11549);
#8500=LINE('',#50279,#11550);
#8501=LINE('',#50281,#11551);
#8502=LINE('',#50282,#11552);
#8503=LINE('',#50284,#11553);
#8504=LINE('',#50285,#11554);
#8505=LINE('',#50287,#11555);
#8506=LINE('',#50288,#11556);
#8507=LINE('',#50290,#11557);
#8508=LINE('',#50291,#11558);
#8509=LINE('',#50293,#11559);
#8510=LINE('',#50294,#11560);
#8511=LINE('',#50296,#11561);
#8512=LINE('',#50297,#11562);
#8513=LINE('',#50299,#11563);
#8514=LINE('',#50300,#11564);
#8515=LINE('',#50302,#11565);
#8516=LINE('',#50303,#11566);
#8517=LINE('',#50310,#11567);
#8518=LINE('',#50312,#11568);
#8519=LINE('',#50313,#11569);
#8520=LINE('',#50317,#11570);
#8521=LINE('',#50319,#11571);
#8522=LINE('',#50320,#11572);
#8523=LINE('',#50324,#11573);
#8524=LINE('',#50326,#11574);
#8525=LINE('',#50327,#11575);
#8526=LINE('',#50329,#11576);
#8527=LINE('',#50330,#11577);
#8528=LINE('',#50334,#11578);
#8529=LINE('',#50336,#11579);
#8530=LINE('',#50337,#11580);
#8531=LINE('',#50339,#11581);
#8532=LINE('',#50340,#11582);
#8533=LINE('',#50342,#11583);
#8534=LINE('',#50343,#11584);
#8535=LINE('',#50345,#11585);
#8536=LINE('',#50346,#11586);
#8537=LINE('',#50348,#11587);
#8538=LINE('',#50349,#11588);
#8539=LINE('',#50351,#11589);
#8540=LINE('',#50352,#11590);
#8541=LINE('',#50354,#11591);
#8542=LINE('',#50355,#11592);
#8543=LINE('',#50357,#11593);
#8544=LINE('',#50358,#11594);
#8545=LINE('',#50365,#11595);
#8546=LINE('',#50366,#11596);
#8547=LINE('',#50368,#11597);
#8548=LINE('',#50369,#11598);
#8549=LINE('',#50372,#11599);
#8550=LINE('',#50373,#11600);
#8551=LINE('',#50376,#11601);
#8552=LINE('',#50378,#11602);
#8553=LINE('',#50379,#11603);
#8554=LINE('',#50382,#11604);
#8555=LINE('',#50384,#11605);
#8556=LINE('',#50385,#11606);
#8557=LINE('',#50388,#11607);
#8558=LINE('',#50389,#11608);
#8559=LINE('',#50392,#11609);
#8560=LINE('',#50393,#11610);
#8561=LINE('',#50395,#11611);
#8562=LINE('',#50396,#11612);
#8563=LINE('',#50400,#11613);
#8564=LINE('',#50402,#11614);
#8565=LINE('',#50403,#11615);
#8566=LINE('',#50405,#11616);
#8567=LINE('',#50406,#11617);
#8568=LINE('',#50408,#11618);
#8569=LINE('',#50409,#11619);
#8570=LINE('',#50411,#11620);
#8571=LINE('',#50412,#11621);
#8572=LINE('',#50414,#11622);
#8573=LINE('',#50420,#11623);
#8574=LINE('',#50422,#11624);
#8575=LINE('',#50423,#11625);
#8576=LINE('',#50427,#11626);
#8577=LINE('',#50429,#11627);
#8578=LINE('',#50430,#11628);
#8579=LINE('',#50434,#11629);
#8580=LINE('',#50436,#11630);
#8581=LINE('',#50437,#11631);
#8582=LINE('',#50439,#11632);
#8583=LINE('',#50440,#11633);
#8584=LINE('',#50444,#11634);
#8585=LINE('',#50446,#11635);
#8586=LINE('',#50447,#11636);
#8587=LINE('',#50449,#11637);
#8588=LINE('',#50450,#11638);
#8589=LINE('',#50452,#11639);
#8590=LINE('',#50453,#11640);
#8591=LINE('',#50455,#11641);
#8592=LINE('',#50456,#11642);
#8593=LINE('',#50458,#11643);
#8594=LINE('',#50459,#11644);
#8595=LINE('',#50461,#11645);
#8596=LINE('',#50462,#11646);
#8597=LINE('',#50464,#11647);
#8598=LINE('',#50465,#11648);
#8599=LINE('',#50467,#11649);
#8600=LINE('',#50468,#11650);
#8601=LINE('',#50475,#11651);
#8602=LINE('',#50477,#11652);
#8603=LINE('',#50478,#11653);
#8604=LINE('',#50482,#11654);
#8605=LINE('',#50483,#11655);
#8606=LINE('',#50485,#11656);
#8607=LINE('',#50486,#11657);
#8608=LINE('',#50488,#11658);
#8609=LINE('',#50489,#11659);
#8610=LINE('',#50493,#11660);
#8611=LINE('',#50495,#11661);
#8612=LINE('',#50496,#11662);
#8613=LINE('',#50500,#11663);
#8614=LINE('',#50501,#11664);
#8615=LINE('',#50503,#11665);
#8616=LINE('',#50504,#11666);
#8617=LINE('',#50506,#11667);
#8618=LINE('',#50507,#11668);
#8619=LINE('',#50509,#11669);
#8620=LINE('',#50510,#11670);
#8621=LINE('',#50513,#11671);
#8622=LINE('',#50514,#11672);
#8623=LINE('',#50515,#11673);
#8624=LINE('',#50517,#11674);
#8625=LINE('',#50520,#11675);
#8626=LINE('',#50521,#11676);
#8627=LINE('',#50523,#11677);
#8628=LINE('',#50524,#11678);
#8629=LINE('',#50530,#11679);
#8630=LINE('',#50532,#11680);
#8631=LINE('',#50533,#11681);
#8632=LINE('',#50537,#11682);
#8633=LINE('',#50539,#11683);
#8634=LINE('',#50540,#11684);
#8635=LINE('',#50544,#11685);
#8636=LINE('',#50546,#11686);
#8637=LINE('',#50547,#11687);
#8638=LINE('',#50549,#11688);
#8639=LINE('',#50550,#11689);
#8640=LINE('',#50554,#11690);
#8641=LINE('',#50556,#11691);
#8642=LINE('',#50557,#11692);
#8643=LINE('',#50559,#11693);
#8644=LINE('',#50560,#11694);
#8645=LINE('',#50562,#11695);
#8646=LINE('',#50563,#11696);
#8647=LINE('',#50565,#11697);
#8648=LINE('',#50566,#11698);
#8649=LINE('',#50568,#11699);
#8650=LINE('',#50569,#11700);
#8651=LINE('',#50571,#11701);
#8652=LINE('',#50572,#11702);
#8653=LINE('',#50574,#11703);
#8654=LINE('',#50575,#11704);
#8655=LINE('',#50577,#11705);
#8656=LINE('',#50578,#11706);
#8657=LINE('',#50585,#11707);
#8658=LINE('',#50587,#11708);
#8659=LINE('',#50588,#11709);
#8660=LINE('',#50592,#11710);
#8661=LINE('',#50594,#11711);
#8662=LINE('',#50595,#11712);
#8663=LINE('',#50599,#11713);
#8664=LINE('',#50601,#11714);
#8665=LINE('',#50602,#11715);
#8666=LINE('',#50604,#11716);
#8667=LINE('',#50605,#11717);
#8668=LINE('',#50609,#11718);
#8669=LINE('',#50611,#11719);
#8670=LINE('',#50612,#11720);
#8671=LINE('',#50614,#11721);
#8672=LINE('',#50615,#11722);
#8673=LINE('',#50617,#11723);
#8674=LINE('',#50618,#11724);
#8675=LINE('',#50620,#11725);
#8676=LINE('',#50621,#11726);
#8677=LINE('',#50623,#11727);
#8678=LINE('',#50624,#11728);
#8679=LINE('',#50626,#11729);
#8680=LINE('',#50627,#11730);
#8681=LINE('',#50629,#11731);
#8682=LINE('',#50630,#11732);
#8683=LINE('',#50632,#11733);
#8684=LINE('',#50633,#11734);
#8685=LINE('',#50640,#11735);
#8686=LINE('',#50641,#11736);
#8687=LINE('',#50643,#11737);
#8688=LINE('',#50644,#11738);
#8689=LINE('',#50647,#11739);
#8690=LINE('',#50648,#11740);
#8691=LINE('',#50651,#11741);
#8692=LINE('',#50653,#11742);
#8693=LINE('',#50654,#11743);
#8694=LINE('',#50657,#11744);
#8695=LINE('',#50659,#11745);
#8696=LINE('',#50660,#11746);
#8697=LINE('',#50663,#11747);
#8698=LINE('',#50664,#11748);
#8699=LINE('',#50667,#11749);
#8700=LINE('',#50668,#11750);
#8701=LINE('',#50670,#11751);
#8702=LINE('',#50671,#11752);
#8703=LINE('',#50675,#11753);
#8704=LINE('',#50677,#11754);
#8705=LINE('',#50678,#11755);
#8706=LINE('',#50680,#11756);
#8707=LINE('',#50681,#11757);
#8708=LINE('',#50683,#11758);
#8709=LINE('',#50684,#11759);
#8710=LINE('',#50686,#11760);
#8711=LINE('',#50687,#11761);
#8712=LINE('',#50689,#11762);
#8713=LINE('',#50695,#11763);
#8714=LINE('',#50697,#11764);
#8715=LINE('',#50698,#11765);
#8716=LINE('',#50702,#11766);
#8717=LINE('',#50704,#11767);
#8718=LINE('',#50705,#11768);
#8719=LINE('',#50709,#11769);
#8720=LINE('',#50711,#11770);
#8721=LINE('',#50712,#11771);
#8722=LINE('',#50714,#11772);
#8723=LINE('',#50715,#11773);
#8724=LINE('',#50719,#11774);
#8725=LINE('',#50721,#11775);
#8726=LINE('',#50722,#11776);
#8727=LINE('',#50724,#11777);
#8728=LINE('',#50725,#11778);
#8729=LINE('',#50727,#11779);
#8730=LINE('',#50728,#11780);
#8731=LINE('',#50730,#11781);
#8732=LINE('',#50731,#11782);
#8733=LINE('',#50733,#11783);
#8734=LINE('',#50734,#11784);
#8735=LINE('',#50736,#11785);
#8736=LINE('',#50737,#11786);
#8737=LINE('',#50739,#11787);
#8738=LINE('',#50740,#11788);
#8739=LINE('',#50742,#11789);
#8740=LINE('',#50743,#11790);
#8741=LINE('',#50750,#11791);
#8742=LINE('',#50752,#11792);
#8743=LINE('',#50753,#11793);
#8744=LINE('',#50757,#11794);
#8745=LINE('',#50758,#11795);
#8746=LINE('',#50760,#11796);
#8747=LINE('',#50761,#11797);
#8748=LINE('',#50763,#11798);
#8749=LINE('',#50764,#11799);
#8750=LINE('',#50768,#11800);
#8751=LINE('',#50770,#11801);
#8752=LINE('',#50771,#11802);
#8753=LINE('',#50775,#11803);
#8754=LINE('',#50776,#11804);
#8755=LINE('',#50778,#11805);
#8756=LINE('',#50779,#11806);
#8757=LINE('',#50781,#11807);
#8758=LINE('',#50782,#11808);
#8759=LINE('',#50784,#11809);
#8760=LINE('',#50785,#11810);
#8761=LINE('',#50788,#11811);
#8762=LINE('',#50789,#11812);
#8763=LINE('',#50790,#11813);
#8764=LINE('',#50792,#11814);
#8765=LINE('',#50795,#11815);
#8766=LINE('',#50796,#11816);
#8767=LINE('',#50798,#11817);
#8768=LINE('',#50799,#11818);
#8769=LINE('',#50805,#11819);
#8770=LINE('',#50807,#11820);
#8771=LINE('',#50808,#11821);
#8772=LINE('',#50812,#11822);
#8773=LINE('',#50814,#11823);
#8774=LINE('',#50815,#11824);
#8775=LINE('',#50819,#11825);
#8776=LINE('',#50821,#11826);
#8777=LINE('',#50822,#11827);
#8778=LINE('',#50824,#11828);
#8779=LINE('',#50825,#11829);
#8780=LINE('',#50829,#11830);
#8781=LINE('',#50831,#11831);
#8782=LINE('',#50832,#11832);
#8783=LINE('',#50834,#11833);
#8784=LINE('',#50835,#11834);
#8785=LINE('',#50837,#11835);
#8786=LINE('',#50838,#11836);
#8787=LINE('',#50840,#11837);
#8788=LINE('',#50841,#11838);
#8789=LINE('',#50843,#11839);
#8790=LINE('',#50844,#11840);
#8791=LINE('',#50846,#11841);
#8792=LINE('',#50847,#11842);
#8793=LINE('',#50849,#11843);
#8794=LINE('',#50850,#11844);
#8795=LINE('',#50852,#11845);
#8796=LINE('',#50853,#11846);
#8797=LINE('',#50860,#11847);
#8798=LINE('',#50862,#11848);
#8799=LINE('',#50863,#11849);
#8800=LINE('',#50867,#11850);
#8801=LINE('',#50869,#11851);
#8802=LINE('',#50870,#11852);
#8803=LINE('',#50874,#11853);
#8804=LINE('',#50876,#11854);
#8805=LINE('',#50877,#11855);
#8806=LINE('',#50879,#11856);
#8807=LINE('',#50880,#11857);
#8808=LINE('',#50884,#11858);
#8809=LINE('',#50886,#11859);
#8810=LINE('',#50887,#11860);
#8811=LINE('',#50889,#11861);
#8812=LINE('',#50890,#11862);
#8813=LINE('',#50892,#11863);
#8814=LINE('',#50893,#11864);
#8815=LINE('',#50895,#11865);
#8816=LINE('',#50896,#11866);
#8817=LINE('',#50898,#11867);
#8818=LINE('',#50899,#11868);
#8819=LINE('',#50901,#11869);
#8820=LINE('',#50902,#11870);
#8821=LINE('',#50904,#11871);
#8822=LINE('',#50905,#11872);
#8823=LINE('',#50907,#11873);
#8824=LINE('',#50908,#11874);
#8825=LINE('',#50915,#11875);
#8826=LINE('',#50916,#11876);
#8827=LINE('',#50918,#11877);
#8828=LINE('',#50919,#11878);
#8829=LINE('',#50922,#11879);
#8830=LINE('',#50923,#11880);
#8831=LINE('',#50926,#11881);
#8832=LINE('',#50928,#11882);
#8833=LINE('',#50929,#11883);
#8834=LINE('',#50932,#11884);
#8835=LINE('',#50934,#11885);
#8836=LINE('',#50935,#11886);
#8837=LINE('',#50938,#11887);
#8838=LINE('',#50939,#11888);
#8839=LINE('',#50942,#11889);
#8840=LINE('',#50943,#11890);
#8841=LINE('',#50945,#11891);
#8842=LINE('',#50946,#11892);
#8843=LINE('',#50950,#11893);
#8844=LINE('',#50952,#11894);
#8845=LINE('',#50953,#11895);
#8846=LINE('',#50955,#11896);
#8847=LINE('',#50956,#11897);
#8848=LINE('',#50958,#11898);
#8849=LINE('',#50959,#11899);
#8850=LINE('',#50961,#11900);
#8851=LINE('',#50962,#11901);
#8852=LINE('',#50964,#11902);
#8853=LINE('',#50970,#11903);
#8854=LINE('',#50972,#11904);
#8855=LINE('',#50973,#11905);
#8856=LINE('',#50977,#11906);
#8857=LINE('',#50979,#11907);
#8858=LINE('',#50980,#11908);
#8859=LINE('',#50984,#11909);
#8860=LINE('',#50986,#11910);
#8861=LINE('',#50987,#11911);
#8862=LINE('',#50989,#11912);
#8863=LINE('',#50990,#11913);
#8864=LINE('',#50994,#11914);
#8865=LINE('',#50996,#11915);
#8866=LINE('',#50997,#11916);
#8867=LINE('',#50999,#11917);
#8868=LINE('',#51000,#11918);
#8869=LINE('',#51002,#11919);
#8870=LINE('',#51003,#11920);
#8871=LINE('',#51005,#11921);
#8872=LINE('',#51006,#11922);
#8873=LINE('',#51008,#11923);
#8874=LINE('',#51009,#11924);
#8875=LINE('',#51011,#11925);
#8876=LINE('',#51012,#11926);
#8877=LINE('',#51014,#11927);
#8878=LINE('',#51015,#11928);
#8879=LINE('',#51017,#11929);
#8880=LINE('',#51018,#11930);
#8881=LINE('',#51025,#11931);
#8882=LINE('',#51027,#11932);
#8883=LINE('',#51028,#11933);
#8884=LINE('',#51032,#11934);
#8885=LINE('',#51033,#11935);
#8886=LINE('',#51035,#11936);
#8887=LINE('',#51036,#11937);
#8888=LINE('',#51038,#11938);
#8889=LINE('',#51039,#11939);
#8890=LINE('',#51043,#11940);
#8891=LINE('',#51045,#11941);
#8892=LINE('',#51046,#11942);
#8893=LINE('',#51050,#11943);
#8894=LINE('',#51051,#11944);
#8895=LINE('',#51053,#11945);
#8896=LINE('',#51054,#11946);
#8897=LINE('',#51056,#11947);
#8898=LINE('',#51057,#11948);
#8899=LINE('',#51059,#11949);
#8900=LINE('',#51060,#11950);
#8901=LINE('',#51063,#11951);
#8902=LINE('',#51064,#11952);
#8903=LINE('',#51065,#11953);
#8904=LINE('',#51067,#11954);
#8905=LINE('',#51070,#11955);
#8906=LINE('',#51071,#11956);
#8907=LINE('',#51073,#11957);
#8908=LINE('',#51074,#11958);
#8909=LINE('',#51080,#11959);
#8910=LINE('',#51082,#11960);
#8911=LINE('',#51083,#11961);
#8912=LINE('',#51087,#11962);
#8913=LINE('',#51089,#11963);
#8914=LINE('',#51090,#11964);
#8915=LINE('',#51094,#11965);
#8916=LINE('',#51096,#11966);
#8917=LINE('',#51097,#11967);
#8918=LINE('',#51099,#11968);
#8919=LINE('',#51100,#11969);
#8920=LINE('',#51104,#11970);
#8921=LINE('',#51106,#11971);
#8922=LINE('',#51107,#11972);
#8923=LINE('',#51109,#11973);
#8924=LINE('',#51110,#11974);
#8925=LINE('',#51112,#11975);
#8926=LINE('',#51113,#11976);
#8927=LINE('',#51115,#11977);
#8928=LINE('',#51116,#11978);
#8929=LINE('',#51118,#11979);
#8930=LINE('',#51119,#11980);
#8931=LINE('',#51121,#11981);
#8932=LINE('',#51122,#11982);
#8933=LINE('',#51124,#11983);
#8934=LINE('',#51125,#11984);
#8935=LINE('',#51127,#11985);
#8936=LINE('',#51128,#11986);
#8937=LINE('',#51135,#11987);
#8938=LINE('',#51137,#11988);
#8939=LINE('',#51138,#11989);
#8940=LINE('',#51142,#11990);
#8941=LINE('',#51144,#11991);
#8942=LINE('',#51145,#11992);
#8943=LINE('',#51149,#11993);
#8944=LINE('',#51151,#11994);
#8945=LINE('',#51152,#11995);
#8946=LINE('',#51154,#11996);
#8947=LINE('',#51155,#11997);
#8948=LINE('',#51159,#11998);
#8949=LINE('',#51161,#11999);
#8950=LINE('',#51162,#12000);
#8951=LINE('',#51164,#12001);
#8952=LINE('',#51165,#12002);
#8953=LINE('',#51167,#12003);
#8954=LINE('',#51168,#12004);
#8955=LINE('',#51170,#12005);
#8956=LINE('',#51171,#12006);
#8957=LINE('',#51173,#12007);
#8958=LINE('',#51174,#12008);
#8959=LINE('',#51176,#12009);
#8960=LINE('',#51177,#12010);
#8961=LINE('',#51179,#12011);
#8962=LINE('',#51180,#12012);
#8963=LINE('',#51182,#12013);
#8964=LINE('',#51183,#12014);
#8965=LINE('',#51190,#12015);
#8966=LINE('',#51191,#12016);
#8967=LINE('',#51193,#12017);
#8968=LINE('',#51194,#12018);
#8969=LINE('',#51197,#12019);
#8970=LINE('',#51198,#12020);
#8971=LINE('',#51201,#12021);
#8972=LINE('',#51203,#12022);
#8973=LINE('',#51204,#12023);
#8974=LINE('',#51207,#12024);
#8975=LINE('',#51209,#12025);
#8976=LINE('',#51210,#12026);
#8977=LINE('',#51213,#12027);
#8978=LINE('',#51214,#12028);
#8979=LINE('',#51217,#12029);
#8980=LINE('',#51218,#12030);
#8981=LINE('',#51220,#12031);
#8982=LINE('',#51221,#12032);
#8983=LINE('',#51225,#12033);
#8984=LINE('',#51227,#12034);
#8985=LINE('',#51228,#12035);
#8986=LINE('',#51230,#12036);
#8987=LINE('',#51231,#12037);
#8988=LINE('',#51233,#12038);
#8989=LINE('',#51234,#12039);
#8990=LINE('',#51236,#12040);
#8991=LINE('',#51237,#12041);
#8992=LINE('',#51239,#12042);
#8993=LINE('',#51245,#12043);
#8994=LINE('',#51247,#12044);
#8995=LINE('',#51248,#12045);
#8996=LINE('',#51252,#12046);
#8997=LINE('',#51254,#12047);
#8998=LINE('',#51255,#12048);
#8999=LINE('',#51259,#12049);
#9000=LINE('',#51261,#12050);
#9001=LINE('',#51262,#12051);
#9002=LINE('',#51264,#12052);
#9003=LINE('',#51265,#12053);
#9004=LINE('',#51269,#12054);
#9005=LINE('',#51271,#12055);
#9006=LINE('',#51272,#12056);
#9007=LINE('',#51274,#12057);
#9008=LINE('',#51275,#12058);
#9009=LINE('',#51277,#12059);
#9010=LINE('',#51278,#12060);
#9011=LINE('',#51280,#12061);
#9012=LINE('',#51281,#12062);
#9013=LINE('',#51283,#12063);
#9014=LINE('',#51284,#12064);
#9015=LINE('',#51286,#12065);
#9016=LINE('',#51287,#12066);
#9017=LINE('',#51289,#12067);
#9018=LINE('',#51290,#12068);
#9019=LINE('',#51292,#12069);
#9020=LINE('',#51293,#12070);
#9021=LINE('',#51300,#12071);
#9022=LINE('',#51302,#12072);
#9023=LINE('',#51303,#12073);
#9024=LINE('',#51307,#12074);
#9025=LINE('',#51308,#12075);
#9026=LINE('',#51310,#12076);
#9027=LINE('',#51311,#12077);
#9028=LINE('',#51313,#12078);
#9029=LINE('',#51314,#12079);
#9030=LINE('',#51318,#12080);
#9031=LINE('',#51320,#12081);
#9032=LINE('',#51321,#12082);
#9033=LINE('',#51325,#12083);
#9034=LINE('',#51326,#12084);
#9035=LINE('',#51328,#12085);
#9036=LINE('',#51329,#12086);
#9037=LINE('',#51331,#12087);
#9038=LINE('',#51332,#12088);
#9039=LINE('',#51334,#12089);
#9040=LINE('',#51335,#12090);
#9041=LINE('',#51338,#12091);
#9042=LINE('',#51339,#12092);
#9043=LINE('',#51340,#12093);
#9044=LINE('',#51342,#12094);
#9045=LINE('',#51345,#12095);
#9046=LINE('',#51346,#12096);
#9047=LINE('',#51348,#12097);
#9048=LINE('',#51349,#12098);
#9049=LINE('',#51355,#12099);
#9050=LINE('',#51357,#12100);
#9051=LINE('',#51358,#12101);
#9052=LINE('',#51362,#12102);
#9053=LINE('',#51364,#12103);
#9054=LINE('',#51365,#12104);
#9055=LINE('',#51369,#12105);
#9056=LINE('',#51371,#12106);
#9057=LINE('',#51372,#12107);
#9058=LINE('',#51374,#12108);
#9059=LINE('',#51375,#12109);
#9060=LINE('',#51379,#12110);
#9061=LINE('',#51381,#12111);
#9062=LINE('',#51382,#12112);
#9063=LINE('',#51384,#12113);
#9064=LINE('',#51385,#12114);
#9065=LINE('',#51387,#12115);
#9066=LINE('',#51388,#12116);
#9067=LINE('',#51390,#12117);
#9068=LINE('',#51391,#12118);
#9069=LINE('',#51393,#12119);
#9070=LINE('',#51394,#12120);
#9071=LINE('',#51396,#12121);
#9072=LINE('',#51397,#12122);
#9073=LINE('',#51399,#12123);
#9074=LINE('',#51400,#12124);
#9075=LINE('',#51402,#12125);
#9076=LINE('',#51403,#12126);
#9077=LINE('',#51410,#12127);
#9078=LINE('',#51412,#12128);
#9079=LINE('',#51413,#12129);
#9080=LINE('',#51417,#12130);
#9081=LINE('',#51419,#12131);
#9082=LINE('',#51420,#12132);
#9083=LINE('',#51424,#12133);
#9084=LINE('',#51426,#12134);
#9085=LINE('',#51427,#12135);
#9086=LINE('',#51429,#12136);
#9087=LINE('',#51430,#12137);
#9088=LINE('',#51434,#12138);
#9089=LINE('',#51436,#12139);
#9090=LINE('',#51437,#12140);
#9091=LINE('',#51439,#12141);
#9092=LINE('',#51440,#12142);
#9093=LINE('',#51442,#12143);
#9094=LINE('',#51443,#12144);
#9095=LINE('',#51445,#12145);
#9096=LINE('',#51446,#12146);
#9097=LINE('',#51448,#12147);
#9098=LINE('',#51449,#12148);
#9099=LINE('',#51451,#12149);
#9100=LINE('',#51452,#12150);
#9101=LINE('',#51454,#12151);
#9102=LINE('',#51455,#12152);
#9103=LINE('',#51457,#12153);
#9104=LINE('',#51458,#12154);
#9105=LINE('',#51465,#12155);
#9106=LINE('',#51466,#12156);
#9107=LINE('',#51468,#12157);
#9108=LINE('',#51469,#12158);
#9109=LINE('',#51472,#12159);
#9110=LINE('',#51473,#12160);
#9111=LINE('',#51476,#12161);
#9112=LINE('',#51478,#12162);
#9113=LINE('',#51479,#12163);
#9114=LINE('',#51482,#12164);
#9115=LINE('',#51484,#12165);
#9116=LINE('',#51485,#12166);
#9117=LINE('',#51488,#12167);
#9118=LINE('',#51489,#12168);
#9119=LINE('',#51492,#12169);
#9120=LINE('',#51493,#12170);
#9121=LINE('',#51495,#12171);
#9122=LINE('',#51496,#12172);
#9123=LINE('',#51500,#12173);
#9124=LINE('',#51502,#12174);
#9125=LINE('',#51503,#12175);
#9126=LINE('',#51505,#12176);
#9127=LINE('',#51506,#12177);
#9128=LINE('',#51508,#12178);
#9129=LINE('',#51509,#12179);
#9130=LINE('',#51511,#12180);
#9131=LINE('',#51512,#12181);
#9132=LINE('',#51514,#12182);
#9133=LINE('',#51520,#12183);
#9134=LINE('',#51522,#12184);
#9135=LINE('',#51523,#12185);
#9136=LINE('',#51527,#12186);
#9137=LINE('',#51529,#12187);
#9138=LINE('',#51530,#12188);
#9139=LINE('',#51534,#12189);
#9140=LINE('',#51536,#12190);
#9141=LINE('',#51537,#12191);
#9142=LINE('',#51539,#12192);
#9143=LINE('',#51540,#12193);
#9144=LINE('',#51544,#12194);
#9145=LINE('',#51546,#12195);
#9146=LINE('',#51547,#12196);
#9147=LINE('',#51549,#12197);
#9148=LINE('',#51550,#12198);
#9149=LINE('',#51552,#12199);
#9150=LINE('',#51553,#12200);
#9151=LINE('',#51555,#12201);
#9152=LINE('',#51556,#12202);
#9153=LINE('',#51558,#12203);
#9154=LINE('',#51559,#12204);
#9155=LINE('',#51561,#12205);
#9156=LINE('',#51562,#12206);
#9157=LINE('',#51564,#12207);
#9158=LINE('',#51565,#12208);
#9159=LINE('',#51567,#12209);
#9160=LINE('',#51568,#12210);
#9161=LINE('',#51575,#12211);
#9162=LINE('',#51577,#12212);
#9163=LINE('',#51578,#12213);
#9164=LINE('',#51582,#12214);
#9165=LINE('',#51583,#12215);
#9166=LINE('',#51585,#12216);
#9167=LINE('',#51586,#12217);
#9168=LINE('',#51588,#12218);
#9169=LINE('',#51589,#12219);
#9170=LINE('',#51593,#12220);
#9171=LINE('',#51595,#12221);
#9172=LINE('',#51596,#12222);
#9173=LINE('',#51600,#12223);
#9174=LINE('',#51601,#12224);
#9175=LINE('',#51603,#12225);
#9176=LINE('',#51604,#12226);
#9177=LINE('',#51606,#12227);
#9178=LINE('',#51607,#12228);
#9179=LINE('',#51609,#12229);
#9180=LINE('',#51610,#12230);
#9181=LINE('',#51613,#12231);
#9182=LINE('',#51614,#12232);
#9183=LINE('',#51615,#12233);
#9184=LINE('',#51617,#12234);
#9185=LINE('',#51620,#12235);
#9186=LINE('',#51621,#12236);
#9187=LINE('',#51623,#12237);
#9188=LINE('',#51624,#12238);
#9189=LINE('',#51630,#12239);
#9190=LINE('',#51632,#12240);
#9191=LINE('',#51633,#12241);
#9192=LINE('',#51637,#12242);
#9193=LINE('',#51639,#12243);
#9194=LINE('',#51640,#12244);
#9195=LINE('',#51644,#12245);
#9196=LINE('',#51646,#12246);
#9197=LINE('',#51647,#12247);
#9198=LINE('',#51649,#12248);
#9199=LINE('',#51650,#12249);
#9200=LINE('',#51654,#12250);
#9201=LINE('',#51656,#12251);
#9202=LINE('',#51657,#12252);
#9203=LINE('',#51659,#12253);
#9204=LINE('',#51660,#12254);
#9205=LINE('',#51662,#12255);
#9206=LINE('',#51663,#12256);
#9207=LINE('',#51665,#12257);
#9208=LINE('',#51666,#12258);
#9209=LINE('',#51668,#12259);
#9210=LINE('',#51669,#12260);
#9211=LINE('',#51671,#12261);
#9212=LINE('',#51672,#12262);
#9213=LINE('',#51674,#12263);
#9214=LINE('',#51675,#12264);
#9215=LINE('',#51677,#12265);
#9216=LINE('',#51678,#12266);
#9217=LINE('',#51685,#12267);
#9218=LINE('',#51687,#12268);
#9219=LINE('',#51688,#12269);
#9220=LINE('',#51692,#12270);
#9221=LINE('',#51694,#12271);
#9222=LINE('',#51695,#12272);
#9223=LINE('',#51699,#12273);
#9224=LINE('',#51701,#12274);
#9225=LINE('',#51702,#12275);
#9226=LINE('',#51704,#12276);
#9227=LINE('',#51705,#12277);
#9228=LINE('',#51709,#12278);
#9229=LINE('',#51711,#12279);
#9230=LINE('',#51712,#12280);
#9231=LINE('',#51714,#12281);
#9232=LINE('',#51715,#12282);
#9233=LINE('',#51717,#12283);
#9234=LINE('',#51718,#12284);
#9235=LINE('',#51720,#12285);
#9236=LINE('',#51721,#12286);
#9237=LINE('',#51723,#12287);
#9238=LINE('',#51724,#12288);
#9239=LINE('',#51726,#12289);
#9240=LINE('',#51727,#12290);
#9241=LINE('',#51729,#12291);
#9242=LINE('',#51730,#12292);
#9243=LINE('',#51732,#12293);
#9244=LINE('',#51733,#12294);
#9245=LINE('',#51740,#12295);
#9246=LINE('',#51741,#12296);
#9247=LINE('',#51743,#12297);
#9248=LINE('',#51744,#12298);
#9249=LINE('',#51747,#12299);
#9250=LINE('',#51748,#12300);
#9251=LINE('',#51751,#12301);
#9252=LINE('',#51753,#12302);
#9253=LINE('',#51754,#12303);
#9254=LINE('',#51757,#12304);
#9255=LINE('',#51759,#12305);
#9256=LINE('',#51760,#12306);
#9257=LINE('',#51763,#12307);
#9258=LINE('',#51764,#12308);
#9259=LINE('',#51767,#12309);
#9260=LINE('',#51768,#12310);
#9261=LINE('',#51770,#12311);
#9262=LINE('',#51771,#12312);
#9263=LINE('',#51775,#12313);
#9264=LINE('',#51777,#12314);
#9265=LINE('',#51778,#12315);
#9266=LINE('',#51780,#12316);
#9267=LINE('',#51781,#12317);
#9268=LINE('',#51783,#12318);
#9269=LINE('',#51784,#12319);
#9270=LINE('',#51786,#12320);
#9271=LINE('',#51787,#12321);
#9272=LINE('',#51789,#12322);
#9273=LINE('',#51795,#12323);
#9274=LINE('',#51797,#12324);
#9275=LINE('',#51798,#12325);
#9276=LINE('',#51802,#12326);
#9277=LINE('',#51804,#12327);
#9278=LINE('',#51805,#12328);
#9279=LINE('',#51809,#12329);
#9280=LINE('',#51811,#12330);
#9281=LINE('',#51812,#12331);
#9282=LINE('',#51814,#12332);
#9283=LINE('',#51815,#12333);
#9284=LINE('',#51819,#12334);
#9285=LINE('',#51821,#12335);
#9286=LINE('',#51822,#12336);
#9287=LINE('',#51824,#12337);
#9288=LINE('',#51825,#12338);
#9289=LINE('',#51827,#12339);
#9290=LINE('',#51828,#12340);
#9291=LINE('',#51830,#12341);
#9292=LINE('',#51831,#12342);
#9293=LINE('',#51833,#12343);
#9294=LINE('',#51834,#12344);
#9295=LINE('',#51836,#12345);
#9296=LINE('',#51837,#12346);
#9297=LINE('',#51839,#12347);
#9298=LINE('',#51840,#12348);
#9299=LINE('',#51842,#12349);
#9300=LINE('',#51843,#12350);
#9301=LINE('',#51850,#12351);
#9302=LINE('',#51852,#12352);
#9303=LINE('',#51853,#12353);
#9304=LINE('',#51857,#12354);
#9305=LINE('',#51858,#12355);
#9306=LINE('',#51860,#12356);
#9307=LINE('',#51861,#12357);
#9308=LINE('',#51863,#12358);
#9309=LINE('',#51864,#12359);
#9310=LINE('',#51868,#12360);
#9311=LINE('',#51870,#12361);
#9312=LINE('',#51871,#12362);
#9313=LINE('',#51875,#12363);
#9314=LINE('',#51876,#12364);
#9315=LINE('',#51878,#12365);
#9316=LINE('',#51879,#12366);
#9317=LINE('',#51881,#12367);
#9318=LINE('',#51882,#12368);
#9319=LINE('',#51884,#12369);
#9320=LINE('',#51885,#12370);
#9321=LINE('',#51888,#12371);
#9322=LINE('',#51889,#12372);
#9323=LINE('',#51890,#12373);
#9324=LINE('',#51892,#12374);
#9325=LINE('',#51895,#12375);
#9326=LINE('',#51896,#12376);
#9327=LINE('',#51898,#12377);
#9328=LINE('',#51899,#12378);
#9329=LINE('',#51905,#12379);
#9330=LINE('',#51907,#12380);
#9331=LINE('',#51908,#12381);
#9332=LINE('',#51912,#12382);
#9333=LINE('',#51914,#12383);
#9334=LINE('',#51915,#12384);
#9335=LINE('',#51919,#12385);
#9336=LINE('',#51921,#12386);
#9337=LINE('',#51922,#12387);
#9338=LINE('',#51924,#12388);
#9339=LINE('',#51925,#12389);
#9340=LINE('',#51929,#12390);
#9341=LINE('',#51931,#12391);
#9342=LINE('',#51932,#12392);
#9343=LINE('',#51934,#12393);
#9344=LINE('',#51935,#12394);
#9345=LINE('',#51937,#12395);
#9346=LINE('',#51938,#12396);
#9347=LINE('',#51940,#12397);
#9348=LINE('',#51941,#12398);
#9349=LINE('',#51943,#12399);
#9350=LINE('',#51944,#12400);
#9351=LINE('',#51946,#12401);
#9352=LINE('',#51947,#12402);
#9353=LINE('',#51949,#12403);
#9354=LINE('',#51950,#12404);
#9355=LINE('',#51952,#12405);
#9356=LINE('',#51953,#12406);
#9357=LINE('',#51960,#12407);
#9358=LINE('',#51962,#12408);
#9359=LINE('',#51963,#12409);
#9360=LINE('',#51967,#12410);
#9361=LINE('',#51969,#12411);
#9362=LINE('',#51970,#12412);
#9363=LINE('',#51974,#12413);
#9364=LINE('',#51976,#12414);
#9365=LINE('',#51977,#12415);
#9366=LINE('',#51979,#12416);
#9367=LINE('',#51980,#12417);
#9368=LINE('',#51984,#12418);
#9369=LINE('',#51986,#12419);
#9370=LINE('',#51987,#12420);
#9371=LINE('',#51989,#12421);
#9372=LINE('',#51990,#12422);
#9373=LINE('',#51992,#12423);
#9374=LINE('',#51993,#12424);
#9375=LINE('',#51995,#12425);
#9376=LINE('',#51996,#12426);
#9377=LINE('',#51998,#12427);
#9378=LINE('',#51999,#12428);
#9379=LINE('',#52001,#12429);
#9380=LINE('',#52002,#12430);
#9381=LINE('',#52004,#12431);
#9382=LINE('',#52005,#12432);
#9383=LINE('',#52007,#12433);
#9384=LINE('',#52008,#12434);
#9385=LINE('',#52015,#12435);
#9386=LINE('',#52016,#12436);
#9387=LINE('',#52018,#12437);
#9388=LINE('',#52019,#12438);
#9389=LINE('',#52022,#12439);
#9390=LINE('',#52023,#12440);
#9391=LINE('',#52026,#12441);
#9392=LINE('',#52028,#12442);
#9393=LINE('',#52029,#12443);
#9394=LINE('',#52032,#12444);
#9395=LINE('',#52034,#12445);
#9396=LINE('',#52035,#12446);
#9397=LINE('',#52038,#12447);
#9398=LINE('',#52039,#12448);
#9399=LINE('',#52042,#12449);
#9400=LINE('',#52043,#12450);
#9401=LINE('',#52045,#12451);
#9402=LINE('',#52046,#12452);
#9403=LINE('',#52050,#12453);
#9404=LINE('',#52052,#12454);
#9405=LINE('',#52053,#12455);
#9406=LINE('',#52055,#12456);
#9407=LINE('',#52056,#12457);
#9408=LINE('',#52058,#12458);
#9409=LINE('',#52059,#12459);
#9410=LINE('',#52061,#12460);
#9411=LINE('',#52062,#12461);
#9412=LINE('',#52064,#12462);
#9413=LINE('',#52070,#12463);
#9414=LINE('',#52072,#12464);
#9415=LINE('',#52073,#12465);
#9416=LINE('',#52077,#12466);
#9417=LINE('',#52079,#12467);
#9418=LINE('',#52080,#12468);
#9419=LINE('',#52084,#12469);
#9420=LINE('',#52086,#12470);
#9421=LINE('',#52087,#12471);
#9422=LINE('',#52089,#12472);
#9423=LINE('',#52090,#12473);
#9424=LINE('',#52094,#12474);
#9425=LINE('',#52096,#12475);
#9426=LINE('',#52097,#12476);
#9427=LINE('',#52099,#12477);
#9428=LINE('',#52100,#12478);
#9429=LINE('',#52102,#12479);
#9430=LINE('',#52103,#12480);
#9431=LINE('',#52105,#12481);
#9432=LINE('',#52106,#12482);
#9433=LINE('',#52108,#12483);
#9434=LINE('',#52109,#12484);
#9435=LINE('',#52111,#12485);
#9436=LINE('',#52112,#12486);
#9437=LINE('',#52114,#12487);
#9438=LINE('',#52115,#12488);
#9439=LINE('',#52117,#12489);
#9440=LINE('',#52118,#12490);
#9441=LINE('',#52125,#12491);
#9442=LINE('',#52127,#12492);
#9443=LINE('',#52128,#12493);
#9444=LINE('',#52132,#12494);
#9445=LINE('',#52133,#12495);
#9446=LINE('',#52135,#12496);
#9447=LINE('',#52136,#12497);
#9448=LINE('',#52138,#12498);
#9449=LINE('',#52139,#12499);
#9450=LINE('',#52143,#12500);
#9451=LINE('',#52145,#12501);
#9452=LINE('',#52146,#12502);
#9453=LINE('',#52150,#12503);
#9454=LINE('',#52151,#12504);
#9455=LINE('',#52153,#12505);
#9456=LINE('',#52154,#12506);
#9457=LINE('',#52156,#12507);
#9458=LINE('',#52157,#12508);
#9459=LINE('',#52159,#12509);
#9460=LINE('',#52160,#12510);
#9461=LINE('',#52163,#12511);
#9462=LINE('',#52164,#12512);
#9463=LINE('',#52165,#12513);
#9464=LINE('',#52167,#12514);
#9465=LINE('',#52170,#12515);
#9466=LINE('',#52171,#12516);
#9467=LINE('',#52173,#12517);
#9468=LINE('',#52174,#12518);
#9469=LINE('',#52180,#12519);
#9470=LINE('',#52182,#12520);
#9471=LINE('',#52183,#12521);
#9472=LINE('',#52187,#12522);
#9473=LINE('',#52189,#12523);
#9474=LINE('',#52190,#12524);
#9475=LINE('',#52194,#12525);
#9476=LINE('',#52196,#12526);
#9477=LINE('',#52197,#12527);
#9478=LINE('',#52199,#12528);
#9479=LINE('',#52200,#12529);
#9480=LINE('',#52204,#12530);
#9481=LINE('',#52206,#12531);
#9482=LINE('',#52207,#12532);
#9483=LINE('',#52209,#12533);
#9484=LINE('',#52210,#12534);
#9485=LINE('',#52212,#12535);
#9486=LINE('',#52213,#12536);
#9487=LINE('',#52215,#12537);
#9488=LINE('',#52216,#12538);
#9489=LINE('',#52218,#12539);
#9490=LINE('',#52219,#12540);
#9491=LINE('',#52221,#12541);
#9492=LINE('',#52222,#12542);
#9493=LINE('',#52224,#12543);
#9494=LINE('',#52225,#12544);
#9495=LINE('',#52227,#12545);
#9496=LINE('',#52228,#12546);
#9497=LINE('',#52235,#12547);
#9498=LINE('',#52237,#12548);
#9499=LINE('',#52238,#12549);
#9500=LINE('',#52242,#12550);
#9501=LINE('',#52244,#12551);
#9502=LINE('',#52245,#12552);
#9503=LINE('',#52249,#12553);
#9504=LINE('',#52251,#12554);
#9505=LINE('',#52252,#12555);
#9506=LINE('',#52254,#12556);
#9507=LINE('',#52255,#12557);
#9508=LINE('',#52259,#12558);
#9509=LINE('',#52261,#12559);
#9510=LINE('',#52262,#12560);
#9511=LINE('',#52264,#12561);
#9512=LINE('',#52265,#12562);
#9513=LINE('',#52267,#12563);
#9514=LINE('',#52268,#12564);
#9515=LINE('',#52270,#12565);
#9516=LINE('',#52271,#12566);
#9517=LINE('',#52273,#12567);
#9518=LINE('',#52274,#12568);
#9519=LINE('',#52276,#12569);
#9520=LINE('',#52277,#12570);
#9521=LINE('',#52279,#12571);
#9522=LINE('',#52280,#12572);
#9523=LINE('',#52282,#12573);
#9524=LINE('',#52283,#12574);
#9525=LINE('',#52290,#12575);
#9526=LINE('',#52291,#12576);
#9527=LINE('',#52293,#12577);
#9528=LINE('',#52294,#12578);
#9529=LINE('',#52297,#12579);
#9530=LINE('',#52298,#12580);
#9531=LINE('',#52301,#12581);
#9532=LINE('',#52303,#12582);
#9533=LINE('',#52304,#12583);
#9534=LINE('',#52307,#12584);
#9535=LINE('',#52309,#12585);
#9536=LINE('',#52310,#12586);
#9537=LINE('',#52313,#12587);
#9538=LINE('',#52314,#12588);
#9539=LINE('',#52317,#12589);
#9540=LINE('',#52318,#12590);
#9541=LINE('',#52320,#12591);
#9542=LINE('',#52321,#12592);
#9543=LINE('',#52325,#12593);
#9544=LINE('',#52327,#12594);
#9545=LINE('',#52328,#12595);
#9546=LINE('',#52330,#12596);
#9547=LINE('',#52331,#12597);
#9548=LINE('',#52333,#12598);
#9549=LINE('',#52334,#12599);
#9550=LINE('',#52336,#12600);
#9551=LINE('',#52337,#12601);
#9552=LINE('',#52339,#12602);
#9553=LINE('',#52345,#12603);
#9554=LINE('',#52347,#12604);
#9555=LINE('',#52348,#12605);
#9556=LINE('',#52352,#12606);
#9557=LINE('',#52354,#12607);
#9558=LINE('',#52355,#12608);
#9559=LINE('',#52359,#12609);
#9560=LINE('',#52361,#12610);
#9561=LINE('',#52362,#12611);
#9562=LINE('',#52364,#12612);
#9563=LINE('',#52365,#12613);
#9564=LINE('',#52369,#12614);
#9565=LINE('',#52371,#12615);
#9566=LINE('',#52372,#12616);
#9567=LINE('',#52374,#12617);
#9568=LINE('',#52375,#12618);
#9569=LINE('',#52377,#12619);
#9570=LINE('',#52378,#12620);
#9571=LINE('',#52380,#12621);
#9572=LINE('',#52381,#12622);
#9573=LINE('',#52383,#12623);
#9574=LINE('',#52384,#12624);
#9575=LINE('',#52386,#12625);
#9576=LINE('',#52387,#12626);
#9577=LINE('',#52389,#12627);
#9578=LINE('',#52390,#12628);
#9579=LINE('',#52392,#12629);
#9580=LINE('',#52393,#12630);
#9581=LINE('',#52400,#12631);
#9582=LINE('',#52402,#12632);
#9583=LINE('',#52403,#12633);
#9584=LINE('',#52407,#12634);
#9585=LINE('',#52408,#12635);
#9586=LINE('',#52410,#12636);
#9587=LINE('',#52411,#12637);
#9588=LINE('',#52413,#12638);
#9589=LINE('',#52414,#12639);
#9590=LINE('',#52418,#12640);
#9591=LINE('',#52420,#12641);
#9592=LINE('',#52421,#12642);
#9593=LINE('',#52425,#12643);
#9594=LINE('',#52426,#12644);
#9595=LINE('',#52428,#12645);
#9596=LINE('',#52429,#12646);
#9597=LINE('',#52431,#12647);
#9598=LINE('',#52432,#12648);
#9599=LINE('',#52434,#12649);
#9600=LINE('',#52435,#12650);
#9601=LINE('',#52438,#12651);
#9602=LINE('',#52439,#12652);
#9603=LINE('',#52440,#12653);
#9604=LINE('',#52442,#12654);
#9605=LINE('',#52445,#12655);
#9606=LINE('',#52446,#12656);
#9607=LINE('',#52448,#12657);
#9608=LINE('',#52449,#12658);
#9609=LINE('',#52455,#12659);
#9610=LINE('',#52457,#12660);
#9611=LINE('',#52458,#12661);
#9612=LINE('',#52462,#12662);
#9613=LINE('',#52464,#12663);
#9614=LINE('',#52465,#12664);
#9615=LINE('',#52469,#12665);
#9616=LINE('',#52471,#12666);
#9617=LINE('',#52472,#12667);
#9618=LINE('',#52474,#12668);
#9619=LINE('',#52475,#12669);
#9620=LINE('',#52479,#12670);
#9621=LINE('',#52481,#12671);
#9622=LINE('',#52482,#12672);
#9623=LINE('',#52484,#12673);
#9624=LINE('',#52485,#12674);
#9625=LINE('',#52487,#12675);
#9626=LINE('',#52488,#12676);
#9627=LINE('',#52490,#12677);
#9628=LINE('',#52491,#12678);
#9629=LINE('',#52493,#12679);
#9630=LINE('',#52494,#12680);
#9631=LINE('',#52496,#12681);
#9632=LINE('',#52497,#12682);
#9633=LINE('',#52499,#12683);
#9634=LINE('',#52500,#12684);
#9635=LINE('',#52502,#12685);
#9636=LINE('',#52503,#12686);
#9637=LINE('',#52510,#12687);
#9638=LINE('',#52512,#12688);
#9639=LINE('',#52513,#12689);
#9640=LINE('',#52517,#12690);
#9641=LINE('',#52519,#12691);
#9642=LINE('',#52520,#12692);
#9643=LINE('',#52524,#12693);
#9644=LINE('',#52526,#12694);
#9645=LINE('',#52527,#12695);
#9646=LINE('',#52529,#12696);
#9647=LINE('',#52530,#12697);
#9648=LINE('',#52534,#12698);
#9649=LINE('',#52536,#12699);
#9650=LINE('',#52537,#12700);
#9651=LINE('',#52539,#12701);
#9652=LINE('',#52540,#12702);
#9653=LINE('',#52542,#12703);
#9654=LINE('',#52543,#12704);
#9655=LINE('',#52545,#12705);
#9656=LINE('',#52546,#12706);
#9657=LINE('',#52548,#12707);
#9658=LINE('',#52549,#12708);
#9659=LINE('',#52551,#12709);
#9660=LINE('',#52552,#12710);
#9661=LINE('',#52554,#12711);
#9662=LINE('',#52555,#12712);
#9663=LINE('',#52557,#12713);
#9664=LINE('',#52558,#12714);
#9665=LINE('',#52568,#12715);
#9666=LINE('',#52574,#12716);
#9667=LINE('',#52581,#12717);
#9668=LINE('',#52585,#12718);
#9669=LINE('',#52587,#12719);
#9670=LINE('',#52588,#12720);
#9671=LINE('',#52592,#12721);
#9672=LINE('',#52594,#12722);
#9673=LINE('',#52595,#12723);
#9674=LINE('',#52599,#12724);
#9675=LINE('',#52601,#12725);
#9676=LINE('',#52602,#12726);
#9677=LINE('',#52604,#12727);
#9678=LINE('',#52605,#12728);
#9679=LINE('',#52609,#12729);
#9680=LINE('',#52611,#12730);
#9681=LINE('',#52612,#12731);
#9682=LINE('',#52614,#12732);
#9683=LINE('',#52615,#12733);
#9684=LINE('',#52617,#12734);
#9685=LINE('',#52618,#12735);
#9686=LINE('',#52620,#12736);
#9687=LINE('',#52621,#12737);
#9688=LINE('',#52623,#12738);
#9689=LINE('',#52624,#12739);
#9690=LINE('',#52626,#12740);
#9691=LINE('',#52627,#12741);
#9692=LINE('',#52629,#12742);
#9693=LINE('',#52630,#12743);
#9694=LINE('',#52632,#12744);
#9695=LINE('',#52633,#12745);
#9696=LINE('',#52640,#12746);
#9697=LINE('',#52642,#12747);
#9698=LINE('',#52643,#12748);
#9699=LINE('',#52647,#12749);
#9700=LINE('',#52649,#12750);
#9701=LINE('',#52650,#12751);
#9702=LINE('',#52654,#12752);
#9703=LINE('',#52656,#12753);
#9704=LINE('',#52657,#12754);
#9705=LINE('',#52659,#12755);
#9706=LINE('',#52660,#12756);
#9707=LINE('',#52664,#12757);
#9708=LINE('',#52666,#12758);
#9709=LINE('',#52667,#12759);
#9710=LINE('',#52669,#12760);
#9711=LINE('',#52670,#12761);
#9712=LINE('',#52672,#12762);
#9713=LINE('',#52673,#12763);
#9714=LINE('',#52675,#12764);
#9715=LINE('',#52676,#12765);
#9716=LINE('',#52678,#12766);
#9717=LINE('',#52679,#12767);
#9718=LINE('',#52681,#12768);
#9719=LINE('',#52682,#12769);
#9720=LINE('',#52684,#12770);
#9721=LINE('',#52685,#12771);
#9722=LINE('',#52687,#12772);
#9723=LINE('',#52688,#12773);
#9724=LINE('',#52698,#12774);
#9725=LINE('',#52704,#12775);
#9726=LINE('',#52709,#12776);
#9727=LINE('',#52713,#12777);
#9728=LINE('',#52720,#12778);
#9729=LINE('',#52723,#12779);
#9730=LINE('',#52726,#12780);
#9731=LINE('',#52873,#12781);
#9732=LINE('',#52877,#12782);
#9733=LINE('',#52881,#12783);
#9734=LINE('',#52885,#12784);
#9735=LINE('',#52889,#12785);
#9736=LINE('',#52895,#12786);
#9737=LINE('',#52899,#12787);
#9738=LINE('',#52903,#12788);
#9739=LINE('',#52907,#12789);
#9740=LINE('',#52911,#12790);
#9741=LINE('',#52918,#12791);
#9742=LINE('',#52923,#12792);
#9743=LINE('',#52928,#12793);
#9744=LINE('',#52935,#12794);
#9745=LINE('',#52938,#12795);
#9746=LINE('',#52942,#12796);
#9747=LINE('',#52948,#12797);
#9748=LINE('',#52951,#12798);
#9749=LINE('',#52956,#12799);
#9750=LINE('',#53010,#12800);
#9751=LINE('',#53047,#12801);
#9752=LINE('',#53085,#12802);
#9753=LINE('',#53123,#12803);
#9754=LINE('',#53160,#12804);
#9755=LINE('',#53197,#12805);
#9756=LINE('',#53231,#12806);
#9757=LINE('',#53269,#12807);
#9758=LINE('',#53307,#12808);
#9759=LINE('',#53311,#12809);
#9760=LINE('',#53318,#12810);
#9761=LINE('',#53320,#12811);
#9762=LINE('',#53322,#12812);
#9763=LINE('',#53323,#12813);
#9764=LINE('',#53326,#12814);
#9765=LINE('',#53328,#12815);
#9766=LINE('',#53329,#12816);
#9767=LINE('',#53333,#12817);
#9768=LINE('',#53335,#12818);
#9769=LINE('',#53337,#12819);
#9770=LINE('',#53339,#12820);
#9771=LINE('',#53341,#12821);
#9772=LINE('',#53342,#12822);
#9773=LINE('',#53345,#12823);
#9774=LINE('',#53347,#12824);
#9775=LINE('',#53348,#12825);
#9776=LINE('',#53351,#12826);
#9777=LINE('',#53353,#12827);
#9778=LINE('',#53354,#12828);
#9779=LINE('',#53357,#12829);
#9780=LINE('',#53359,#12830);
#9781=LINE('',#53361,#12831);
#9782=LINE('',#53362,#12832);
#9783=LINE('',#53366,#12833);
#9784=LINE('',#53368,#12834);
#9785=LINE('',#53369,#12835);
#9786=LINE('',#53371,#12836);
#9787=LINE('',#53373,#12837);
#9788=LINE('',#53374,#12838);
#9789=LINE('',#53377,#12839);
#9790=LINE('',#53378,#12840);
#9791=LINE('',#53379,#12841);
#9792=LINE('',#53383,#12842);
#9793=LINE('',#53385,#12843);
#9794=LINE('',#53386,#12844);
#9795=LINE('',#53390,#12845);
#9796=LINE('',#53391,#12846);
#9797=LINE('',#53393,#12847);
#9798=LINE('',#53394,#12848);
#9799=LINE('',#53396,#12849);
#9800=LINE('',#53397,#12850);
#9801=LINE('',#53401,#12851);
#9802=LINE('',#53403,#12852);
#9803=LINE('',#53404,#12853);
#9804=LINE('',#53408,#12854);
#9805=LINE('',#53409,#12855);
#9806=LINE('',#53411,#12856);
#9807=LINE('',#53412,#12857);
#9808=LINE('',#53414,#12858);
#9809=LINE('',#53415,#12859);
#9810=LINE('',#53419,#12860);
#9811=LINE('',#53421,#12861);
#9812=LINE('',#53422,#12862);
#9813=LINE('',#53426,#12863);
#9814=LINE('',#53427,#12864);
#9815=LINE('',#53429,#12865);
#9816=LINE('',#53430,#12866);
#9817=LINE('',#53432,#12867);
#9818=LINE('',#53433,#12868);
#9819=LINE('',#53437,#12869);
#9820=LINE('',#53439,#12870);
#9821=LINE('',#53440,#12871);
#9822=LINE('',#53444,#12872);
#9823=LINE('',#53445,#12873);
#9824=LINE('',#53447,#12874);
#9825=LINE('',#53448,#12875);
#9826=LINE('',#53450,#12876);
#9827=LINE('',#53451,#12877);
#9828=LINE('',#53455,#12878);
#9829=LINE('',#53457,#12879);
#9830=LINE('',#53458,#12880);
#9831=LINE('',#53462,#12881);
#9832=LINE('',#53463,#12882);
#9833=LINE('',#53465,#12883);
#9834=LINE('',#53466,#12884);
#9835=LINE('',#53468,#12885);
#9836=LINE('',#53469,#12886);
#9837=LINE('',#53473,#12887);
#9838=LINE('',#53474,#12888);
#9839=LINE('',#53476,#12889);
#9840=LINE('',#53477,#12890);
#9841=LINE('',#53480,#12891);
#9842=LINE('',#53482,#12892);
#9843=LINE('',#53483,#12893);
#9844=LINE('',#53484,#12894);
#9845=LINE('',#53486,#12895);
#9846=LINE('',#53489,#12896);
#9847=LINE('',#53490,#12897);
#9848=LINE('',#53492,#12898);
#9849=LINE('',#53495,#12899);
#9850=LINE('',#53496,#12900);
#9851=LINE('',#53498,#12901);
#9852=LINE('',#53501,#12902);
#9853=LINE('',#53502,#12903);
#9854=LINE('',#53505,#12904);
#9855=LINE('',#53506,#12905);
#9856=LINE('',#53507,#12906);
#9857=LINE('',#53509,#12907);
#9858=LINE('',#53511,#12908);
#9859=LINE('',#53512,#12909);
#9860=LINE('',#53517,#12910);
#9861=LINE('',#53520,#12911);
#9862=LINE('',#53532,#12912);
#9863=LINE('',#53535,#12913);
#9864=LINE('',#53540,#12914);
#9865=LINE('',#53543,#12915);
#9866=LINE('',#53548,#12916);
#9867=LINE('',#53551,#12917);
#9868=LINE('',#53556,#12918);
#9869=LINE('',#53560,#12919);
#9870=LINE('',#53562,#12920);
#9871=LINE('',#53572,#12921);
#9872=LINE('',#53574,#12922);
#9873=LINE('',#53576,#12923);
#9874=LINE('',#53578,#12924);
#9875=LINE('',#53590,#12925);
#9876=LINE('',#53596,#12926);
#9877=LINE('',#53601,#12927);
#9878=LINE('',#53604,#12928);
#9879=LINE('',#57693,#12929);
#9880=LINE('',#57787,#12930);
#9881=LINE('',#57789,#12931);
#9882=LINE('',#57790,#12932);
#9883=LINE('',#57792,#12933);
#9884=LINE('',#57793,#12934);
#9885=LINE('',#57795,#12935);
#9886=LINE('',#57796,#12936);
#9887=LINE('',#57798,#12937);
#9888=LINE('',#57799,#12938);
#9889=LINE('',#57801,#12939);
#9890=LINE('',#57802,#12940);
#9891=LINE('',#57804,#12941);
#9892=LINE('',#57805,#12942);
#9893=LINE('',#57807,#12943);
#9894=LINE('',#57808,#12944);
#9895=LINE('',#57810,#12945);
#9896=LINE('',#57811,#12946);
#9897=LINE('',#57814,#12947);
#9898=LINE('',#57819,#12948);
#9899=LINE('',#57822,#12949);
#9900=LINE('',#57823,#12950);
#9901=LINE('',#57883,#12951);
#9902=LINE('',#57891,#12952);
#9903=LINE('',#57895,#12953);
#9904=LINE('',#57902,#12954);
#9905=LINE('',#57906,#12955);
#9906=LINE('',#57910,#12956);
#9907=LINE('',#57914,#12957);
#9908=LINE('',#57919,#12958);
#9909=LINE('',#57920,#12959);
#9910=LINE('',#57923,#12960);
#9911=LINE('',#57924,#12961);
#9912=LINE('',#57927,#12962);
#9913=LINE('',#57930,#12963);
#9914=LINE('',#57933,#12964);
#9915=LINE('',#57940,#12965);
#9916=LINE('',#57945,#12966);
#9917=LINE('',#57947,#12967);
#9918=LINE('',#57957,#12968);
#9919=LINE('',#57964,#12969);
#9920=LINE('',#57970,#12970);
#9921=LINE('',#57980,#12971);
#9922=LINE('',#57993,#12972);
#9923=LINE('',#57997,#12973);
#9924=LINE('',#57999,#12974);
#9925=LINE('',#58002,#12975);
#9926=LINE('',#58006,#12976);
#9927=LINE('',#58010,#12977);
#9928=LINE('',#58013,#12978);
#9929=LINE('',#58020,#12979);
#9930=LINE('',#58025,#12980);
#9931=LINE('',#58029,#12981);
#9932=LINE('',#58035,#12982);
#9933=LINE('',#58039,#12983);
#9934=LINE('',#58043,#12984);
#9935=LINE('',#58053,#12985);
#9936=LINE('',#58061,#12986);
#9937=LINE('',#58066,#12987);
#9938=LINE('',#58072,#12988);
#9939=LINE('',#60057,#12989);
#9940=LINE('',#60060,#12990);
#9941=LINE('',#60061,#12991);
#9942=LINE('',#60065,#12992);
#9943=LINE('',#60071,#12993);
#9944=LINE('',#60075,#12994);
#9945=LINE('',#60079,#12995);
#9946=LINE('',#60087,#12996);
#9947=LINE('',#60092,#12997);
#9948=LINE('',#60096,#12998);
#9949=LINE('',#60102,#12999);
#9950=LINE('',#60106,#13000);
#9951=LINE('',#60110,#13001);
#9952=LINE('',#60120,#13002);
#9953=LINE('',#60128,#13003);
#9954=LINE('',#60133,#13004);
#9955=LINE('',#60139,#13005);
#9956=LINE('',#61900,#13006);
#9957=LINE('',#61903,#13007);
#9958=LINE('',#61904,#13008);
#9959=LINE('',#61908,#13009);
#9960=LINE('',#61914,#13010);
#9961=LINE('',#61918,#13011);
#9962=LINE('',#61922,#13012);
#9963=LINE('',#61929,#13013);
#9964=LINE('',#61931,#13014);
#9965=LINE('',#61933,#13015);
#9966=LINE('',#61934,#13016);
#9967=LINE('',#61937,#13017);
#9968=LINE('',#61939,#13018);
#9969=LINE('',#61941,#13019);
#9970=LINE('',#61943,#13020);
#9971=LINE('',#61944,#13021);
#9972=LINE('',#61947,#13022);
#9973=LINE('',#61948,#13023);
#9974=LINE('',#61951,#13024);
#9975=LINE('',#61952,#13025);
#9976=LINE('',#61955,#13026);
#9977=LINE('',#61957,#13027);
#9978=LINE('',#61958,#13028);
#9979=LINE('',#61971,#13029);
#9980=LINE('',#61975,#13030);
#9981=LINE('',#61977,#13031);
#9982=LINE('',#61986,#13032);
#9983=LINE('',#61992,#13033);
#9984=LINE('',#61993,#13034);
#9985=LINE('',#61998,#13035);
#9986=LINE('',#62026,#13036);
#9987=LINE('',#62032,#13037);
#9988=LINE('',#62034,#13038);
#9989=LINE('',#62035,#13039);
#9990=LINE('',#62038,#13040);
#9991=LINE('',#62039,#13041);
#9992=LINE('',#62042,#13042);
#9993=LINE('',#62044,#13043);
#9994=LINE('',#62045,#13044);
#9995=LINE('',#62048,#13045);
#9996=LINE('',#62050,#13046);
#9997=LINE('',#62052,#13047);
#9998=LINE('',#62054,#13048);
#9999=LINE('',#62055,#13049);
#10000=LINE('',#62058,#13050);
#10001=LINE('',#62064,#13051);
#10002=LINE('',#62065,#13052);
#10003=LINE('',#62068,#13053);
#10004=LINE('',#62070,#13054);
#10005=LINE('',#62074,#13055);
#10006=LINE('',#62076,#13056);
#10007=LINE('',#62078,#13057);
#10008=LINE('',#62079,#13058);
#10009=LINE('',#62085,#13059);
#10010=LINE('',#62101,#13060);
#10011=LINE('',#62103,#13061);
#10012=LINE('',#62109,#13062);
#10013=LINE('',#62110,#13063);
#10014=LINE('',#62113,#13064);
#10015=LINE('',#62115,#13065);
#10016=LINE('',#62121,#13066);
#10017=LINE('',#62123,#13067);
#10018=LINE('',#62125,#13068);
#10019=LINE('',#62131,#13069);
#10020=LINE('',#62133,#13070);
#10021=LINE('',#62135,#13071);
#10022=LINE('',#62136,#13072);
#10023=LINE('',#62138,#13073);
#10024=LINE('',#62139,#13074);
#10025=LINE('',#62147,#13075);
#10026=LINE('',#62153,#13076);
#10027=LINE('',#62154,#13077);
#10028=LINE('',#62176,#13078);
#10029=LINE('',#62202,#13079);
#10030=LINE('',#62203,#13080);
#10031=LINE('',#62206,#13081);
#10032=LINE('',#62211,#13082);
#10033=LINE('',#62218,#13083);
#10034=LINE('',#62220,#13084);
#10035=LINE('',#62221,#13085);
#10036=LINE('',#62226,#13086);
#10037=LINE('',#62267,#13087);
#10038=LINE('',#62273,#13088);
#10039=LINE('',#62274,#13089);
#10040=LINE('',#62279,#13090);
#10041=LINE('',#62307,#13091);
#10042=LINE('',#62313,#13092);
#10043=LINE('',#62315,#13093);
#10044=LINE('',#62316,#13094);
#10045=LINE('',#62319,#13095);
#10046=LINE('',#62320,#13096);
#10047=LINE('',#62323,#13097);
#10048=LINE('',#62325,#13098);
#10049=LINE('',#62326,#13099);
#10050=LINE('',#62328,#13100);
#10051=LINE('',#62329,#13101);
#10052=LINE('',#62332,#13102);
#10053=LINE('',#62333,#13103);
#10054=LINE('',#62336,#13104);
#10055=LINE('',#62337,#13105);
#10056=LINE('',#62339,#13106);
#10057=LINE('',#62342,#13107);
#10058=LINE('',#62344,#13108);
#10059=LINE('',#62345,#13109);
#10060=LINE('',#62348,#13110);
#10061=LINE('',#62349,#13111);
#10062=LINE('',#62352,#13112);
#10063=LINE('',#62353,#13113);
#10064=LINE('',#62356,#13114);
#10065=LINE('',#62358,#13115);
#10066=LINE('',#62360,#13116);
#10067=LINE('',#62361,#13117);
#10068=LINE('',#62364,#13118);
#10069=LINE('',#62370,#13119);
#10070=LINE('',#62371,#13120);
#10071=LINE('',#62374,#13121);
#10072=LINE('',#62376,#13122);
#10073=LINE('',#62380,#13123);
#10074=LINE('',#62382,#13124);
#10075=LINE('',#62384,#13125);
#10076=LINE('',#62385,#13126);
#10077=LINE('',#62391,#13127);
#10078=LINE('',#62406,#13128);
#10079=LINE('',#62408,#13129);
#10080=LINE('',#62410,#13130);
#10081=LINE('',#62412,#13131);
#10082=LINE('',#62413,#13132);
#10083=LINE('',#62416,#13133);
#10084=LINE('',#62417,#13134);
#10085=LINE('',#62420,#13135);
#10086=LINE('',#62448,#13136);
#10087=LINE('',#62454,#13137);
#10088=LINE('',#62455,#13138);
#10089=LINE('',#62460,#13139);
#10090=LINE('',#62462,#13140);
#10091=LINE('',#62468,#13141);
#10092=LINE('',#62470,#13142);
#10093=LINE('',#62471,#13143);
#10094=LINE('',#62474,#13144);
#10095=LINE('',#62476,#13145);
#10096=LINE('',#62477,#13146);
#10097=LINE('',#62483,#13147);
#10098=LINE('',#62486,#13148);
#10099=LINE('',#62492,#13149);
#10100=LINE('',#62494,#13150);
#10101=LINE('',#62499,#13151);
#10102=LINE('',#62502,#13152);
#10103=LINE('',#62504,#13153);
#10104=LINE('',#62509,#13154);
#10105=LINE('',#62512,#13155);
#10106=LINE('',#62517,#13156);
#10107=LINE('',#62531,#13157);
#10108=LINE('',#62533,#13158);
#10109=LINE('',#62534,#13159);
#10110=LINE('',#62538,#13160);
#10111=LINE('',#62545,#13161);
#10112=LINE('',#62556,#13162);
#10113=LINE('',#62559,#13163);
#10114=LINE('',#62565,#13164);
#10115=LINE('',#62568,#13165);
#10116=LINE('',#62579,#13166);
#10117=LINE('',#62583,#13167);
#10118=LINE('',#62585,#13168);
#10119=LINE('',#62591,#13169);
#10120=LINE('',#62610,#13170);
#10121=LINE('',#62616,#13171);
#10122=LINE('',#62626,#13172);
#10123=LINE('',#62635,#13173);
#10124=LINE('',#62639,#13174);
#10125=LINE('',#62643,#13175);
#10126=LINE('',#62647,#13176);
#10127=LINE('',#62665,#13177);
#10128=LINE('',#62670,#13178);
#10129=LINE('',#62673,#13179);
#10130=LINE('',#62678,#13180);
#10131=LINE('',#62680,#13181);
#10132=LINE('',#62704,#13182);
#10133=LINE('',#62706,#13183);
#10134=LINE('',#62707,#13184);
#10135=LINE('',#62709,#13185);
#10136=LINE('',#62714,#13186);
#10137=LINE('',#62721,#13187);
#10138=LINE('',#62722,#13188);
#10139=LINE('',#62725,#13189);
#10140=LINE('',#62732,#13190);
#10141=LINE('',#62733,#13191);
#10142=LINE('',#62735,#13192);
#10143=LINE('',#62736,#13193);
#10144=LINE('',#62739,#13194);
#10145=LINE('',#62760,#13195);
#10146=LINE('',#62761,#13196);
#10147=LINE('',#62769,#13197);
#10148=LINE('',#62785,#13198);
#10149=LINE('',#62786,#13199);
#10150=LINE('',#62788,#13200);
#10151=LINE('',#62790,#13201);
#10152=LINE('',#62791,#13202);
#10153=LINE('',#62794,#13203);
#10154=LINE('',#62795,#13204);
#10155=LINE('',#62798,#13205);
#10156=LINE('',#62799,#13206);
#10157=LINE('',#62802,#13207);
#10158=LINE('',#62803,#13208);
#10159=LINE('',#62813,#13209);
#10160=LINE('',#62815,#13210);
#10161=LINE('',#62817,#13211);
#10162=LINE('',#62822,#13212);
#10163=LINE('',#62867,#13213);
#10164=LINE('',#62871,#13214);
#10165=LINE('',#62875,#13215);
#10166=LINE('',#62879,#13216);
#10167=LINE('',#62883,#13217);
#10168=LINE('',#62891,#13218);
#10169=LINE('',#62893,#13219);
#10170=LINE('',#62894,#13220);
#10171=LINE('',#62913,#13221);
#10172=LINE('',#62914,#13222);
#10173=LINE('',#62915,#13223);
#10174=LINE('',#62918,#13224);
#10175=LINE('',#62919,#13225);
#10176=LINE('',#62923,#13226);
#10177=LINE('',#62925,#13227);
#10178=LINE('',#62926,#13228);
#10179=LINE('',#62932,#13229);
#10180=LINE('',#62934,#13230);
#10181=LINE('',#62935,#13231);
#10182=LINE('',#62943,#13232);
#10183=LINE('',#62949,#13233);
#10184=LINE('',#62954,#13234);
#10185=LINE('',#62956,#13235);
#10186=LINE('',#62997,#13236);
#10187=LINE('',#63003,#13237);
#10188=LINE('',#63010,#13238);
#10189=LINE('',#63013,#13239);
#10190=LINE('',#63019,#13240);
#10191=LINE('',#63025,#13241);
#10192=LINE('',#63031,#13242);
#10193=LINE('',#63037,#13243);
#10194=LINE('',#63043,#13244);
#10195=LINE('',#63053,#13245);
#10196=LINE('',#63057,#13246);
#10197=LINE('',#63064,#13247);
#10198=LINE('',#63066,#13248);
#10199=LINE('',#63073,#13249);
#10200=LINE('',#63077,#13250);
#10201=LINE('',#63081,#13251);
#10202=LINE('',#63085,#13252);
#10203=LINE('',#63089,#13253);
#10204=LINE('',#63092,#13254);
#10205=LINE('',#63097,#13255);
#10206=LINE('',#63130,#13256);
#10207=LINE('',#63214,#13257);
#10208=LINE('',#63304,#13258);
#10209=LINE('',#63394,#13259);
#10210=LINE('',#63478,#13260);
#10211=LINE('',#63568,#13261);
#10212=LINE('',#63652,#13262);
#10213=LINE('',#63739,#13263);
#10214=LINE('',#63829,#13264);
#10215=LINE('',#63913,#13265);
#10216=LINE('',#64003,#13266);
#10217=LINE('',#64093,#13267);
#10218=LINE('',#64177,#13268);
#10219=LINE('',#64267,#13269);
#10220=LINE('',#64354,#13270);
#10221=LINE('',#64441,#13271);
#10222=LINE('',#64531,#13272);
#10223=LINE('',#64615,#13273);
#10224=LINE('',#64705,#13274);
#10225=LINE('',#64795,#13275);
#10226=LINE('',#64879,#13276);
#10227=LINE('',#64969,#13277);
#10228=LINE('',#65056,#13278);
#10229=LINE('',#65143,#13279);
#10230=LINE('',#65233,#13280);
#10231=LINE('',#65317,#13281);
#10232=LINE('',#65407,#13282);
#10233=LINE('',#65497,#13283);
#10234=LINE('',#65581,#13284);
#10235=LINE('',#65591,#13285);
#10236=LINE('',#65627,#13286);
#10237=LINE('',#65664,#13287);
#10238=LINE('',#65702,#13288);
#10239=LINE('',#65739,#13289);
#10240=LINE('',#65776,#13290);
#10241=LINE('',#65814,#13291);
#10242=LINE('',#65850,#13292);
#10243=LINE('',#65888,#13293);
#10244=LINE('',#65925,#13294);
#10245=LINE('',#65962,#13295);
#10246=LINE('',#66000,#13296);
#10247=LINE('',#66037,#13297);
#10248=LINE('',#66074,#13298);
#10249=LINE('',#66112,#13299);
#10250=LINE('',#66148,#13300);
#10251=LINE('',#66186,#13301);
#10252=LINE('',#66223,#13302);
#10253=LINE('',#66260,#13303);
#10254=LINE('',#66298,#13304);
#10255=LINE('',#66335,#13305);
#10256=LINE('',#66372,#13306);
#10257=LINE('',#66410,#13307);
#10258=LINE('',#66447,#13308);
#10259=LINE('',#66484,#13309);
#10260=LINE('',#66521,#13310);
#10261=LINE('',#66558,#13311);
#10262=LINE('',#66596,#13312);
#10263=LINE('',#66634,#13313);
#10264=LINE('',#66640,#13314);
#10265=LINE('',#66654,#13315);
#10266=LINE('',#66660,#13316);
#10267=LINE('',#66662,#13317);
#10268=LINE('',#66663,#13318);
#10269=LINE('',#66670,#13319);
#10270=LINE('',#66672,#13320);
#10271=LINE('',#66678,#13321);
#10272=LINE('',#66686,#13322);
#10273=LINE('',#66704,#13323);
#10274=LINE('',#66705,#13324);
#10275=LINE('',#66706,#13325);
#10276=LINE('',#66708,#13326);
#10277=LINE('',#70186,#13327);
#10278=LINE('',#70188,#13328);
#10279=LINE('',#70190,#13329);
#10280=LINE('',#70191,#13330);
#10281=LINE('',#70195,#13331);
#10282=LINE('',#70198,#13332);
#10283=LINE('',#70199,#13333);
#10284=LINE('',#70205,#13334);
#10285=LINE('',#70207,#13335);
#10286=LINE('',#70209,#13336);
#10287=LINE('',#70210,#13337);
#10288=LINE('',#70214,#13338);
#10289=LINE('',#70217,#13339);
#10290=LINE('',#70218,#13340);
#10291=LINE('',#70224,#13341);
#10292=LINE('',#70226,#13342);
#10293=LINE('',#70228,#13343);
#10294=LINE('',#70229,#13344);
#10295=LINE('',#70233,#13345);
#10296=LINE('',#70236,#13346);
#10297=LINE('',#70237,#13347);
#10298=LINE('',#70243,#13348);
#10299=LINE('',#70245,#13349);
#10300=LINE('',#70247,#13350);
#10301=LINE('',#70248,#13351);
#10302=LINE('',#70252,#13352);
#10303=LINE('',#70255,#13353);
#10304=LINE('',#70256,#13354);
#10305=LINE('',#70262,#13355);
#10306=LINE('',#70264,#13356);
#10307=LINE('',#70266,#13357);
#10308=LINE('',#70267,#13358);
#10309=LINE('',#70271,#13359);
#10310=LINE('',#70274,#13360);
#10311=LINE('',#70275,#13361);
#10312=LINE('',#70281,#13362);
#10313=LINE('',#70283,#13363);
#10314=LINE('',#70285,#13364);
#10315=LINE('',#70286,#13365);
#10316=LINE('',#70290,#13366);
#10317=LINE('',#70293,#13367);
#10318=LINE('',#70294,#13368);
#10319=LINE('',#70300,#13369);
#10320=LINE('',#70302,#13370);
#10321=LINE('',#70304,#13371);
#10322=LINE('',#70305,#13372);
#10323=LINE('',#70309,#13373);
#10324=LINE('',#70312,#13374);
#10325=LINE('',#70313,#13375);
#10326=LINE('',#70319,#13376);
#10327=LINE('',#70321,#13377);
#10328=LINE('',#70323,#13378);
#10329=LINE('',#70324,#13379);
#10330=LINE('',#70328,#13380);
#10331=LINE('',#70331,#13381);
#10332=LINE('',#70332,#13382);
#10333=LINE('',#70338,#13383);
#10334=LINE('',#70340,#13384);
#10335=LINE('',#70342,#13385);
#10336=LINE('',#70343,#13386);
#10337=LINE('',#70347,#13387);
#10338=LINE('',#70350,#13388);
#10339=LINE('',#70351,#13389);
#10340=LINE('',#70357,#13390);
#10341=LINE('',#70359,#13391);
#10342=LINE('',#70361,#13392);
#10343=LINE('',#70362,#13393);
#10344=LINE('',#70366,#13394);
#10345=LINE('',#70369,#13395);
#10346=LINE('',#70370,#13396);
#10347=LINE('',#70376,#13397);
#10348=LINE('',#70378,#13398);
#10349=LINE('',#70380,#13399);
#10350=LINE('',#70381,#13400);
#10351=LINE('',#70385,#13401);
#10352=LINE('',#70388,#13402);
#10353=LINE('',#70389,#13403);
#10354=LINE('',#70395,#13404);
#10355=LINE('',#70397,#13405);
#10356=LINE('',#70399,#13406);
#10357=LINE('',#70400,#13407);
#10358=LINE('',#70404,#13408);
#10359=LINE('',#70407,#13409);
#10360=LINE('',#70408,#13410);
#10361=LINE('',#70414,#13411);
#10362=LINE('',#70416,#13412);
#10363=LINE('',#70418,#13413);
#10364=LINE('',#70419,#13414);
#10365=LINE('',#70423,#13415);
#10366=LINE('',#70426,#13416);
#10367=LINE('',#70427,#13417);
#10368=LINE('',#70433,#13418);
#10369=LINE('',#70435,#13419);
#10370=LINE('',#70437,#13420);
#10371=LINE('',#70438,#13421);
#10372=LINE('',#70442,#13422);
#10373=LINE('',#70445,#13423);
#10374=LINE('',#70446,#13424);
#10375=LINE('',#70452,#13425);
#10376=LINE('',#70454,#13426);
#10377=LINE('',#70456,#13427);
#10378=LINE('',#70457,#13428);
#10379=LINE('',#70461,#13429);
#10380=LINE('',#70464,#13430);
#10381=LINE('',#70465,#13431);
#10382=LINE('',#70471,#13432);
#10383=LINE('',#70473,#13433);
#10384=LINE('',#70475,#13434);
#10385=LINE('',#70476,#13435);
#10386=LINE('',#70480,#13436);
#10387=LINE('',#70483,#13437);
#10388=LINE('',#70484,#13438);
#10389=LINE('',#70490,#13439);
#10390=LINE('',#70492,#13440);
#10391=LINE('',#70494,#13441);
#10392=LINE('',#70495,#13442);
#10393=LINE('',#70499,#13443);
#10394=LINE('',#70502,#13444);
#10395=LINE('',#70503,#13445);
#10396=LINE('',#70509,#13446);
#10397=LINE('',#70511,#13447);
#10398=LINE('',#70513,#13448);
#10399=LINE('',#70514,#13449);
#10400=LINE('',#70519,#13450);
#10401=LINE('',#70523,#13451);
#10402=LINE('',#70524,#13452);
#10403=LINE('',#70532,#13453);
#10404=LINE('',#70534,#13454);
#10405=LINE('',#70536,#13455);
#10406=LINE('',#70537,#13456);
#10407=LINE('',#70541,#13457);
#10408=LINE('',#70544,#13458);
#10409=LINE('',#70545,#13459);
#10410=LINE('',#70551,#13460);
#10411=LINE('',#70553,#13461);
#10412=LINE('',#70555,#13462);
#10413=LINE('',#70556,#13463);
#10414=LINE('',#70560,#13464);
#10415=LINE('',#70563,#13465);
#10416=LINE('',#70564,#13466);
#10417=LINE('',#70570,#13467);
#10418=LINE('',#70572,#13468);
#10419=LINE('',#70574,#13469);
#10420=LINE('',#70575,#13470);
#10421=LINE('',#70579,#13471);
#10422=LINE('',#70582,#13472);
#10423=LINE('',#70583,#13473);
#10424=LINE('',#70589,#13474);
#10425=LINE('',#70591,#13475);
#10426=LINE('',#70593,#13476);
#10427=LINE('',#70594,#13477);
#10428=LINE('',#70598,#13478);
#10429=LINE('',#70601,#13479);
#10430=LINE('',#70602,#13480);
#10431=LINE('',#70608,#13481);
#10432=LINE('',#70610,#13482);
#10433=LINE('',#70612,#13483);
#10434=LINE('',#70613,#13484);
#10435=LINE('',#70617,#13485);
#10436=LINE('',#70620,#13486);
#10437=LINE('',#70621,#13487);
#10438=LINE('',#70627,#13488);
#10439=LINE('',#70629,#13489);
#10440=LINE('',#70631,#13490);
#10441=LINE('',#70632,#13491);
#10442=LINE('',#70636,#13492);
#10443=LINE('',#70639,#13493);
#10444=LINE('',#70640,#13494);
#10445=LINE('',#70646,#13495);
#10446=LINE('',#70648,#13496);
#10447=LINE('',#70650,#13497);
#10448=LINE('',#70651,#13498);
#10449=LINE('',#70655,#13499);
#10450=LINE('',#70658,#13500);
#10451=LINE('',#70659,#13501);
#10452=LINE('',#70665,#13502);
#10453=LINE('',#70667,#13503);
#10454=LINE('',#70669,#13504);
#10455=LINE('',#70670,#13505);
#10456=LINE('',#70674,#13506);
#10457=LINE('',#70677,#13507);
#10458=LINE('',#70678,#13508);
#10459=LINE('',#70684,#13509);
#10460=LINE('',#70686,#13510);
#10461=LINE('',#70688,#13511);
#10462=LINE('',#70689,#13512);
#10463=LINE('',#70693,#13513);
#10464=LINE('',#70696,#13514);
#10465=LINE('',#70697,#13515);
#10466=LINE('',#70703,#13516);
#10467=LINE('',#70705,#13517);
#10468=LINE('',#70707,#13518);
#10469=LINE('',#70708,#13519);
#10470=LINE('',#70712,#13520);
#10471=LINE('',#70715,#13521);
#10472=LINE('',#70716,#13522);
#10473=LINE('',#70722,#13523);
#10474=LINE('',#70724,#13524);
#10475=LINE('',#70726,#13525);
#10476=LINE('',#70727,#13526);
#10477=LINE('',#70731,#13527);
#10478=LINE('',#70734,#13528);
#10479=LINE('',#70735,#13529);
#10480=LINE('',#70741,#13530);
#10481=LINE('',#70743,#13531);
#10482=LINE('',#70745,#13532);
#10483=LINE('',#70746,#13533);
#10484=LINE('',#70750,#13534);
#10485=LINE('',#70753,#13535);
#10486=LINE('',#70754,#13536);
#10487=LINE('',#70760,#13537);
#10488=LINE('',#70762,#13538);
#10489=LINE('',#70764,#13539);
#10490=LINE('',#70765,#13540);
#10491=LINE('',#70769,#13541);
#10492=LINE('',#70772,#13542);
#10493=LINE('',#70773,#13543);
#10494=LINE('',#70779,#13544);
#10495=LINE('',#70781,#13545);
#10496=LINE('',#70783,#13546);
#10497=LINE('',#70784,#13547);
#10498=LINE('',#70788,#13548);
#10499=LINE('',#70791,#13549);
#10500=LINE('',#70792,#13550);
#10501=LINE('',#70798,#13551);
#10502=LINE('',#70800,#13552);
#10503=LINE('',#70802,#13553);
#10504=LINE('',#70803,#13554);
#10505=LINE('',#70807,#13555);
#10506=LINE('',#70810,#13556);
#10507=LINE('',#70811,#13557);
#10508=LINE('',#70817,#13558);
#10509=LINE('',#70819,#13559);
#10510=LINE('',#70821,#13560);
#10511=LINE('',#70822,#13561);
#10512=LINE('',#70826,#13562);
#10513=LINE('',#70829,#13563);
#10514=LINE('',#70830,#13564);
#10515=LINE('',#70836,#13565);
#10516=LINE('',#70838,#13566);
#10517=LINE('',#70840,#13567);
#10518=LINE('',#70841,#13568);
#10519=LINE('',#70845,#13569);
#10520=LINE('',#70848,#13570);
#10521=LINE('',#70849,#13571);
#10522=LINE('',#70855,#13572);
#10523=LINE('',#70857,#13573);
#10524=LINE('',#70859,#13574);
#10525=LINE('',#70860,#13575);
#10526=LINE('',#70864,#13576);
#10527=LINE('',#70867,#13577);
#10528=LINE('',#70868,#13578);
#10529=LINE('',#70874,#13579);
#10530=LINE('',#70875,#13580);
#10531=LINE('',#70877,#13581);
#10532=LINE('',#70883,#13582);
#10533=LINE('',#71335,#13583);
#10534=LINE('',#71337,#13584);
#10535=LINE('',#71338,#13585);
#10536=LINE('',#71342,#13586);
#10537=LINE('',#71344,#13587);
#10538=LINE('',#71345,#13588);
#10539=LINE('',#71349,#13589);
#10540=LINE('',#71351,#13590);
#10541=LINE('',#71352,#13591);
#10542=LINE('',#71354,#13592);
#10543=LINE('',#71355,#13593);
#10544=LINE('',#71357,#13594);
#10545=LINE('',#71361,#13595);
#10546=LINE('',#71363,#13596);
#10547=LINE('',#71364,#13597);
#10548=LINE('',#71373,#13598);
#10549=LINE('',#71377,#13599);
#10550=LINE('',#71379,#13600);
#10551=LINE('',#71380,#13601);
#10552=LINE('',#71382,#13602);
#10553=LINE('',#71383,#13603);
#10554=LINE('',#71385,#13604);
#10555=LINE('',#71389,#13605);
#10556=LINE('',#71391,#13606);
#10557=LINE('',#71392,#13607);
#10558=LINE('',#71394,#13608);
#10559=LINE('',#71395,#13609);
#10560=LINE('',#71411,#13610);
#10561=LINE('',#71414,#13611);
#10562=LINE('',#71436,#13612);
#10563=LINE('',#71468,#13613);
#10564=LINE('',#71469,#13614);
#10565=LINE('',#71501,#13615);
#10566=LINE('',#71502,#13616);
#10567=LINE('',#71504,#13617);
#10568=LINE('',#71505,#13618);
#10569=LINE('',#71537,#13619);
#10570=LINE('',#71538,#13620);
#10571=LINE('',#71540,#13621);
#10572=LINE('',#71541,#13622);
#10573=LINE('',#71543,#13623);
#10574=LINE('',#71544,#13624);
#10575=LINE('',#71546,#13625);
#10576=LINE('',#71547,#13626);
#10577=LINE('',#71549,#13627);
#10578=LINE('',#71550,#13628);
#10579=LINE('',#71552,#13629);
#10580=LINE('',#71553,#13630);
#10581=LINE('',#71567,#13631);
#10582=LINE('',#71571,#13632);
#10583=LINE('',#71577,#13633);
#10584=VECTOR('',#37671,39.77639320225);
#10585=VECTOR('',#37678,38.5);
#10586=VECTOR('',#37687,40.);
#10587=VECTOR('',#37690,36.97360679775);
#10588=VECTOR('',#37701,26.25);
#10589=VECTOR('',#37710,26.);
#10590=VECTOR('',#37719,31.9267766952966);
#10591=VECTOR('',#37726,33.);
#10592=VECTOR('',#37737,33.8502380998955);
#10593=VECTOR('',#37744,35.25);
#10594=VECTOR('',#37753,126.961414092626);
#10595=VECTOR('',#37760,129.25);
#10596=VECTOR('',#37769,124.);
#10597=VECTOR('',#37772,131.441987426416);
#10598=VECTOR('',#37779,133.);
#10599=VECTOR('',#37786,134.437780860397);
#10600=VECTOR('',#37793,135.25);
#10601=VECTOR('',#37800,135.912219139603);
#10602=VECTOR('',#37807,136.);
#10603=VECTOR('',#37812,10.);
#10604=VECTOR('',#37817,136.);
#10605=VECTOR('',#37824,10.);
#10606=VECTOR('',#37829,10.);
#10607=VECTOR('',#37836,10.);
#10608=VECTOR('',#37843,10.);
#10609=VECTOR('',#37850,10.);
#10610=VECTOR('',#37857,10.);
#10611=VECTOR('',#37864,10.);
#10612=VECTOR('',#37871,10.);
#10613=VECTOR('',#37878,10.);
#10614=VECTOR('',#37885,10.);
#10615=VECTOR('',#37892,10.);
#10616=VECTOR('',#37899,10.);
#10617=VECTOR('',#37906,10.);
#10618=VECTOR('',#37913,10.);
#10619=VECTOR('',#37920,10.);
#10620=VECTOR('',#37927,10.);
#10621=VECTOR('',#37934,10.);
#10622=VECTOR('',#37941,10.);
#10623=VECTOR('',#37948,10.);
#10624=VECTOR('',#37955,10.);
#10625=VECTOR('',#37962,10.);
#10626=VECTOR('',#37969,10.);
#10627=VECTOR('',#37976,10.);
#10628=VECTOR('',#37983,10.);
#10629=VECTOR('',#37990,10.);
#10630=VECTOR('',#37997,10.);
#10631=VECTOR('',#38004,10.);
#10632=VECTOR('',#38011,10.);
#10633=VECTOR('',#38018,10.);
#10634=VECTOR('',#38025,10.);
#10635=VECTOR('',#38032,10.);
#10636=VECTOR('',#38039,10.);
#10637=VECTOR('',#38046,10.);
#10638=VECTOR('',#38053,10.);
#10639=VECTOR('',#38060,10.);
#10640=VECTOR('',#38067,10.);
#10641=VECTOR('',#38074,10.);
#10642=VECTOR('',#38081,10.);
#10643=VECTOR('',#38088,10.);
#10644=VECTOR('',#38095,10.);
#10645=VECTOR('',#38102,10.);
#10646=VECTOR('',#38109,10.);
#10647=VECTOR('',#38116,10.);
#10648=VECTOR('',#38123,10.);
#10649=VECTOR('',#38130,10.);
#10650=VECTOR('',#38137,10.);
#10651=VECTOR('',#38144,10.);
#10652=VECTOR('',#38151,10.);
#10653=VECTOR('',#38158,10.);
#10654=VECTOR('',#38165,10.);
#10655=VECTOR('',#38172,10.);
#10656=VECTOR('',#38179,10.);
#10657=VECTOR('',#38186,10.);
#10658=VECTOR('',#38193,10.);
#10659=VECTOR('',#38200,10.);
#10660=VECTOR('',#38207,10.);
#10661=VECTOR('',#38214,10.);
#10662=VECTOR('',#38221,10.);
#10663=VECTOR('',#38228,10.);
#10664=VECTOR('',#38235,10.);
#10665=VECTOR('',#38242,10.);
#10666=VECTOR('',#38249,10.);
#10667=VECTOR('',#38256,10.);
#10668=VECTOR('',#38263,10.);
#10669=VECTOR('',#38270,10.);
#10670=VECTOR('',#38277,10.);
#10671=VECTOR('',#38284,10.);
#10672=VECTOR('',#38291,10.);
#10673=VECTOR('',#38298,10.);
#10674=VECTOR('',#38305,10.);
#10675=VECTOR('',#38312,10.);
#10676=VECTOR('',#38319,10.);
#10677=VECTOR('',#38326,10.);
#10678=VECTOR('',#38333,10.);
#10679=VECTOR('',#38340,10.);
#10680=VECTOR('',#38347,10.);
#10681=VECTOR('',#38354,10.);
#10682=VECTOR('',#38361,10.);
#10683=VECTOR('',#38368,10.);
#10684=VECTOR('',#38375,10.);
#10685=VECTOR('',#38382,10.);
#10686=VECTOR('',#38389,10.);
#10687=VECTOR('',#38396,10.);
#10688=VECTOR('',#38403,10.);
#10689=VECTOR('',#38410,10.);
#10690=VECTOR('',#38417,10.);
#10691=VECTOR('',#38424,10.);
#10692=VECTOR('',#38431,10.);
#10693=VECTOR('',#38438,10.);
#10694=VECTOR('',#38445,10.);
#10695=VECTOR('',#38452,10.);
#10696=VECTOR('',#38459,10.);
#10697=VECTOR('',#38466,10.);
#10698=VECTOR('',#38473,10.);
#10699=VECTOR('',#38480,10.);
#10700=VECTOR('',#38487,10.);
#10701=VECTOR('',#38494,10.);
#10702=VECTOR('',#38501,10.);
#10703=VECTOR('',#38508,10.);
#10704=VECTOR('',#38515,10.);
#10705=VECTOR('',#38522,10.);
#10706=VECTOR('',#38529,10.);
#10707=VECTOR('',#38536,10.);
#10708=VECTOR('',#38543,10.);
#10709=VECTOR('',#38550,10.);
#10710=VECTOR('',#38557,10.);
#10711=VECTOR('',#38564,10.);
#10712=VECTOR('',#38571,10.);
#10713=VECTOR('',#38578,10.);
#10714=VECTOR('',#38585,10.);
#10715=VECTOR('',#38592,10.);
#10716=VECTOR('',#38599,10.);
#10717=VECTOR('',#38606,10.);
#10718=VECTOR('',#38613,10.);
#10719=VECTOR('',#38620,10.);
#10720=VECTOR('',#38627,10.);
#10721=VECTOR('',#38634,10.);
#10722=VECTOR('',#38641,10.);
#10723=VECTOR('',#38648,10.);
#10724=VECTOR('',#38655,10.);
#10725=VECTOR('',#38662,10.);
#10726=VECTOR('',#38669,10.);
#10727=VECTOR('',#38676,10.);
#10728=VECTOR('',#38683,10.);
#10729=VECTOR('',#38690,10.);
#10730=VECTOR('',#38697,10.);
#10731=VECTOR('',#38704,10.);
#10732=VECTOR('',#38711,10.);
#10733=VECTOR('',#38718,10.);
#10734=VECTOR('',#38725,10.);
#10735=VECTOR('',#38732,10.);
#10736=VECTOR('',#38739,10.);
#10737=VECTOR('',#38746,10.);
#10738=VECTOR('',#38753,10.);
#10739=VECTOR('',#38760,10.);
#10740=VECTOR('',#38767,10.);
#10741=VECTOR('',#38774,10.);
#10742=VECTOR('',#38781,10.);
#10743=VECTOR('',#38788,10.);
#10744=VECTOR('',#38795,10.);
#10745=VECTOR('',#38802,10.);
#10746=VECTOR('',#38809,10.);
#10747=VECTOR('',#38816,10.);
#10748=VECTOR('',#38885,10.);
#10749=VECTOR('',#38888,10.);
#10750=VECTOR('',#38891,10.);
#10751=VECTOR('',#38896,10.);
#10752=VECTOR('',#38901,10.);
#10753=VECTOR('',#38906,10.);
#10754=VECTOR('',#38911,10.);
#10755=VECTOR('',#38928,10.);
#10756=VECTOR('',#38929,10.);
#10757=VECTOR('',#38930,10.);
#10758=VECTOR('',#38931,10.);
#10759=VECTOR('',#38934,10.);
#10760=VECTOR('',#38935,10.);
#10761=VECTOR('',#38938,10.);
#10762=VECTOR('',#38939,10.);
#10763=VECTOR('',#38940,10.);
#10764=VECTOR('',#38943,10.);
#10765=VECTOR('',#38944,10.);
#10766=VECTOR('',#38945,10.);
#10767=VECTOR('',#38948,10.);
#10768=VECTOR('',#38949,10.);
#10769=VECTOR('',#38952,10.);
#10770=VECTOR('',#38953,10.);
#10771=VECTOR('',#38956,10.);
#10772=VECTOR('',#38957,10.);
#10773=VECTOR('',#38960,10.);
#10774=VECTOR('',#38961,10.);
#10775=VECTOR('',#38962,10.);
#10776=VECTOR('',#38965,10.);
#10777=VECTOR('',#38966,10.);
#10778=VECTOR('',#38969,10.);
#10779=VECTOR('',#38970,10.);
#10780=VECTOR('',#38973,10.);
#10781=VECTOR('',#38974,10.);
#10782=VECTOR('',#38977,10.);
#10783=VECTOR('',#38984,10.);
#10784=VECTOR('',#38985,10.);
#10785=VECTOR('',#38986,10.);
#10786=VECTOR('',#38989,10.);
#10787=VECTOR('',#38990,10.);
#10788=VECTOR('',#38991,10.);
#10789=VECTOR('',#38994,10.);
#10790=VECTOR('',#38995,10.);
#10791=VECTOR('',#38996,10.);
#10792=VECTOR('',#38999,10.);
#10793=VECTOR('',#39000,10.);
#10794=VECTOR('',#39003,10.);
#10795=VECTOR('',#39004,10.);
#10796=VECTOR('',#39005,10.);
#10797=VECTOR('',#39008,10.);
#10798=VECTOR('',#39009,10.);
#10799=VECTOR('',#39012,10.);
#10800=VECTOR('',#39013,10.);
#10801=VECTOR('',#39016,10.);
#10802=VECTOR('',#39017,10.);
#10803=VECTOR('',#39020,10.);
#10804=VECTOR('',#39021,10.);
#10805=VECTOR('',#39024,10.);
#10806=VECTOR('',#39025,10.);
#10807=VECTOR('',#39028,10.);
#10808=VECTOR('',#39029,10.);
#10809=VECTOR('',#39032,10.);
#10810=VECTOR('',#39033,10.);
#10811=VECTOR('',#39042,10.);
#10812=VECTOR('',#39043,10.);
#10813=VECTOR('',#39044,10.);
#10814=VECTOR('',#39047,10.);
#10815=VECTOR('',#39048,10.);
#10816=VECTOR('',#39049,10.);
#10817=VECTOR('',#39050,10.);
#10818=VECTOR('',#39053,10.);
#10819=VECTOR('',#39054,10.);
#10820=VECTOR('',#39057,10.);
#10821=VECTOR('',#39058,10.);
#10822=VECTOR('',#39059,10.);
#10823=VECTOR('',#39062,10.);
#10824=VECTOR('',#39063,10.);
#10825=VECTOR('',#39064,10.);
#10826=VECTOR('',#39065,10.);
#10827=VECTOR('',#39068,10.);
#10828=VECTOR('',#39069,10.);
#10829=VECTOR('',#39072,10.);
#10830=VECTOR('',#39073,10.);
#10831=VECTOR('',#39076,10.);
#10832=VECTOR('',#39077,10.);
#10833=VECTOR('',#39078,10.);
#10834=VECTOR('',#39081,10.);
#10835=VECTOR('',#39084,10.);
#10836=VECTOR('',#39085,10.);
#10837=VECTOR('',#39088,10.);
#10838=VECTOR('',#39089,10.);
#10839=VECTOR('',#39096,10.);
#10840=VECTOR('',#39097,10.);
#10841=VECTOR('',#39098,10.);
#10842=VECTOR('',#39101,10.);
#10843=VECTOR('',#39102,10.);
#10844=VECTOR('',#39103,10.);
#10845=VECTOR('',#39106,10.);
#10846=VECTOR('',#39107,10.);
#10847=VECTOR('',#39108,10.);
#10848=VECTOR('',#39111,10.);
#10849=VECTOR('',#39112,10.);
#10850=VECTOR('',#39115,10.);
#10851=VECTOR('',#39116,10.);
#10852=VECTOR('',#39117,10.);
#10853=VECTOR('',#39120,10.);
#10854=VECTOR('',#39121,10.);
#10855=VECTOR('',#39124,10.);
#10856=VECTOR('',#39125,10.);
#10857=VECTOR('',#39128,10.);
#10858=VECTOR('',#39129,10.);
#10859=VECTOR('',#39132,10.);
#10860=VECTOR('',#39133,10.);
#10861=VECTOR('',#39136,10.);
#10862=VECTOR('',#39137,10.);
#10863=VECTOR('',#39140,10.);
#10864=VECTOR('',#39141,10.);
#10865=VECTOR('',#39144,10.);
#10866=VECTOR('',#39145,10.);
#10867=VECTOR('',#39154,10.);
#10868=VECTOR('',#39155,10.);
#10869=VECTOR('',#39156,10.);
#10870=VECTOR('',#39159,10.);
#10871=VECTOR('',#39160,10.);
#10872=VECTOR('',#39161,10.);
#10873=VECTOR('',#39164,10.);
#10874=VECTOR('',#39165,10.);
#10875=VECTOR('',#39166,10.);
#10876=VECTOR('',#39169,10.);
#10877=VECTOR('',#39170,10.);
#10878=VECTOR('',#39173,10.);
#10879=VECTOR('',#39174,10.);
#10880=VECTOR('',#39175,10.);
#10881=VECTOR('',#39178,10.);
#10882=VECTOR('',#39179,10.);
#10883=VECTOR('',#39182,10.);
#10884=VECTOR('',#39183,10.);
#10885=VECTOR('',#39186,10.);
#10886=VECTOR('',#39187,10.);
#10887=VECTOR('',#39190,10.);
#10888=VECTOR('',#39191,10.);
#10889=VECTOR('',#39194,10.);
#10890=VECTOR('',#39195,10.);
#10891=VECTOR('',#39198,10.);
#10892=VECTOR('',#39199,10.);
#10893=VECTOR('',#39202,10.);
#10894=VECTOR('',#39203,10.);
#10895=VECTOR('',#39212,10.);
#10896=VECTOR('',#39213,10.);
#10897=VECTOR('',#39214,10.);
#10898=VECTOR('',#39215,10.);
#10899=VECTOR('',#39218,10.);
#10900=VECTOR('',#39219,10.);
#10901=VECTOR('',#39222,10.);
#10902=VECTOR('',#39223,10.);
#10903=VECTOR('',#39224,10.);
#10904=VECTOR('',#39227,10.);
#10905=VECTOR('',#39228,10.);
#10906=VECTOR('',#39229,10.);
#10907=VECTOR('',#39232,10.);
#10908=VECTOR('',#39233,10.);
#10909=VECTOR('',#39236,10.);
#10910=VECTOR('',#39237,10.);
#10911=VECTOR('',#39240,10.);
#10912=VECTOR('',#39241,10.);
#10913=VECTOR('',#39244,10.);
#10914=VECTOR('',#39245,10.);
#10915=VECTOR('',#39246,10.);
#10916=VECTOR('',#39249,10.);
#10917=VECTOR('',#39250,10.);
#10918=VECTOR('',#39253,10.);
#10919=VECTOR('',#39254,10.);
#10920=VECTOR('',#39257,10.);
#10921=VECTOR('',#39258,10.);
#10922=VECTOR('',#39261,10.);
#10923=VECTOR('',#39268,10.);
#10924=VECTOR('',#39269,10.);
#10925=VECTOR('',#39270,10.);
#10926=VECTOR('',#39273,10.);
#10927=VECTOR('',#39274,10.);
#10928=VECTOR('',#39275,10.);
#10929=VECTOR('',#39278,10.);
#10930=VECTOR('',#39279,10.);
#10931=VECTOR('',#39280,10.);
#10932=VECTOR('',#39283,10.);
#10933=VECTOR('',#39284,10.);
#10934=VECTOR('',#39287,10.);
#10935=VECTOR('',#39288,10.);
#10936=VECTOR('',#39289,10.);
#10937=VECTOR('',#39292,10.);
#10938=VECTOR('',#39293,10.);
#10939=VECTOR('',#39296,10.);
#10940=VECTOR('',#39297,10.);
#10941=VECTOR('',#39300,10.);
#10942=VECTOR('',#39301,10.);
#10943=VECTOR('',#39304,10.);
#10944=VECTOR('',#39305,10.);
#10945=VECTOR('',#39308,10.);
#10946=VECTOR('',#39309,10.);
#10947=VECTOR('',#39312,10.);
#10948=VECTOR('',#39313,10.);
#10949=VECTOR('',#39316,10.);
#10950=VECTOR('',#39317,10.);
#10951=VECTOR('',#39326,10.);
#10952=VECTOR('',#39327,10.);
#10953=VECTOR('',#39328,10.);
#10954=VECTOR('',#39331,10.);
#10955=VECTOR('',#39332,10.);
#10956=VECTOR('',#39333,10.);
#10957=VECTOR('',#39334,10.);
#10958=VECTOR('',#39337,10.);
#10959=VECTOR('',#39338,10.);
#10960=VECTOR('',#39341,10.);
#10961=VECTOR('',#39342,10.);
#10962=VECTOR('',#39343,10.);
#10963=VECTOR('',#39346,10.);
#10964=VECTOR('',#39347,10.);
#10965=VECTOR('',#39348,10.);
#10966=VECTOR('',#39349,10.);
#10967=VECTOR('',#39352,10.);
#10968=VECTOR('',#39353,10.);
#10969=VECTOR('',#39356,10.);
#10970=VECTOR('',#39357,10.);
#10971=VECTOR('',#39360,10.);
#10972=VECTOR('',#39361,10.);
#10973=VECTOR('',#39362,10.);
#10974=VECTOR('',#39365,10.);
#10975=VECTOR('',#39368,10.);
#10976=VECTOR('',#39369,10.);
#10977=VECTOR('',#39372,10.);
#10978=VECTOR('',#39373,10.);
#10979=VECTOR('',#39380,10.);
#10980=VECTOR('',#39381,10.);
#10981=VECTOR('',#39382,10.);
#10982=VECTOR('',#39385,10.);
#10983=VECTOR('',#39386,10.);
#10984=VECTOR('',#39387,10.);
#10985=VECTOR('',#39390,10.);
#10986=VECTOR('',#39391,10.);
#10987=VECTOR('',#39392,10.);
#10988=VECTOR('',#39395,10.);
#10989=VECTOR('',#39396,10.);
#10990=VECTOR('',#39399,10.);
#10991=VECTOR('',#39400,10.);
#10992=VECTOR('',#39401,10.);
#10993=VECTOR('',#39404,10.);
#10994=VECTOR('',#39405,10.);
#10995=VECTOR('',#39408,10.);
#10996=VECTOR('',#39409,10.);
#10997=VECTOR('',#39412,10.);
#10998=VECTOR('',#39413,10.);
#10999=VECTOR('',#39416,10.);
#11000=VECTOR('',#39417,10.);
#11001=VECTOR('',#39420,10.);
#11002=VECTOR('',#39421,10.);
#11003=VECTOR('',#39424,10.);
#11004=VECTOR('',#39425,10.);
#11005=VECTOR('',#39428,10.);
#11006=VECTOR('',#39429,10.);
#11007=VECTOR('',#39438,10.);
#11008=VECTOR('',#39439,10.);
#11009=VECTOR('',#39440,10.);
#11010=VECTOR('',#39443,10.);
#11011=VECTOR('',#39444,10.);
#11012=VECTOR('',#39445,10.);
#11013=VECTOR('',#39448,10.);
#11014=VECTOR('',#39449,10.);
#11015=VECTOR('',#39450,10.);
#11016=VECTOR('',#39453,10.);
#11017=VECTOR('',#39454,10.);
#11018=VECTOR('',#39457,10.);
#11019=VECTOR('',#39458,10.);
#11020=VECTOR('',#39459,10.);
#11021=VECTOR('',#39462,10.);
#11022=VECTOR('',#39463,10.);
#11023=VECTOR('',#39466,10.);
#11024=VECTOR('',#39467,10.);
#11025=VECTOR('',#39470,10.);
#11026=VECTOR('',#39471,10.);
#11027=VECTOR('',#39474,10.);
#11028=VECTOR('',#39475,10.);
#11029=VECTOR('',#39478,10.);
#11030=VECTOR('',#39479,10.);
#11031=VECTOR('',#39482,10.);
#11032=VECTOR('',#39483,10.);
#11033=VECTOR('',#39486,10.);
#11034=VECTOR('',#39487,10.);
#11035=VECTOR('',#39496,10.);
#11036=VECTOR('',#39497,10.);
#11037=VECTOR('',#39498,10.);
#11038=VECTOR('',#39499,10.);
#11039=VECTOR('',#39502,10.);
#11040=VECTOR('',#39503,10.);
#11041=VECTOR('',#39506,10.);
#11042=VECTOR('',#39507,10.);
#11043=VECTOR('',#39508,10.);
#11044=VECTOR('',#39511,10.);
#11045=VECTOR('',#39512,10.);
#11046=VECTOR('',#39513,10.);
#11047=VECTOR('',#39516,10.);
#11048=VECTOR('',#39517,10.);
#11049=VECTOR('',#39520,10.);
#11050=VECTOR('',#39521,10.);
#11051=VECTOR('',#39524,10.);
#11052=VECTOR('',#39525,10.);
#11053=VECTOR('',#39528,10.);
#11054=VECTOR('',#39529,10.);
#11055=VECTOR('',#39530,10.);
#11056=VECTOR('',#39533,10.);
#11057=VECTOR('',#39534,10.);
#11058=VECTOR('',#39537,10.);
#11059=VECTOR('',#39538,10.);
#11060=VECTOR('',#39541,10.);
#11061=VECTOR('',#39542,10.);
#11062=VECTOR('',#39545,10.);
#11063=VECTOR('',#39552,10.);
#11064=VECTOR('',#39553,10.);
#11065=VECTOR('',#39554,10.);
#11066=VECTOR('',#39557,10.);
#11067=VECTOR('',#39558,10.);
#11068=VECTOR('',#39559,10.);
#11069=VECTOR('',#39562,10.);
#11070=VECTOR('',#39563,10.);
#11071=VECTOR('',#39564,10.);
#11072=VECTOR('',#39567,10.);
#11073=VECTOR('',#39568,10.);
#11074=VECTOR('',#39571,10.);
#11075=VECTOR('',#39572,10.);
#11076=VECTOR('',#39573,10.);
#11077=VECTOR('',#39576,10.);
#11078=VECTOR('',#39577,10.);
#11079=VECTOR('',#39580,10.);
#11080=VECTOR('',#39581,10.);
#11081=VECTOR('',#39584,10.);
#11082=VECTOR('',#39585,10.);
#11083=VECTOR('',#39588,10.);
#11084=VECTOR('',#39589,10.);
#11085=VECTOR('',#39592,10.);
#11086=VECTOR('',#39593,10.);
#11087=VECTOR('',#39596,10.);
#11088=VECTOR('',#39597,10.);
#11089=VECTOR('',#39600,10.);
#11090=VECTOR('',#39601,10.);
#11091=VECTOR('',#39610,10.);
#11092=VECTOR('',#39611,10.);
#11093=VECTOR('',#39612,10.);
#11094=VECTOR('',#39615,10.);
#11095=VECTOR('',#39616,10.);
#11096=VECTOR('',#39617,10.);
#11097=VECTOR('',#39618,10.);
#11098=VECTOR('',#39621,10.);
#11099=VECTOR('',#39622,10.);
#11100=VECTOR('',#39625,10.);
#11101=VECTOR('',#39626,10.);
#11102=VECTOR('',#39627,10.);
#11103=VECTOR('',#39630,10.);
#11104=VECTOR('',#39631,10.);
#11105=VECTOR('',#39632,10.);
#11106=VECTOR('',#39633,10.);
#11107=VECTOR('',#39636,10.);
#11108=VECTOR('',#39637,10.);
#11109=VECTOR('',#39640,10.);
#11110=VECTOR('',#39641,10.);
#11111=VECTOR('',#39644,10.);
#11112=VECTOR('',#39645,10.);
#11113=VECTOR('',#39646,10.);
#11114=VECTOR('',#39649,10.);
#11115=VECTOR('',#39652,10.);
#11116=VECTOR('',#39653,10.);
#11117=VECTOR('',#39656,10.);
#11118=VECTOR('',#39657,10.);
#11119=VECTOR('',#39664,10.);
#11120=VECTOR('',#39665,10.);
#11121=VECTOR('',#39666,10.);
#11122=VECTOR('',#39669,10.);
#11123=VECTOR('',#39670,10.);
#11124=VECTOR('',#39671,10.);
#11125=VECTOR('',#39674,10.);
#11126=VECTOR('',#39675,10.);
#11127=VECTOR('',#39676,10.);
#11128=VECTOR('',#39679,10.);
#11129=VECTOR('',#39680,10.);
#11130=VECTOR('',#39683,10.);
#11131=VECTOR('',#39684,10.);
#11132=VECTOR('',#39685,10.);
#11133=VECTOR('',#39688,10.);
#11134=VECTOR('',#39689,10.);
#11135=VECTOR('',#39692,10.);
#11136=VECTOR('',#39693,10.);
#11137=VECTOR('',#39696,10.);
#11138=VECTOR('',#39697,10.);
#11139=VECTOR('',#39700,10.);
#11140=VECTOR('',#39701,10.);
#11141=VECTOR('',#39704,10.);
#11142=VECTOR('',#39705,10.);
#11143=VECTOR('',#39708,10.);
#11144=VECTOR('',#39709,10.);
#11145=VECTOR('',#39712,10.);
#11146=VECTOR('',#39713,10.);
#11147=VECTOR('',#39722,10.);
#11148=VECTOR('',#39723,10.);
#11149=VECTOR('',#39724,10.);
#11150=VECTOR('',#39727,10.);
#11151=VECTOR('',#39728,10.);
#11152=VECTOR('',#39729,10.);
#11153=VECTOR('',#39732,10.);
#11154=VECTOR('',#39733,10.);
#11155=VECTOR('',#39734,10.);
#11156=VECTOR('',#39737,10.);
#11157=VECTOR('',#39738,10.);
#11158=VECTOR('',#39741,10.);
#11159=VECTOR('',#39742,10.);
#11160=VECTOR('',#39743,10.);
#11161=VECTOR('',#39746,10.);
#11162=VECTOR('',#39747,10.);
#11163=VECTOR('',#39750,10.);
#11164=VECTOR('',#39751,10.);
#11165=VECTOR('',#39754,10.);
#11166=VECTOR('',#39755,10.);
#11167=VECTOR('',#39758,10.);
#11168=VECTOR('',#39759,10.);
#11169=VECTOR('',#39762,10.);
#11170=VECTOR('',#39763,10.);
#11171=VECTOR('',#39766,10.);
#11172=VECTOR('',#39767,10.);
#11173=VECTOR('',#39770,10.);
#11174=VECTOR('',#39771,10.);
#11175=VECTOR('',#39780,10.);
#11176=VECTOR('',#39781,10.);
#11177=VECTOR('',#39782,10.);
#11178=VECTOR('',#39783,10.);
#11179=VECTOR('',#39786,10.);
#11180=VECTOR('',#39787,10.);
#11181=VECTOR('',#39790,10.);
#11182=VECTOR('',#39791,10.);
#11183=VECTOR('',#39792,10.);
#11184=VECTOR('',#39795,10.);
#11185=VECTOR('',#39796,10.);
#11186=VECTOR('',#39797,10.);
#11187=VECTOR('',#39800,10.);
#11188=VECTOR('',#39801,10.);
#11189=VECTOR('',#39804,10.);
#11190=VECTOR('',#39805,10.);
#11191=VECTOR('',#39808,10.);
#11192=VECTOR('',#39809,10.);
#11193=VECTOR('',#39812,10.);
#11194=VECTOR('',#39813,10.);
#11195=VECTOR('',#39814,10.);
#11196=VECTOR('',#39817,10.);
#11197=VECTOR('',#39818,10.);
#11198=VECTOR('',#39821,10.);
#11199=VECTOR('',#39822,10.);
#11200=VECTOR('',#39825,10.);
#11201=VECTOR('',#39826,10.);
#11202=VECTOR('',#39829,10.);
#11203=VECTOR('',#39836,10.);
#11204=VECTOR('',#39837,10.);
#11205=VECTOR('',#39838,10.);
#11206=VECTOR('',#39841,10.);
#11207=VECTOR('',#39842,10.);
#11208=VECTOR('',#39843,10.);
#11209=VECTOR('',#39846,10.);
#11210=VECTOR('',#39847,10.);
#11211=VECTOR('',#39848,10.);
#11212=VECTOR('',#39851,10.);
#11213=VECTOR('',#39852,10.);
#11214=VECTOR('',#39855,10.);
#11215=VECTOR('',#39856,10.);
#11216=VECTOR('',#39857,10.);
#11217=VECTOR('',#39860,10.);
#11218=VECTOR('',#39861,10.);
#11219=VECTOR('',#39864,10.);
#11220=VECTOR('',#39865,10.);
#11221=VECTOR('',#39868,10.);
#11222=VECTOR('',#39869,10.);
#11223=VECTOR('',#39872,10.);
#11224=VECTOR('',#39873,10.);
#11225=VECTOR('',#39876,10.);
#11226=VECTOR('',#39877,10.);
#11227=VECTOR('',#39880,10.);
#11228=VECTOR('',#39881,10.);
#11229=VECTOR('',#39884,10.);
#11230=VECTOR('',#39885,10.);
#11231=VECTOR('',#39894,10.);
#11232=VECTOR('',#39895,10.);
#11233=VECTOR('',#39896,10.);
#11234=VECTOR('',#39899,10.);
#11235=VECTOR('',#39900,10.);
#11236=VECTOR('',#39901,10.);
#11237=VECTOR('',#39902,10.);
#11238=VECTOR('',#39905,10.);
#11239=VECTOR('',#39906,10.);
#11240=VECTOR('',#39909,10.);
#11241=VECTOR('',#39910,10.);
#11242=VECTOR('',#39911,10.);
#11243=VECTOR('',#39914,10.);
#11244=VECTOR('',#39915,10.);
#11245=VECTOR('',#39916,10.);
#11246=VECTOR('',#39917,10.);
#11247=VECTOR('',#39920,10.);
#11248=VECTOR('',#39921,10.);
#11249=VECTOR('',#39924,10.);
#11250=VECTOR('',#39925,10.);
#11251=VECTOR('',#39928,10.);
#11252=VECTOR('',#39929,10.);
#11253=VECTOR('',#39930,10.);
#11254=VECTOR('',#39933,10.);
#11255=VECTOR('',#39936,10.);
#11256=VECTOR('',#39937,10.);
#11257=VECTOR('',#39940,10.);
#11258=VECTOR('',#39941,10.);
#11259=VECTOR('',#39948,10.);
#11260=VECTOR('',#39949,10.);
#11261=VECTOR('',#39950,10.);
#11262=VECTOR('',#39953,10.);
#11263=VECTOR('',#39954,10.);
#11264=VECTOR('',#39955,10.);
#11265=VECTOR('',#39958,10.);
#11266=VECTOR('',#39959,10.);
#11267=VECTOR('',#39960,10.);
#11268=VECTOR('',#39963,10.);
#11269=VECTOR('',#39964,10.);
#11270=VECTOR('',#39967,10.);
#11271=VECTOR('',#39968,10.);
#11272=VECTOR('',#39969,10.);
#11273=VECTOR('',#39972,10.);
#11274=VECTOR('',#39973,10.);
#11275=VECTOR('',#39976,10.);
#11276=VECTOR('',#39977,10.);
#11277=VECTOR('',#39980,10.);
#11278=VECTOR('',#39981,10.);
#11279=VECTOR('',#39984,10.);
#11280=VECTOR('',#39985,10.);
#11281=VECTOR('',#39988,10.);
#11282=VECTOR('',#39989,10.);
#11283=VECTOR('',#39992,10.);
#11284=VECTOR('',#39993,10.);
#11285=VECTOR('',#39996,10.);
#11286=VECTOR('',#39997,10.);
#11287=VECTOR('',#40006,10.);
#11288=VECTOR('',#40007,10.);
#11289=VECTOR('',#40008,10.);
#11290=VECTOR('',#40011,10.);
#11291=VECTOR('',#40012,10.);
#11292=VECTOR('',#40013,10.);
#11293=VECTOR('',#40016,10.);
#11294=VECTOR('',#40017,10.);
#11295=VECTOR('',#40018,10.);
#11296=VECTOR('',#40021,10.);
#11297=VECTOR('',#40022,10.);
#11298=VECTOR('',#40025,10.);
#11299=VECTOR('',#40026,10.);
#11300=VECTOR('',#40027,10.);
#11301=VECTOR('',#40030,10.);
#11302=VECTOR('',#40031,10.);
#11303=VECTOR('',#40034,10.);
#11304=VECTOR('',#40035,10.);
#11305=VECTOR('',#40038,10.);
#11306=VECTOR('',#40039,10.);
#11307=VECTOR('',#40042,10.);
#11308=VECTOR('',#40043,10.);
#11309=VECTOR('',#40046,10.);
#11310=VECTOR('',#40047,10.);
#11311=VECTOR('',#40050,10.);
#11312=VECTOR('',#40051,10.);
#11313=VECTOR('',#40054,10.);
#11314=VECTOR('',#40055,10.);
#11315=VECTOR('',#40064,10.);
#11316=VECTOR('',#40065,10.);
#11317=VECTOR('',#40066,10.);
#11318=VECTOR('',#40067,10.);
#11319=VECTOR('',#40070,10.);
#11320=VECTOR('',#40071,10.);
#11321=VECTOR('',#40074,10.);
#11322=VECTOR('',#40075,10.);
#11323=VECTOR('',#40076,10.);
#11324=VECTOR('',#40079,10.);
#11325=VECTOR('',#40080,10.);
#11326=VECTOR('',#40081,10.);
#11327=VECTOR('',#40084,10.);
#11328=VECTOR('',#40085,10.);
#11329=VECTOR('',#40088,10.);
#11330=VECTOR('',#40089,10.);
#11331=VECTOR('',#40092,10.);
#11332=VECTOR('',#40093,10.);
#11333=VECTOR('',#40096,10.);
#11334=VECTOR('',#40097,10.);
#11335=VECTOR('',#40098,10.);
#11336=VECTOR('',#40101,10.);
#11337=VECTOR('',#40102,10.);
#11338=VECTOR('',#40105,10.);
#11339=VECTOR('',#40106,10.);
#11340=VECTOR('',#40109,10.);
#11341=VECTOR('',#40110,10.);
#11342=VECTOR('',#40113,10.);
#11343=VECTOR('',#40120,10.);
#11344=VECTOR('',#40121,10.);
#11345=VECTOR('',#40122,10.);
#11346=VECTOR('',#40125,10.);
#11347=VECTOR('',#40126,10.);
#11348=VECTOR('',#40127,10.);
#11349=VECTOR('',#40130,10.);
#11350=VECTOR('',#40131,10.);
#11351=VECTOR('',#40132,10.);
#11352=VECTOR('',#40135,10.);
#11353=VECTOR('',#40136,10.);
#11354=VECTOR('',#40139,10.);
#11355=VECTOR('',#40140,10.);
#11356=VECTOR('',#40141,10.);
#11357=VECTOR('',#40144,10.);
#11358=VECTOR('',#40145,10.);
#11359=VECTOR('',#40148,10.);
#11360=VECTOR('',#40149,10.);
#11361=VECTOR('',#40152,10.);
#11362=VECTOR('',#40153,10.);
#11363=VECTOR('',#40156,10.);
#11364=VECTOR('',#40157,10.);
#11365=VECTOR('',#40160,10.);
#11366=VECTOR('',#40161,10.);
#11367=VECTOR('',#40164,10.);
#11368=VECTOR('',#40165,10.);
#11369=VECTOR('',#40168,10.);
#11370=VECTOR('',#40169,10.);
#11371=VECTOR('',#40178,10.);
#11372=VECTOR('',#40179,10.);
#11373=VECTOR('',#40180,10.);
#11374=VECTOR('',#40183,10.);
#11375=VECTOR('',#40184,10.);
#11376=VECTOR('',#40185,10.);
#11377=VECTOR('',#40186,10.);
#11378=VECTOR('',#40189,10.);
#11379=VECTOR('',#40190,10.);
#11380=VECTOR('',#40193,10.);
#11381=VECTOR('',#40194,10.);
#11382=VECTOR('',#40195,10.);
#11383=VECTOR('',#40198,10.);
#11384=VECTOR('',#40199,10.);
#11385=VECTOR('',#40200,10.);
#11386=VECTOR('',#40201,10.);
#11387=VECTOR('',#40204,10.);
#11388=VECTOR('',#40205,10.);
#11389=VECTOR('',#40208,10.);
#11390=VECTOR('',#40209,10.);
#11391=VECTOR('',#40212,10.);
#11392=VECTOR('',#40213,10.);
#11393=VECTOR('',#40214,10.);
#11394=VECTOR('',#40217,10.);
#11395=VECTOR('',#40220,10.);
#11396=VECTOR('',#40221,10.);
#11397=VECTOR('',#40224,10.);
#11398=VECTOR('',#40225,10.);
#11399=VECTOR('',#40232,10.);
#11400=VECTOR('',#40233,10.);
#11401=VECTOR('',#40234,10.);
#11402=VECTOR('',#40237,10.);
#11403=VECTOR('',#40238,10.);
#11404=VECTOR('',#40239,10.);
#11405=VECTOR('',#40242,10.);
#11406=VECTOR('',#40243,10.);
#11407=VECTOR('',#40244,10.);
#11408=VECTOR('',#40247,10.);
#11409=VECTOR('',#40248,10.);
#11410=VECTOR('',#40251,10.);
#11411=VECTOR('',#40252,10.);
#11412=VECTOR('',#40253,10.);
#11413=VECTOR('',#40256,10.);
#11414=VECTOR('',#40257,10.);
#11415=VECTOR('',#40260,10.);
#11416=VECTOR('',#40261,10.);
#11417=VECTOR('',#40264,10.);
#11418=VECTOR('',#40265,10.);
#11419=VECTOR('',#40268,10.);
#11420=VECTOR('',#40269,10.);
#11421=VECTOR('',#40272,10.);
#11422=VECTOR('',#40273,10.);
#11423=VECTOR('',#40276,10.);
#11424=VECTOR('',#40277,10.);
#11425=VECTOR('',#40280,10.);
#11426=VECTOR('',#40281,10.);
#11427=VECTOR('',#40290,10.);
#11428=VECTOR('',#40291,10.);
#11429=VECTOR('',#40292,10.);
#11430=VECTOR('',#40295,10.);
#11431=VECTOR('',#40296,10.);
#11432=VECTOR('',#40297,10.);
#11433=VECTOR('',#40300,10.);
#11434=VECTOR('',#40301,10.);
#11435=VECTOR('',#40302,10.);
#11436=VECTOR('',#40305,10.);
#11437=VECTOR('',#40306,10.);
#11438=VECTOR('',#40309,10.);
#11439=VECTOR('',#40310,10.);
#11440=VECTOR('',#40311,10.);
#11441=VECTOR('',#40314,10.);
#11442=VECTOR('',#40315,10.);
#11443=VECTOR('',#40318,10.);
#11444=VECTOR('',#40319,10.);
#11445=VECTOR('',#40322,10.);
#11446=VECTOR('',#40323,10.);
#11447=VECTOR('',#40326,10.);
#11448=VECTOR('',#40327,10.);
#11449=VECTOR('',#40330,10.);
#11450=VECTOR('',#40331,10.);
#11451=VECTOR('',#40334,10.);
#11452=VECTOR('',#40335,10.);
#11453=VECTOR('',#40338,10.);
#11454=VECTOR('',#40339,10.);
#11455=VECTOR('',#40348,10.);
#11456=VECTOR('',#40349,10.);
#11457=VECTOR('',#40350,10.);
#11458=VECTOR('',#40351,10.);
#11459=VECTOR('',#40354,10.);
#11460=VECTOR('',#40355,10.);
#11461=VECTOR('',#40358,10.);
#11462=VECTOR('',#40359,10.);
#11463=VECTOR('',#40360,10.);
#11464=VECTOR('',#40363,10.);
#11465=VECTOR('',#40364,10.);
#11466=VECTOR('',#40365,10.);
#11467=VECTOR('',#40368,10.);
#11468=VECTOR('',#40369,10.);
#11469=VECTOR('',#40372,10.);
#11470=VECTOR('',#40373,10.);
#11471=VECTOR('',#40376,10.);
#11472=VECTOR('',#40377,10.);
#11473=VECTOR('',#40380,10.);
#11474=VECTOR('',#40381,10.);
#11475=VECTOR('',#40382,10.);
#11476=VECTOR('',#40385,10.);
#11477=VECTOR('',#40386,10.);
#11478=VECTOR('',#40389,10.);
#11479=VECTOR('',#40390,10.);
#11480=VECTOR('',#40393,10.);
#11481=VECTOR('',#40394,10.);
#11482=VECTOR('',#40397,10.);
#11483=VECTOR('',#40404,10.);
#11484=VECTOR('',#40405,10.);
#11485=VECTOR('',#40406,10.);
#11486=VECTOR('',#40409,10.);
#11487=VECTOR('',#40410,10.);
#11488=VECTOR('',#40411,10.);
#11489=VECTOR('',#40414,10.);
#11490=VECTOR('',#40415,10.);
#11491=VECTOR('',#40416,10.);
#11492=VECTOR('',#40419,10.);
#11493=VECTOR('',#40420,10.);
#11494=VECTOR('',#40423,10.);
#11495=VECTOR('',#40424,10.);
#11496=VECTOR('',#40425,10.);
#11497=VECTOR('',#40428,10.);
#11498=VECTOR('',#40429,10.);
#11499=VECTOR('',#40432,10.);
#11500=VECTOR('',#40433,10.);
#11501=VECTOR('',#40436,10.);
#11502=VECTOR('',#40437,10.);
#11503=VECTOR('',#40440,10.);
#11504=VECTOR('',#40441,10.);
#11505=VECTOR('',#40444,10.);
#11506=VECTOR('',#40445,10.);
#11507=VECTOR('',#40448,10.);
#11508=VECTOR('',#40449,10.);
#11509=VECTOR('',#40452,10.);
#11510=VECTOR('',#40453,10.);
#11511=VECTOR('',#40462,10.);
#11512=VECTOR('',#40463,10.);
#11513=VECTOR('',#40464,10.);
#11514=VECTOR('',#40467,10.);
#11515=VECTOR('',#40468,10.);
#11516=VECTOR('',#40469,10.);
#11517=VECTOR('',#40470,10.);
#11518=VECTOR('',#40473,10.);
#11519=VECTOR('',#40474,10.);
#11520=VECTOR('',#40477,10.);
#11521=VECTOR('',#40478,10.);
#11522=VECTOR('',#40479,10.);
#11523=VECTOR('',#40482,10.);
#11524=VECTOR('',#40483,10.);
#11525=VECTOR('',#40484,10.);
#11526=VECTOR('',#40485,10.);
#11527=VECTOR('',#40488,10.);
#11528=VECTOR('',#40489,10.);
#11529=VECTOR('',#40492,10.);
#11530=VECTOR('',#40493,10.);
#11531=VECTOR('',#40496,10.);
#11532=VECTOR('',#40497,10.);
#11533=VECTOR('',#40498,10.);
#11534=VECTOR('',#40501,10.);
#11535=VECTOR('',#40504,10.);
#11536=VECTOR('',#40505,10.);
#11537=VECTOR('',#40508,10.);
#11538=VECTOR('',#40509,10.);
#11539=VECTOR('',#40516,10.);
#11540=VECTOR('',#40517,10.);
#11541=VECTOR('',#40518,10.);
#11542=VECTOR('',#40521,10.);
#11543=VECTOR('',#40522,10.);
#11544=VECTOR('',#40523,10.);
#11545=VECTOR('',#40526,10.);
#11546=VECTOR('',#40527,10.);
#11547=VECTOR('',#40528,10.);
#11548=VECTOR('',#40531,10.);
#11549=VECTOR('',#40532,10.);
#11550=VECTOR('',#40535,10.);
#11551=VECTOR('',#40536,10.);
#11552=VECTOR('',#40537,10.);
#11553=VECTOR('',#40540,10.);
#11554=VECTOR('',#40541,10.);
#11555=VECTOR('',#40544,10.);
#11556=VECTOR('',#40545,10.);
#11557=VECTOR('',#40548,10.);
#11558=VECTOR('',#40549,10.);
#11559=VECTOR('',#40552,10.);
#11560=VECTOR('',#40553,10.);
#11561=VECTOR('',#40556,10.);
#11562=VECTOR('',#40557,10.);
#11563=VECTOR('',#40560,10.);
#11564=VECTOR('',#40561,10.);
#11565=VECTOR('',#40564,10.);
#11566=VECTOR('',#40565,10.);
#11567=VECTOR('',#40574,10.);
#11568=VECTOR('',#40575,10.);
#11569=VECTOR('',#40576,10.);
#11570=VECTOR('',#40579,10.);
#11571=VECTOR('',#40580,10.);
#11572=VECTOR('',#40581,10.);
#11573=VECTOR('',#40584,10.);
#11574=VECTOR('',#40585,10.);
#11575=VECTOR('',#40586,10.);
#11576=VECTOR('',#40589,10.);
#11577=VECTOR('',#40590,10.);
#11578=VECTOR('',#40593,10.);
#11579=VECTOR('',#40594,10.);
#11580=VECTOR('',#40595,10.);
#11581=VECTOR('',#40598,10.);
#11582=VECTOR('',#40599,10.);
#11583=VECTOR('',#40602,10.);
#11584=VECTOR('',#40603,10.);
#11585=VECTOR('',#40606,10.);
#11586=VECTOR('',#40607,10.);
#11587=VECTOR('',#40610,10.);
#11588=VECTOR('',#40611,10.);
#11589=VECTOR('',#40614,10.);
#11590=VECTOR('',#40615,10.);
#11591=VECTOR('',#40618,10.);
#11592=VECTOR('',#40619,10.);
#11593=VECTOR('',#40622,10.);
#11594=VECTOR('',#40623,10.);
#11595=VECTOR('',#40632,10.);
#11596=VECTOR('',#40633,10.);
#11597=VECTOR('',#40634,10.);
#11598=VECTOR('',#40635,10.);
#11599=VECTOR('',#40638,10.);
#11600=VECTOR('',#40639,10.);
#11601=VECTOR('',#40642,10.);
#11602=VECTOR('',#40643,10.);
#11603=VECTOR('',#40644,10.);
#11604=VECTOR('',#40647,10.);
#11605=VECTOR('',#40648,10.);
#11606=VECTOR('',#40649,10.);
#11607=VECTOR('',#40652,10.);
#11608=VECTOR('',#40653,10.);
#11609=VECTOR('',#40656,10.);
#11610=VECTOR('',#40657,10.);
#11611=VECTOR('',#40660,10.);
#11612=VECTOR('',#40661,10.);
#11613=VECTOR('',#40664,10.);
#11614=VECTOR('',#40665,10.);
#11615=VECTOR('',#40666,10.);
#11616=VECTOR('',#40669,10.);
#11617=VECTOR('',#40670,10.);
#11618=VECTOR('',#40673,10.);
#11619=VECTOR('',#40674,10.);
#11620=VECTOR('',#40677,10.);
#11621=VECTOR('',#40678,10.);
#11622=VECTOR('',#40681,10.);
#11623=VECTOR('',#40688,10.);
#11624=VECTOR('',#40689,10.);
#11625=VECTOR('',#40690,10.);
#11626=VECTOR('',#40693,10.);
#11627=VECTOR('',#40694,10.);
#11628=VECTOR('',#40695,10.);
#11629=VECTOR('',#40698,10.);
#11630=VECTOR('',#40699,10.);
#11631=VECTOR('',#40700,10.);
#11632=VECTOR('',#40703,10.);
#11633=VECTOR('',#40704,10.);
#11634=VECTOR('',#40707,10.);
#11635=VECTOR('',#40708,10.);
#11636=VECTOR('',#40709,10.);
#11637=VECTOR('',#40712,10.);
#11638=VECTOR('',#40713,10.);
#11639=VECTOR('',#40716,10.);
#11640=VECTOR('',#40717,10.);
#11641=VECTOR('',#40720,10.);
#11642=VECTOR('',#40721,10.);
#11643=VECTOR('',#40724,10.);
#11644=VECTOR('',#40725,10.);
#11645=VECTOR('',#40728,10.);
#11646=VECTOR('',#40729,10.);
#11647=VECTOR('',#40732,10.);
#11648=VECTOR('',#40733,10.);
#11649=VECTOR('',#40736,10.);
#11650=VECTOR('',#40737,10.);
#11651=VECTOR('',#40746,10.);
#11652=VECTOR('',#40747,10.);
#11653=VECTOR('',#40748,10.);
#11654=VECTOR('',#40751,10.);
#11655=VECTOR('',#40752,10.);
#11656=VECTOR('',#40753,10.);
#11657=VECTOR('',#40754,10.);
#11658=VECTOR('',#40757,10.);
#11659=VECTOR('',#40758,10.);
#11660=VECTOR('',#40761,10.);
#11661=VECTOR('',#40762,10.);
#11662=VECTOR('',#40763,10.);
#11663=VECTOR('',#40766,10.);
#11664=VECTOR('',#40767,10.);
#11665=VECTOR('',#40768,10.);
#11666=VECTOR('',#40769,10.);
#11667=VECTOR('',#40772,10.);
#11668=VECTOR('',#40773,10.);
#11669=VECTOR('',#40776,10.);
#11670=VECTOR('',#40777,10.);
#11671=VECTOR('',#40780,10.);
#11672=VECTOR('',#40781,10.);
#11673=VECTOR('',#40782,10.);
#11674=VECTOR('',#40785,10.);
#11675=VECTOR('',#40788,10.);
#11676=VECTOR('',#40789,10.);
#11677=VECTOR('',#40792,10.);
#11678=VECTOR('',#40793,10.);
#11679=VECTOR('',#40800,10.);
#11680=VECTOR('',#40801,10.);
#11681=VECTOR('',#40802,10.);
#11682=VECTOR('',#40805,10.);
#11683=VECTOR('',#40806,10.);
#11684=VECTOR('',#40807,10.);
#11685=VECTOR('',#40810,10.);
#11686=VECTOR('',#40811,10.);
#11687=VECTOR('',#40812,10.);
#11688=VECTOR('',#40815,10.);
#11689=VECTOR('',#40816,10.);
#11690=VECTOR('',#40819,10.);
#11691=VECTOR('',#40820,10.);
#11692=VECTOR('',#40821,10.);
#11693=VECTOR('',#40824,10.);
#11694=VECTOR('',#40825,10.);
#11695=VECTOR('',#40828,10.);
#11696=VECTOR('',#40829,10.);
#11697=VECTOR('',#40832,10.);
#11698=VECTOR('',#40833,10.);
#11699=VECTOR('',#40836,10.);
#11700=VECTOR('',#40837,10.);
#11701=VECTOR('',#40840,10.);
#11702=VECTOR('',#40841,10.);
#11703=VECTOR('',#40844,10.);
#11704=VECTOR('',#40845,10.);
#11705=VECTOR('',#40848,10.);
#11706=VECTOR('',#40849,10.);
#11707=VECTOR('',#40858,10.);
#11708=VECTOR('',#40859,10.);
#11709=VECTOR('',#40860,10.);
#11710=VECTOR('',#40863,10.);
#11711=VECTOR('',#40864,10.);
#11712=VECTOR('',#40865,10.);
#11713=VECTOR('',#40868,10.);
#11714=VECTOR('',#40869,10.);
#11715=VECTOR('',#40870,10.);
#11716=VECTOR('',#40873,10.);
#11717=VECTOR('',#40874,10.);
#11718=VECTOR('',#40877,10.);
#11719=VECTOR('',#40878,10.);
#11720=VECTOR('',#40879,10.);
#11721=VECTOR('',#40882,10.);
#11722=VECTOR('',#40883,10.);
#11723=VECTOR('',#40886,10.);
#11724=VECTOR('',#40887,10.);
#11725=VECTOR('',#40890,10.);
#11726=VECTOR('',#40891,10.);
#11727=VECTOR('',#40894,10.);
#11728=VECTOR('',#40895,10.);
#11729=VECTOR('',#40898,10.);
#11730=VECTOR('',#40899,10.);
#11731=VECTOR('',#40902,10.);
#11732=VECTOR('',#40903,10.);
#11733=VECTOR('',#40906,10.);
#11734=VECTOR('',#40907,10.);
#11735=VECTOR('',#40916,10.);
#11736=VECTOR('',#40917,10.);
#11737=VECTOR('',#40918,10.);
#11738=VECTOR('',#40919,10.);
#11739=VECTOR('',#40922,10.);
#11740=VECTOR('',#40923,10.);
#11741=VECTOR('',#40926,10.);
#11742=VECTOR('',#40927,10.);
#11743=VECTOR('',#40928,10.);
#11744=VECTOR('',#40931,10.);
#11745=VECTOR('',#40932,10.);
#11746=VECTOR('',#40933,10.);
#11747=VECTOR('',#40936,10.);
#11748=VECTOR('',#40937,10.);
#11749=VECTOR('',#40940,10.);
#11750=VECTOR('',#40941,10.);
#11751=VECTOR('',#40944,10.);
#11752=VECTOR('',#40945,10.);
#11753=VECTOR('',#40948,10.);
#11754=VECTOR('',#40949,10.);
#11755=VECTOR('',#40950,10.);
#11756=VECTOR('',#40953,10.);
#11757=VECTOR('',#40954,10.);
#11758=VECTOR('',#40957,10.);
#11759=VECTOR('',#40958,10.);
#11760=VECTOR('',#40961,10.);
#11761=VECTOR('',#40962,10.);
#11762=VECTOR('',#40965,10.);
#11763=VECTOR('',#40972,10.);
#11764=VECTOR('',#40973,10.);
#11765=VECTOR('',#40974,10.);
#11766=VECTOR('',#40977,10.);
#11767=VECTOR('',#40978,10.);
#11768=VECTOR('',#40979,10.);
#11769=VECTOR('',#40982,10.);
#11770=VECTOR('',#40983,10.);
#11771=VECTOR('',#40984,10.);
#11772=VECTOR('',#40987,10.);
#11773=VECTOR('',#40988,10.);
#11774=VECTOR('',#40991,10.);
#11775=VECTOR('',#40992,10.);
#11776=VECTOR('',#40993,10.);
#11777=VECTOR('',#40996,10.);
#11778=VECTOR('',#40997,10.);
#11779=VECTOR('',#41000,10.);
#11780=VECTOR('',#41001,10.);
#11781=VECTOR('',#41004,10.);
#11782=VECTOR('',#41005,10.);
#11783=VECTOR('',#41008,10.);
#11784=VECTOR('',#41009,10.);
#11785=VECTOR('',#41012,10.);
#11786=VECTOR('',#41013,10.);
#11787=VECTOR('',#41016,10.);
#11788=VECTOR('',#41017,10.);
#11789=VECTOR('',#41020,10.);
#11790=VECTOR('',#41021,10.);
#11791=VECTOR('',#41030,10.);
#11792=VECTOR('',#41031,10.);
#11793=VECTOR('',#41032,10.);
#11794=VECTOR('',#41035,10.);
#11795=VECTOR('',#41036,10.);
#11796=VECTOR('',#41037,10.);
#11797=VECTOR('',#41038,10.);
#11798=VECTOR('',#41041,10.);
#11799=VECTOR('',#41042,10.);
#11800=VECTOR('',#41045,10.);
#11801=VECTOR('',#41046,10.);
#11802=VECTOR('',#41047,10.);
#11803=VECTOR('',#41050,10.);
#11804=VECTOR('',#41051,10.);
#11805=VECTOR('',#41052,10.);
#11806=VECTOR('',#41053,10.);
#11807=VECTOR('',#41056,10.);
#11808=VECTOR('',#41057,10.);
#11809=VECTOR('',#41060,10.);
#11810=VECTOR('',#41061,10.);
#11811=VECTOR('',#41064,10.);
#11812=VECTOR('',#41065,10.);
#11813=VECTOR('',#41066,10.);
#11814=VECTOR('',#41069,10.);
#11815=VECTOR('',#41072,10.);
#11816=VECTOR('',#41073,10.);
#11817=VECTOR('',#41076,10.);
#11818=VECTOR('',#41077,10.);
#11819=VECTOR('',#41084,10.);
#11820=VECTOR('',#41085,10.);
#11821=VECTOR('',#41086,10.);
#11822=VECTOR('',#41089,10.);
#11823=VECTOR('',#41090,10.);
#11824=VECTOR('',#41091,10.);
#11825=VECTOR('',#41094,10.);
#11826=VECTOR('',#41095,10.);
#11827=VECTOR('',#41096,10.);
#11828=VECTOR('',#41099,10.);
#11829=VECTOR('',#41100,10.);
#11830=VECTOR('',#41103,10.);
#11831=VECTOR('',#41104,10.);
#11832=VECTOR('',#41105,10.);
#11833=VECTOR('',#41108,10.);
#11834=VECTOR('',#41109,10.);
#11835=VECTOR('',#41112,10.);
#11836=VECTOR('',#41113,10.);
#11837=VECTOR('',#41116,10.);
#11838=VECTOR('',#41117,10.);
#11839=VECTOR('',#41120,10.);
#11840=VECTOR('',#41121,10.);
#11841=VECTOR('',#41124,10.);
#11842=VECTOR('',#41125,10.);
#11843=VECTOR('',#41128,10.);
#11844=VECTOR('',#41129,10.);
#11845=VECTOR('',#41132,10.);
#11846=VECTOR('',#41133,10.);
#11847=VECTOR('',#41142,10.);
#11848=VECTOR('',#41143,10.);
#11849=VECTOR('',#41144,10.);
#11850=VECTOR('',#41147,10.);
#11851=VECTOR('',#41148,10.);
#11852=VECTOR('',#41149,10.);
#11853=VECTOR('',#41152,10.);
#11854=VECTOR('',#41153,10.);
#11855=VECTOR('',#41154,10.);
#11856=VECTOR('',#41157,10.);
#11857=VECTOR('',#41158,10.);
#11858=VECTOR('',#41161,10.);
#11859=VECTOR('',#41162,10.);
#11860=VECTOR('',#41163,10.);
#11861=VECTOR('',#41166,10.);
#11862=VECTOR('',#41167,10.);
#11863=VECTOR('',#41170,10.);
#11864=VECTOR('',#41171,10.);
#11865=VECTOR('',#41174,10.);
#11866=VECTOR('',#41175,10.);
#11867=VECTOR('',#41178,10.);
#11868=VECTOR('',#41179,10.);
#11869=VECTOR('',#41182,10.);
#11870=VECTOR('',#41183,10.);
#11871=VECTOR('',#41186,10.);
#11872=VECTOR('',#41187,10.);
#11873=VECTOR('',#41190,10.);
#11874=VECTOR('',#41191,10.);
#11875=VECTOR('',#41200,10.);
#11876=VECTOR('',#41201,10.);
#11877=VECTOR('',#41202,10.);
#11878=VECTOR('',#41203,10.);
#11879=VECTOR('',#41206,10.);
#11880=VECTOR('',#41207,10.);
#11881=VECTOR('',#41210,10.);
#11882=VECTOR('',#41211,10.);
#11883=VECTOR('',#41212,10.);
#11884=VECTOR('',#41215,10.);
#11885=VECTOR('',#41216,10.);
#11886=VECTOR('',#41217,10.);
#11887=VECTOR('',#41220,10.);
#11888=VECTOR('',#41221,10.);
#11889=VECTOR('',#41224,10.);
#11890=VECTOR('',#41225,10.);
#11891=VECTOR('',#41228,10.);
#11892=VECTOR('',#41229,10.);
#11893=VECTOR('',#41232,10.);
#11894=VECTOR('',#41233,10.);
#11895=VECTOR('',#41234,10.);
#11896=VECTOR('',#41237,10.);
#11897=VECTOR('',#41238,10.);
#11898=VECTOR('',#41241,10.);
#11899=VECTOR('',#41242,10.);
#11900=VECTOR('',#41245,10.);
#11901=VECTOR('',#41246,10.);
#11902=VECTOR('',#41249,10.);
#11903=VECTOR('',#41256,10.);
#11904=VECTOR('',#41257,10.);
#11905=VECTOR('',#41258,10.);
#11906=VECTOR('',#41261,10.);
#11907=VECTOR('',#41262,10.);
#11908=VECTOR('',#41263,10.);
#11909=VECTOR('',#41266,10.);
#11910=VECTOR('',#41267,10.);
#11911=VECTOR('',#41268,10.);
#11912=VECTOR('',#41271,10.);
#11913=VECTOR('',#41272,10.);
#11914=VECTOR('',#41275,10.);
#11915=VECTOR('',#41276,10.);
#11916=VECTOR('',#41277,10.);
#11917=VECTOR('',#41280,10.);
#11918=VECTOR('',#41281,10.);
#11919=VECTOR('',#41284,10.);
#11920=VECTOR('',#41285,10.);
#11921=VECTOR('',#41288,10.);
#11922=VECTOR('',#41289,10.);
#11923=VECTOR('',#41292,10.);
#11924=VECTOR('',#41293,10.);
#11925=VECTOR('',#41296,10.);
#11926=VECTOR('',#41297,10.);
#11927=VECTOR('',#41300,10.);
#11928=VECTOR('',#41301,10.);
#11929=VECTOR('',#41304,10.);
#11930=VECTOR('',#41305,10.);
#11931=VECTOR('',#41314,10.);
#11932=VECTOR('',#41315,10.);
#11933=VECTOR('',#41316,10.);
#11934=VECTOR('',#41319,10.);
#11935=VECTOR('',#41320,10.);
#11936=VECTOR('',#41321,10.);
#11937=VECTOR('',#41322,10.);
#11938=VECTOR('',#41325,10.);
#11939=VECTOR('',#41326,10.);
#11940=VECTOR('',#41329,10.);
#11941=VECTOR('',#41330,10.);
#11942=VECTOR('',#41331,10.);
#11943=VECTOR('',#41334,10.);
#11944=VECTOR('',#41335,10.);
#11945=VECTOR('',#41336,10.);
#11946=VECTOR('',#41337,10.);
#11947=VECTOR('',#41340,10.);
#11948=VECTOR('',#41341,10.);
#11949=VECTOR('',#41344,10.);
#11950=VECTOR('',#41345,10.);
#11951=VECTOR('',#41348,10.);
#11952=VECTOR('',#41349,10.);
#11953=VECTOR('',#41350,10.);
#11954=VECTOR('',#41353,10.);
#11955=VECTOR('',#41356,10.);
#11956=VECTOR('',#41357,10.);
#11957=VECTOR('',#41360,10.);
#11958=VECTOR('',#41361,10.);
#11959=VECTOR('',#41368,10.);
#11960=VECTOR('',#41369,10.);
#11961=VECTOR('',#41370,10.);
#11962=VECTOR('',#41373,10.);
#11963=VECTOR('',#41374,10.);
#11964=VECTOR('',#41375,10.);
#11965=VECTOR('',#41378,10.);
#11966=VECTOR('',#41379,10.);
#11967=VECTOR('',#41380,10.);
#11968=VECTOR('',#41383,10.);
#11969=VECTOR('',#41384,10.);
#11970=VECTOR('',#41387,10.);
#11971=VECTOR('',#41388,10.);
#11972=VECTOR('',#41389,10.);
#11973=VECTOR('',#41392,10.);
#11974=VECTOR('',#41393,10.);
#11975=VECTOR('',#41396,10.);
#11976=VECTOR('',#41397,10.);
#11977=VECTOR('',#41400,10.);
#11978=VECTOR('',#41401,10.);
#11979=VECTOR('',#41404,10.);
#11980=VECTOR('',#41405,10.);
#11981=VECTOR('',#41408,10.);
#11982=VECTOR('',#41409,10.);
#11983=VECTOR('',#41412,10.);
#11984=VECTOR('',#41413,10.);
#11985=VECTOR('',#41416,10.);
#11986=VECTOR('',#41417,10.);
#11987=VECTOR('',#41426,10.);
#11988=VECTOR('',#41427,10.);
#11989=VECTOR('',#41428,10.);
#11990=VECTOR('',#41431,10.);
#11991=VECTOR('',#41432,10.);
#11992=VECTOR('',#41433,10.);
#11993=VECTOR('',#41436,10.);
#11994=VECTOR('',#41437,10.);
#11995=VECTOR('',#41438,10.);
#11996=VECTOR('',#41441,10.);
#11997=VECTOR('',#41442,10.);
#11998=VECTOR('',#41445,10.);
#11999=VECTOR('',#41446,10.);
#12000=VECTOR('',#41447,10.);
#12001=VECTOR('',#41450,10.);
#12002=VECTOR('',#41451,10.);
#12003=VECTOR('',#41454,10.);
#12004=VECTOR('',#41455,10.);
#12005=VECTOR('',#41458,10.);
#12006=VECTOR('',#41459,10.);
#12007=VECTOR('',#41462,10.);
#12008=VECTOR('',#41463,10.);
#12009=VECTOR('',#41466,10.);
#12010=VECTOR('',#41467,10.);
#12011=VECTOR('',#41470,10.);
#12012=VECTOR('',#41471,10.);
#12013=VECTOR('',#41474,10.);
#12014=VECTOR('',#41475,10.);
#12015=VECTOR('',#41484,10.);
#12016=VECTOR('',#41485,10.);
#12017=VECTOR('',#41486,10.);
#12018=VECTOR('',#41487,10.);
#12019=VECTOR('',#41490,10.);
#12020=VECTOR('',#41491,10.);
#12021=VECTOR('',#41494,10.);
#12022=VECTOR('',#41495,10.);
#12023=VECTOR('',#41496,10.);
#12024=VECTOR('',#41499,10.);
#12025=VECTOR('',#41500,10.);
#12026=VECTOR('',#41501,10.);
#12027=VECTOR('',#41504,10.);
#12028=VECTOR('',#41505,10.);
#12029=VECTOR('',#41508,10.);
#12030=VECTOR('',#41509,10.);
#12031=VECTOR('',#41512,10.);
#12032=VECTOR('',#41513,10.);
#12033=VECTOR('',#41516,10.);
#12034=VECTOR('',#41517,10.);
#12035=VECTOR('',#41518,10.);
#12036=VECTOR('',#41521,10.);
#12037=VECTOR('',#41522,10.);
#12038=VECTOR('',#41525,10.);
#12039=VECTOR('',#41526,10.);
#12040=VECTOR('',#41529,10.);
#12041=VECTOR('',#41530,10.);
#12042=VECTOR('',#41533,10.);
#12043=VECTOR('',#41540,10.);
#12044=VECTOR('',#41541,10.);
#12045=VECTOR('',#41542,10.);
#12046=VECTOR('',#41545,10.);
#12047=VECTOR('',#41546,10.);
#12048=VECTOR('',#41547,10.);
#12049=VECTOR('',#41550,10.);
#12050=VECTOR('',#41551,10.);
#12051=VECTOR('',#41552,10.);
#12052=VECTOR('',#41555,10.);
#12053=VECTOR('',#41556,10.);
#12054=VECTOR('',#41559,10.);
#12055=VECTOR('',#41560,10.);
#12056=VECTOR('',#41561,10.);
#12057=VECTOR('',#41564,10.);
#12058=VECTOR('',#41565,10.);
#12059=VECTOR('',#41568,10.);
#12060=VECTOR('',#41569,10.);
#12061=VECTOR('',#41572,10.);
#12062=VECTOR('',#41573,10.);
#12063=VECTOR('',#41576,10.);
#12064=VECTOR('',#41577,10.);
#12065=VECTOR('',#41580,10.);
#12066=VECTOR('',#41581,10.);
#12067=VECTOR('',#41584,10.);
#12068=VECTOR('',#41585,10.);
#12069=VECTOR('',#41588,10.);
#12070=VECTOR('',#41589,10.);
#12071=VECTOR('',#41598,10.);
#12072=VECTOR('',#41599,10.);
#12073=VECTOR('',#41600,10.);
#12074=VECTOR('',#41603,10.);
#12075=VECTOR('',#41604,10.);
#12076=VECTOR('',#41605,10.);
#12077=VECTOR('',#41606,10.);
#12078=VECTOR('',#41609,10.);
#12079=VECTOR('',#41610,10.);
#12080=VECTOR('',#41613,10.);
#12081=VECTOR('',#41614,10.);
#12082=VECTOR('',#41615,10.);
#12083=VECTOR('',#41618,10.);
#12084=VECTOR('',#41619,10.);
#12085=VECTOR('',#41620,10.);
#12086=VECTOR('',#41621,10.);
#12087=VECTOR('',#41624,10.);
#12088=VECTOR('',#41625,10.);
#12089=VECTOR('',#41628,10.);
#12090=VECTOR('',#41629,10.);
#12091=VECTOR('',#41632,10.);
#12092=VECTOR('',#41633,10.);
#12093=VECTOR('',#41634,10.);
#12094=VECTOR('',#41637,10.);
#12095=VECTOR('',#41640,10.);
#12096=VECTOR('',#41641,10.);
#12097=VECTOR('',#41644,10.);
#12098=VECTOR('',#41645,10.);
#12099=VECTOR('',#41652,10.);
#12100=VECTOR('',#41653,10.);
#12101=VECTOR('',#41654,10.);
#12102=VECTOR('',#41657,10.);
#12103=VECTOR('',#41658,10.);
#12104=VECTOR('',#41659,10.);
#12105=VECTOR('',#41662,10.);
#12106=VECTOR('',#41663,10.);
#12107=VECTOR('',#41664,10.);
#12108=VECTOR('',#41667,10.);
#12109=VECTOR('',#41668,10.);
#12110=VECTOR('',#41671,10.);
#12111=VECTOR('',#41672,10.);
#12112=VECTOR('',#41673,10.);
#12113=VECTOR('',#41676,10.);
#12114=VECTOR('',#41677,10.);
#12115=VECTOR('',#41680,10.);
#12116=VECTOR('',#41681,10.);
#12117=VECTOR('',#41684,10.);
#12118=VECTOR('',#41685,10.);
#12119=VECTOR('',#41688,10.);
#12120=VECTOR('',#41689,10.);
#12121=VECTOR('',#41692,10.);
#12122=VECTOR('',#41693,10.);
#12123=VECTOR('',#41696,10.);
#12124=VECTOR('',#41697,10.);
#12125=VECTOR('',#41700,10.);
#12126=VECTOR('',#41701,10.);
#12127=VECTOR('',#41710,10.);
#12128=VECTOR('',#41711,10.);
#12129=VECTOR('',#41712,10.);
#12130=VECTOR('',#41715,10.);
#12131=VECTOR('',#41716,10.);
#12132=VECTOR('',#41717,10.);
#12133=VECTOR('',#41720,10.);
#12134=VECTOR('',#41721,10.);
#12135=VECTOR('',#41722,10.);
#12136=VECTOR('',#41725,10.);
#12137=VECTOR('',#41726,10.);
#12138=VECTOR('',#41729,10.);
#12139=VECTOR('',#41730,10.);
#12140=VECTOR('',#41731,10.);
#12141=VECTOR('',#41734,10.);
#12142=VECTOR('',#41735,10.);
#12143=VECTOR('',#41738,10.);
#12144=VECTOR('',#41739,10.);
#12145=VECTOR('',#41742,10.);
#12146=VECTOR('',#41743,10.);
#12147=VECTOR('',#41746,10.);
#12148=VECTOR('',#41747,10.);
#12149=VECTOR('',#41750,10.);
#12150=VECTOR('',#41751,10.);
#12151=VECTOR('',#41754,10.);
#12152=VECTOR('',#41755,10.);
#12153=VECTOR('',#41758,10.);
#12154=VECTOR('',#41759,10.);
#12155=VECTOR('',#41768,10.);
#12156=VECTOR('',#41769,10.);
#12157=VECTOR('',#41770,10.);
#12158=VECTOR('',#41771,10.);
#12159=VECTOR('',#41774,10.);
#12160=VECTOR('',#41775,10.);
#12161=VECTOR('',#41778,10.);
#12162=VECTOR('',#41779,10.);
#12163=VECTOR('',#41780,10.);
#12164=VECTOR('',#41783,10.);
#12165=VECTOR('',#41784,10.);
#12166=VECTOR('',#41785,10.);
#12167=VECTOR('',#41788,10.);
#12168=VECTOR('',#41789,10.);
#12169=VECTOR('',#41792,10.);
#12170=VECTOR('',#41793,10.);
#12171=VECTOR('',#41796,10.);
#12172=VECTOR('',#41797,10.);
#12173=VECTOR('',#41800,10.);
#12174=VECTOR('',#41801,10.);
#12175=VECTOR('',#41802,10.);
#12176=VECTOR('',#41805,10.);
#12177=VECTOR('',#41806,10.);
#12178=VECTOR('',#41809,10.);
#12179=VECTOR('',#41810,10.);
#12180=VECTOR('',#41813,10.);
#12181=VECTOR('',#41814,10.);
#12182=VECTOR('',#41817,10.);
#12183=VECTOR('',#41824,10.);
#12184=VECTOR('',#41825,10.);
#12185=VECTOR('',#41826,10.);
#12186=VECTOR('',#41829,10.);
#12187=VECTOR('',#41830,10.);
#12188=VECTOR('',#41831,10.);
#12189=VECTOR('',#41834,10.);
#12190=VECTOR('',#41835,10.);
#12191=VECTOR('',#41836,10.);
#12192=VECTOR('',#41839,10.);
#12193=VECTOR('',#41840,10.);
#12194=VECTOR('',#41843,10.);
#12195=VECTOR('',#41844,10.);
#12196=VECTOR('',#41845,10.);
#12197=VECTOR('',#41848,10.);
#12198=VECTOR('',#41849,10.);
#12199=VECTOR('',#41852,10.);
#12200=VECTOR('',#41853,10.);
#12201=VECTOR('',#41856,10.);
#12202=VECTOR('',#41857,10.);
#12203=VECTOR('',#41860,10.);
#12204=VECTOR('',#41861,10.);
#12205=VECTOR('',#41864,10.);
#12206=VECTOR('',#41865,10.);
#12207=VECTOR('',#41868,10.);
#12208=VECTOR('',#41869,10.);
#12209=VECTOR('',#41872,10.);
#12210=VECTOR('',#41873,10.);
#12211=VECTOR('',#41882,10.);
#12212=VECTOR('',#41883,10.);
#12213=VECTOR('',#41884,10.);
#12214=VECTOR('',#41887,10.);
#12215=VECTOR('',#41888,10.);
#12216=VECTOR('',#41889,10.);
#12217=VECTOR('',#41890,10.);
#12218=VECTOR('',#41893,10.);
#12219=VECTOR('',#41894,10.);
#12220=VECTOR('',#41897,10.);
#12221=VECTOR('',#41898,10.);
#12222=VECTOR('',#41899,10.);
#12223=VECTOR('',#41902,10.);
#12224=VECTOR('',#41903,10.);
#12225=VECTOR('',#41904,10.);
#12226=VECTOR('',#41905,10.);
#12227=VECTOR('',#41908,10.);
#12228=VECTOR('',#41909,10.);
#12229=VECTOR('',#41912,10.);
#12230=VECTOR('',#41913,10.);
#12231=VECTOR('',#41916,10.);
#12232=VECTOR('',#41917,10.);
#12233=VECTOR('',#41918,10.);
#12234=VECTOR('',#41921,10.);
#12235=VECTOR('',#41924,10.);
#12236=VECTOR('',#41925,10.);
#12237=VECTOR('',#41928,10.);
#12238=VECTOR('',#41929,10.);
#12239=VECTOR('',#41936,10.);
#12240=VECTOR('',#41937,10.);
#12241=VECTOR('',#41938,10.);
#12242=VECTOR('',#41941,10.);
#12243=VECTOR('',#41942,10.);
#12244=VECTOR('',#41943,10.);
#12245=VECTOR('',#41946,10.);
#12246=VECTOR('',#41947,10.);
#12247=VECTOR('',#41948,10.);
#12248=VECTOR('',#41951,10.);
#12249=VECTOR('',#41952,10.);
#12250=VECTOR('',#41955,10.);
#12251=VECTOR('',#41956,10.);
#12252=VECTOR('',#41957,10.);
#12253=VECTOR('',#41960,10.);
#12254=VECTOR('',#41961,10.);
#12255=VECTOR('',#41964,10.);
#12256=VECTOR('',#41965,10.);
#12257=VECTOR('',#41968,10.);
#12258=VECTOR('',#41969,10.);
#12259=VECTOR('',#41972,10.);
#12260=VECTOR('',#41973,10.);
#12261=VECTOR('',#41976,10.);
#12262=VECTOR('',#41977,10.);
#12263=VECTOR('',#41980,10.);
#12264=VECTOR('',#41981,10.);
#12265=VECTOR('',#41984,10.);
#12266=VECTOR('',#41985,10.);
#12267=VECTOR('',#41994,10.);
#12268=VECTOR('',#41995,10.);
#12269=VECTOR('',#41996,10.);
#12270=VECTOR('',#41999,10.);
#12271=VECTOR('',#42000,10.);
#12272=VECTOR('',#42001,10.);
#12273=VECTOR('',#42004,10.);
#12274=VECTOR('',#42005,10.);
#12275=VECTOR('',#42006,10.);
#12276=VECTOR('',#42009,10.);
#12277=VECTOR('',#42010,10.);
#12278=VECTOR('',#42013,10.);
#12279=VECTOR('',#42014,10.);
#12280=VECTOR('',#42015,10.);
#12281=VECTOR('',#42018,10.);
#12282=VECTOR('',#42019,10.);
#12283=VECTOR('',#42022,10.);
#12284=VECTOR('',#42023,10.);
#12285=VECTOR('',#42026,10.);
#12286=VECTOR('',#42027,10.);
#12287=VECTOR('',#42030,10.);
#12288=VECTOR('',#42031,10.);
#12289=VECTOR('',#42034,10.);
#12290=VECTOR('',#42035,10.);
#12291=VECTOR('',#42038,10.);
#12292=VECTOR('',#42039,10.);
#12293=VECTOR('',#42042,10.);
#12294=VECTOR('',#42043,10.);
#12295=VECTOR('',#42052,10.);
#12296=VECTOR('',#42053,10.);
#12297=VECTOR('',#42054,10.);
#12298=VECTOR('',#42055,10.);
#12299=VECTOR('',#42058,10.);
#12300=VECTOR('',#42059,10.);
#12301=VECTOR('',#42062,10.);
#12302=VECTOR('',#42063,10.);
#12303=VECTOR('',#42064,10.);
#12304=VECTOR('',#42067,10.);
#12305=VECTOR('',#42068,10.);
#12306=VECTOR('',#42069,10.);
#12307=VECTOR('',#42072,10.);
#12308=VECTOR('',#42073,10.);
#12309=VECTOR('',#42076,10.);
#12310=VECTOR('',#42077,10.);
#12311=VECTOR('',#42080,10.);
#12312=VECTOR('',#42081,10.);
#12313=VECTOR('',#42084,10.);
#12314=VECTOR('',#42085,10.);
#12315=VECTOR('',#42086,10.);
#12316=VECTOR('',#42089,10.);
#12317=VECTOR('',#42090,10.);
#12318=VECTOR('',#42093,10.);
#12319=VECTOR('',#42094,10.);
#12320=VECTOR('',#42097,10.);
#12321=VECTOR('',#42098,10.);
#12322=VECTOR('',#42101,10.);
#12323=VECTOR('',#42108,10.);
#12324=VECTOR('',#42109,10.);
#12325=VECTOR('',#42110,10.);
#12326=VECTOR('',#42113,10.);
#12327=VECTOR('',#42114,10.);
#12328=VECTOR('',#42115,10.);
#12329=VECTOR('',#42118,10.);
#12330=VECTOR('',#42119,10.);
#12331=VECTOR('',#42120,10.);
#12332=VECTOR('',#42123,10.);
#12333=VECTOR('',#42124,10.);
#12334=VECTOR('',#42127,10.);
#12335=VECTOR('',#42128,10.);
#12336=VECTOR('',#42129,10.);
#12337=VECTOR('',#42132,10.);
#12338=VECTOR('',#42133,10.);
#12339=VECTOR('',#42136,10.);
#12340=VECTOR('',#42137,10.);
#12341=VECTOR('',#42140,10.);
#12342=VECTOR('',#42141,10.);
#12343=VECTOR('',#42144,10.);
#12344=VECTOR('',#42145,10.);
#12345=VECTOR('',#42148,10.);
#12346=VECTOR('',#42149,10.);
#12347=VECTOR('',#42152,10.);
#12348=VECTOR('',#42153,10.);
#12349=VECTOR('',#42156,10.);
#12350=VECTOR('',#42157,10.);
#12351=VECTOR('',#42166,10.);
#12352=VECTOR('',#42167,10.);
#12353=VECTOR('',#42168,10.);
#12354=VECTOR('',#42171,10.);
#12355=VECTOR('',#42172,10.);
#12356=VECTOR('',#42173,10.);
#12357=VECTOR('',#42174,10.);
#12358=VECTOR('',#42177,10.);
#12359=VECTOR('',#42178,10.);
#12360=VECTOR('',#42181,10.);
#12361=VECTOR('',#42182,10.);
#12362=VECTOR('',#42183,10.);
#12363=VECTOR('',#42186,10.);
#12364=VECTOR('',#42187,10.);
#12365=VECTOR('',#42188,10.);
#12366=VECTOR('',#42189,10.);
#12367=VECTOR('',#42192,10.);
#12368=VECTOR('',#42193,10.);
#12369=VECTOR('',#42196,10.);
#12370=VECTOR('',#42197,10.);
#12371=VECTOR('',#42200,10.);
#12372=VECTOR('',#42201,10.);
#12373=VECTOR('',#42202,10.);
#12374=VECTOR('',#42205,10.);
#12375=VECTOR('',#42208,10.);
#12376=VECTOR('',#42209,10.);
#12377=VECTOR('',#42212,10.);
#12378=VECTOR('',#42213,10.);
#12379=VECTOR('',#42220,10.);
#12380=VECTOR('',#42221,10.);
#12381=VECTOR('',#42222,10.);
#12382=VECTOR('',#42225,10.);
#12383=VECTOR('',#42226,10.);
#12384=VECTOR('',#42227,10.);
#12385=VECTOR('',#42230,10.);
#12386=VECTOR('',#42231,10.);
#12387=VECTOR('',#42232,10.);
#12388=VECTOR('',#42235,10.);
#12389=VECTOR('',#42236,10.);
#12390=VECTOR('',#42239,10.);
#12391=VECTOR('',#42240,10.);
#12392=VECTOR('',#42241,10.);
#12393=VECTOR('',#42244,10.);
#12394=VECTOR('',#42245,10.);
#12395=VECTOR('',#42248,10.);
#12396=VECTOR('',#42249,10.);
#12397=VECTOR('',#42252,10.);
#12398=VECTOR('',#42253,10.);
#12399=VECTOR('',#42256,10.);
#12400=VECTOR('',#42257,10.);
#12401=VECTOR('',#42260,10.);
#12402=VECTOR('',#42261,10.);
#12403=VECTOR('',#42264,10.);
#12404=VECTOR('',#42265,10.);
#12405=VECTOR('',#42268,10.);
#12406=VECTOR('',#42269,10.);
#12407=VECTOR('',#42278,10.);
#12408=VECTOR('',#42279,10.);
#12409=VECTOR('',#42280,10.);
#12410=VECTOR('',#42283,10.);
#12411=VECTOR('',#42284,10.);
#12412=VECTOR('',#42285,10.);
#12413=VECTOR('',#42288,10.);
#12414=VECTOR('',#42289,10.);
#12415=VECTOR('',#42290,10.);
#12416=VECTOR('',#42293,10.);
#12417=VECTOR('',#42294,10.);
#12418=VECTOR('',#42297,10.);
#12419=VECTOR('',#42298,10.);
#12420=VECTOR('',#42299,10.);
#12421=VECTOR('',#42302,10.);
#12422=VECTOR('',#42303,10.);
#12423=VECTOR('',#42306,10.);
#12424=VECTOR('',#42307,10.);
#12425=VECTOR('',#42310,10.);
#12426=VECTOR('',#42311,10.);
#12427=VECTOR('',#42314,10.);
#12428=VECTOR('',#42315,10.);
#12429=VECTOR('',#42318,10.);
#12430=VECTOR('',#42319,10.);
#12431=VECTOR('',#42322,10.);
#12432=VECTOR('',#42323,10.);
#12433=VECTOR('',#42326,10.);
#12434=VECTOR('',#42327,10.);
#12435=VECTOR('',#42336,10.);
#12436=VECTOR('',#42337,10.);
#12437=VECTOR('',#42338,10.);
#12438=VECTOR('',#42339,10.);
#12439=VECTOR('',#42342,10.);
#12440=VECTOR('',#42343,10.);
#12441=VECTOR('',#42346,10.);
#12442=VECTOR('',#42347,10.);
#12443=VECTOR('',#42348,10.);
#12444=VECTOR('',#42351,10.);
#12445=VECTOR('',#42352,10.);
#12446=VECTOR('',#42353,10.);
#12447=VECTOR('',#42356,10.);
#12448=VECTOR('',#42357,10.);
#12449=VECTOR('',#42360,10.);
#12450=VECTOR('',#42361,10.);
#12451=VECTOR('',#42364,10.);
#12452=VECTOR('',#42365,10.);
#12453=VECTOR('',#42368,10.);
#12454=VECTOR('',#42369,10.);
#12455=VECTOR('',#42370,10.);
#12456=VECTOR('',#42373,10.);
#12457=VECTOR('',#42374,10.);
#12458=VECTOR('',#42377,10.);
#12459=VECTOR('',#42378,10.);
#12460=VECTOR('',#42381,10.);
#12461=VECTOR('',#42382,10.);
#12462=VECTOR('',#42385,10.);
#12463=VECTOR('',#42392,10.);
#12464=VECTOR('',#42393,10.);
#12465=VECTOR('',#42394,10.);
#12466=VECTOR('',#42397,10.);
#12467=VECTOR('',#42398,10.);
#12468=VECTOR('',#42399,10.);
#12469=VECTOR('',#42402,10.);
#12470=VECTOR('',#42403,10.);
#12471=VECTOR('',#42404,10.);
#12472=VECTOR('',#42407,10.);
#12473=VECTOR('',#42408,10.);
#12474=VECTOR('',#42411,10.);
#12475=VECTOR('',#42412,10.);
#12476=VECTOR('',#42413,10.);
#12477=VECTOR('',#42416,10.);
#12478=VECTOR('',#42417,10.);
#12479=VECTOR('',#42420,10.);
#12480=VECTOR('',#42421,10.);
#12481=VECTOR('',#42424,10.);
#12482=VECTOR('',#42425,10.);
#12483=VECTOR('',#42428,10.);
#12484=VECTOR('',#42429,10.);
#12485=VECTOR('',#42432,10.);
#12486=VECTOR('',#42433,10.);
#12487=VECTOR('',#42436,10.);
#12488=VECTOR('',#42437,10.);
#12489=VECTOR('',#42440,10.);
#12490=VECTOR('',#42441,10.);
#12491=VECTOR('',#42450,10.);
#12492=VECTOR('',#42451,10.);
#12493=VECTOR('',#42452,10.);
#12494=VECTOR('',#42455,10.);
#12495=VECTOR('',#42456,10.);
#12496=VECTOR('',#42457,10.);
#12497=VECTOR('',#42458,10.);
#12498=VECTOR('',#42461,10.);
#12499=VECTOR('',#42462,10.);
#12500=VECTOR('',#42465,10.);
#12501=VECTOR('',#42466,10.);
#12502=VECTOR('',#42467,10.);
#12503=VECTOR('',#42470,10.);
#12504=VECTOR('',#42471,10.);
#12505=VECTOR('',#42472,10.);
#12506=VECTOR('',#42473,10.);
#12507=VECTOR('',#42476,10.);
#12508=VECTOR('',#42477,10.);
#12509=VECTOR('',#42480,10.);
#12510=VECTOR('',#42481,10.);
#12511=VECTOR('',#42484,10.);
#12512=VECTOR('',#42485,10.);
#12513=VECTOR('',#42486,10.);
#12514=VECTOR('',#42489,10.);
#12515=VECTOR('',#42492,10.);
#12516=VECTOR('',#42493,10.);
#12517=VECTOR('',#42496,10.);
#12518=VECTOR('',#42497,10.);
#12519=VECTOR('',#42504,10.);
#12520=VECTOR('',#42505,10.);
#12521=VECTOR('',#42506,10.);
#12522=VECTOR('',#42509,10.);
#12523=VECTOR('',#42510,10.);
#12524=VECTOR('',#42511,10.);
#12525=VECTOR('',#42514,10.);
#12526=VECTOR('',#42515,10.);
#12527=VECTOR('',#42516,10.);
#12528=VECTOR('',#42519,10.);
#12529=VECTOR('',#42520,10.);
#12530=VECTOR('',#42523,10.);
#12531=VECTOR('',#42524,10.);
#12532=VECTOR('',#42525,10.);
#12533=VECTOR('',#42528,10.);
#12534=VECTOR('',#42529,10.);
#12535=VECTOR('',#42532,10.);
#12536=VECTOR('',#42533,10.);
#12537=VECTOR('',#42536,10.);
#12538=VECTOR('',#42537,10.);
#12539=VECTOR('',#42540,10.);
#12540=VECTOR('',#42541,10.);
#12541=VECTOR('',#42544,10.);
#12542=VECTOR('',#42545,10.);
#12543=VECTOR('',#42548,10.);
#12544=VECTOR('',#42549,10.);
#12545=VECTOR('',#42552,10.);
#12546=VECTOR('',#42553,10.);
#12547=VECTOR('',#42562,10.);
#12548=VECTOR('',#42563,10.);
#12549=VECTOR('',#42564,10.);
#12550=VECTOR('',#42567,10.);
#12551=VECTOR('',#42568,10.);
#12552=VECTOR('',#42569,10.);
#12553=VECTOR('',#42572,10.);
#12554=VECTOR('',#42573,10.);
#12555=VECTOR('',#42574,10.);
#12556=VECTOR('',#42577,10.);
#12557=VECTOR('',#42578,10.);
#12558=VECTOR('',#42581,10.);
#12559=VECTOR('',#42582,10.);
#12560=VECTOR('',#42583,10.);
#12561=VECTOR('',#42586,10.);
#12562=VECTOR('',#42587,10.);
#12563=VECTOR('',#42590,10.);
#12564=VECTOR('',#42591,10.);
#12565=VECTOR('',#42594,10.);
#12566=VECTOR('',#42595,10.);
#12567=VECTOR('',#42598,10.);
#12568=VECTOR('',#42599,10.);
#12569=VECTOR('',#42602,10.);
#12570=VECTOR('',#42603,10.);
#12571=VECTOR('',#42606,10.);
#12572=VECTOR('',#42607,10.);
#12573=VECTOR('',#42610,10.);
#12574=VECTOR('',#42611,10.);
#12575=VECTOR('',#42620,10.);
#12576=VECTOR('',#42621,10.);
#12577=VECTOR('',#42622,10.);
#12578=VECTOR('',#42623,10.);
#12579=VECTOR('',#42626,10.);
#12580=VECTOR('',#42627,10.);
#12581=VECTOR('',#42630,10.);
#12582=VECTOR('',#42631,10.);
#12583=VECTOR('',#42632,10.);
#12584=VECTOR('',#42635,10.);
#12585=VECTOR('',#42636,10.);
#12586=VECTOR('',#42637,10.);
#12587=VECTOR('',#42640,10.);
#12588=VECTOR('',#42641,10.);
#12589=VECTOR('',#42644,10.);
#12590=VECTOR('',#42645,10.);
#12591=VECTOR('',#42648,10.);
#12592=VECTOR('',#42649,10.);
#12593=VECTOR('',#42652,10.);
#12594=VECTOR('',#42653,10.);
#12595=VECTOR('',#42654,10.);
#12596=VECTOR('',#42657,10.);
#12597=VECTOR('',#42658,10.);
#12598=VECTOR('',#42661,10.);
#12599=VECTOR('',#42662,10.);
#12600=VECTOR('',#42665,10.);
#12601=VECTOR('',#42666,10.);
#12602=VECTOR('',#42669,10.);
#12603=VECTOR('',#42676,10.);
#12604=VECTOR('',#42677,10.);
#12605=VECTOR('',#42678,10.);
#12606=VECTOR('',#42681,10.);
#12607=VECTOR('',#42682,10.);
#12608=VECTOR('',#42683,10.);
#12609=VECTOR('',#42686,10.);
#12610=VECTOR('',#42687,10.);
#12611=VECTOR('',#42688,10.);
#12612=VECTOR('',#42691,10.);
#12613=VECTOR('',#42692,10.);
#12614=VECTOR('',#42695,10.);
#12615=VECTOR('',#42696,10.);
#12616=VECTOR('',#42697,10.);
#12617=VECTOR('',#42700,10.);
#12618=VECTOR('',#42701,10.);
#12619=VECTOR('',#42704,10.);
#12620=VECTOR('',#42705,10.);
#12621=VECTOR('',#42708,10.);
#12622=VECTOR('',#42709,10.);
#12623=VECTOR('',#42712,10.);
#12624=VECTOR('',#42713,10.);
#12625=VECTOR('',#42716,10.);
#12626=VECTOR('',#42717,10.);
#12627=VECTOR('',#42720,10.);
#12628=VECTOR('',#42721,10.);
#12629=VECTOR('',#42724,10.);
#12630=VECTOR('',#42725,10.);
#12631=VECTOR('',#42734,10.);
#12632=VECTOR('',#42735,10.);
#12633=VECTOR('',#42736,10.);
#12634=VECTOR('',#42739,10.);
#12635=VECTOR('',#42740,10.);
#12636=VECTOR('',#42741,10.);
#12637=VECTOR('',#42742,10.);
#12638=VECTOR('',#42745,10.);
#12639=VECTOR('',#42746,10.);
#12640=VECTOR('',#42749,10.);
#12641=VECTOR('',#42750,10.);
#12642=VECTOR('',#42751,10.);
#12643=VECTOR('',#42754,10.);
#12644=VECTOR('',#42755,10.);
#12645=VECTOR('',#42756,10.);
#12646=VECTOR('',#42757,10.);
#12647=VECTOR('',#42760,10.);
#12648=VECTOR('',#42761,10.);
#12649=VECTOR('',#42764,10.);
#12650=VECTOR('',#42765,10.);
#12651=VECTOR('',#42768,10.);
#12652=VECTOR('',#42769,10.);
#12653=VECTOR('',#42770,10.);
#12654=VECTOR('',#42773,10.);
#12655=VECTOR('',#42776,10.);
#12656=VECTOR('',#42777,10.);
#12657=VECTOR('',#42780,10.);
#12658=VECTOR('',#42781,10.);
#12659=VECTOR('',#42788,10.);
#12660=VECTOR('',#42789,10.);
#12661=VECTOR('',#42790,10.);
#12662=VECTOR('',#42793,10.);
#12663=VECTOR('',#42794,10.);
#12664=VECTOR('',#42795,10.);
#12665=VECTOR('',#42798,10.);
#12666=VECTOR('',#42799,10.);
#12667=VECTOR('',#42800,10.);
#12668=VECTOR('',#42803,10.);
#12669=VECTOR('',#42804,10.);
#12670=VECTOR('',#42807,10.);
#12671=VECTOR('',#42808,10.);
#12672=VECTOR('',#42809,10.);
#12673=VECTOR('',#42812,10.);
#12674=VECTOR('',#42813,10.);
#12675=VECTOR('',#42816,10.);
#12676=VECTOR('',#42817,10.);
#12677=VECTOR('',#42820,10.);
#12678=VECTOR('',#42821,10.);
#12679=VECTOR('',#42824,10.);
#12680=VECTOR('',#42825,10.);
#12681=VECTOR('',#42828,10.);
#12682=VECTOR('',#42829,10.);
#12683=VECTOR('',#42832,10.);
#12684=VECTOR('',#42833,10.);
#12685=VECTOR('',#42836,10.);
#12686=VECTOR('',#42837,10.);
#12687=VECTOR('',#42846,10.);
#12688=VECTOR('',#42847,10.);
#12689=VECTOR('',#42848,10.);
#12690=VECTOR('',#42851,10.);
#12691=VECTOR('',#42852,10.);
#12692=VECTOR('',#42853,10.);
#12693=VECTOR('',#42856,10.);
#12694=VECTOR('',#42857,10.);
#12695=VECTOR('',#42858,10.);
#12696=VECTOR('',#42861,10.);
#12697=VECTOR('',#42862,10.);
#12698=VECTOR('',#42865,10.);
#12699=VECTOR('',#42866,10.);
#12700=VECTOR('',#42867,10.);
#12701=VECTOR('',#42870,10.);
#12702=VECTOR('',#42871,10.);
#12703=VECTOR('',#42874,10.);
#12704=VECTOR('',#42875,10.);
#12705=VECTOR('',#42878,10.);
#12706=VECTOR('',#42879,10.);
#12707=VECTOR('',#42882,10.);
#12708=VECTOR('',#42883,10.);
#12709=VECTOR('',#42886,10.);
#12710=VECTOR('',#42887,10.);
#12711=VECTOR('',#42890,10.);
#12712=VECTOR('',#42891,10.);
#12713=VECTOR('',#42894,10.);
#12714=VECTOR('',#42895,10.);
#12715=VECTOR('',#42908,127.185823536562);
#12716=VECTOR('',#42915,128.);
#12717=VECTOR('',#42924,127.);
#12718=VECTOR('',#42927,10.);
#12719=VECTOR('',#42928,10.);
#12720=VECTOR('',#42929,10.);
#12721=VECTOR('',#42932,10.);
#12722=VECTOR('',#42933,10.);
#12723=VECTOR('',#42934,10.);
#12724=VECTOR('',#42937,10.);
#12725=VECTOR('',#42938,10.);
#12726=VECTOR('',#42939,10.);
#12727=VECTOR('',#42942,10.);
#12728=VECTOR('',#42943,10.);
#12729=VECTOR('',#42946,10.);
#12730=VECTOR('',#42947,10.);
#12731=VECTOR('',#42948,10.);
#12732=VECTOR('',#42951,10.);
#12733=VECTOR('',#42952,10.);
#12734=VECTOR('',#42955,10.);
#12735=VECTOR('',#42956,10.);
#12736=VECTOR('',#42959,10.);
#12737=VECTOR('',#42960,10.);
#12738=VECTOR('',#42963,10.);
#12739=VECTOR('',#42964,10.);
#12740=VECTOR('',#42967,10.);
#12741=VECTOR('',#42968,10.);
#12742=VECTOR('',#42971,10.);
#12743=VECTOR('',#42972,10.);
#12744=VECTOR('',#42975,10.);
#12745=VECTOR('',#42976,10.);
#12746=VECTOR('',#42985,10.);
#12747=VECTOR('',#42986,10.);
#12748=VECTOR('',#42987,10.);
#12749=VECTOR('',#42990,10.);
#12750=VECTOR('',#42991,10.);
#12751=VECTOR('',#42992,10.);
#12752=VECTOR('',#42995,10.);
#12753=VECTOR('',#42996,10.);
#12754=VECTOR('',#42997,10.);
#12755=VECTOR('',#43000,10.);
#12756=VECTOR('',#43001,10.);
#12757=VECTOR('',#43004,10.);
#12758=VECTOR('',#43005,10.);
#12759=VECTOR('',#43006,10.);
#12760=VECTOR('',#43009,10.);
#12761=VECTOR('',#43010,10.);
#12762=VECTOR('',#43013,10.);
#12763=VECTOR('',#43014,10.);
#12764=VECTOR('',#43017,10.);
#12765=VECTOR('',#43018,10.);
#12766=VECTOR('',#43021,10.);
#12767=VECTOR('',#43022,10.);
#12768=VECTOR('',#43025,10.);
#12769=VECTOR('',#43026,10.);
#12770=VECTOR('',#43029,10.);
#12771=VECTOR('',#43030,10.);
#12772=VECTOR('',#43033,10.);
#12773=VECTOR('',#43034,10.);
#12774=VECTOR('',#43047,138.753401519042);
#12775=VECTOR('',#43054,139.);
#12776=VECTOR('',#43061,137.5);
#12777=VECTOR('',#43066,129.064176463438);
#12778=VECTOR('',#43075,138.823223304703);
#12779=VECTOR('',#43078,138.5);
#12780=VECTOR('',#43083,137.926776695297);
#12781=VECTOR('',#43374,7.18);
#12782=VECTOR('',#43379,7.18);
#12783=VECTOR('',#43384,7.18);
#12784=VECTOR('',#43389,7.18);
#12785=VECTOR('',#43394,7.18);
#12786=VECTOR('',#43401,25.);
#12787=VECTOR('',#43406,23.);
#12788=VECTOR('',#43411,10.);
#12789=VECTOR('',#43416,10.);
#12790=VECTOR('',#43421,10.);
#12791=VECTOR('',#43432,25.16);
#12792=VECTOR('',#43439,27.);
#12793=VECTOR('',#43446,29.58);
#12794=VECTOR('',#43455,32.6);
#12795=VECTOR('',#43460,32.9);
#12796=VECTOR('',#43465,43.);
#12797=VECTOR('',#43472,124.75);
#12798=VECTOR('',#43477,126.75);
#12799=VECTOR('',#43482,11.59764);
#12800=VECTOR('',#43485,11.59764);
#12801=VECTOR('',#43488,11.59764);
#12802=VECTOR('',#43491,11.59764);
#12803=VECTOR('',#43494,11.59764);
#12804=VECTOR('',#43497,11.59764);
#12805=VECTOR('',#43500,11.59764);
#12806=VECTOR('',#43505,11.59764);
#12807=VECTOR('',#43508,11.59764);
#12808=VECTOR('',#43513,3.02920176969664);
#12809=VECTOR('',#43518,1.5);
#12810=VECTOR('',#43525,10.);
#12811=VECTOR('',#43526,10.);
#12812=VECTOR('',#43527,10.);
#12813=VECTOR('',#43528,10.);
#12814=VECTOR('',#43531,10.);
#12815=VECTOR('',#43532,10.);
#12816=VECTOR('',#43533,10.);
#12817=VECTOR('',#43536,10.);
#12818=VECTOR('',#43537,10.);
#12819=VECTOR('',#43538,10.);
#12820=VECTOR('',#43539,10.);
#12821=VECTOR('',#43540,10.);
#12822=VECTOR('',#43541,10.);
#12823=VECTOR('',#43544,10.);
#12824=VECTOR('',#43545,10.);
#12825=VECTOR('',#43546,10.);
#12826=VECTOR('',#43549,10.);
#12827=VECTOR('',#43550,10.);
#12828=VECTOR('',#43551,10.);
#12829=VECTOR('',#43554,10.);
#12830=VECTOR('',#43555,10.);
#12831=VECTOR('',#43556,10.);
#12832=VECTOR('',#43557,10.);
#12833=VECTOR('',#43560,10.);
#12834=VECTOR('',#43561,10.);
#12835=VECTOR('',#43562,10.);
#12836=VECTOR('',#43565,10.);
#12837=VECTOR('',#43566,10.);
#12838=VECTOR('',#43567,10.);
#12839=VECTOR('',#43570,10.);
#12840=VECTOR('',#43571,10.);
#12841=VECTOR('',#43572,10.);
#12842=VECTOR('',#43575,10.);
#12843=VECTOR('',#43576,10.);
#12844=VECTOR('',#43577,10.);
#12845=VECTOR('',#43580,10.);
#12846=VECTOR('',#43581,10.);
#12847=VECTOR('',#43582,10.);
#12848=VECTOR('',#43583,10.);
#12849=VECTOR('',#43586,10.);
#12850=VECTOR('',#43587,10.);
#12851=VECTOR('',#43590,10.);
#12852=VECTOR('',#43591,10.);
#12853=VECTOR('',#43592,10.);
#12854=VECTOR('',#43595,10.);
#12855=VECTOR('',#43596,10.);
#12856=VECTOR('',#43597,10.);
#12857=VECTOR('',#43598,10.);
#12858=VECTOR('',#43601,10.);
#12859=VECTOR('',#43602,10.);
#12860=VECTOR('',#43605,10.);
#12861=VECTOR('',#43606,10.);
#12862=VECTOR('',#43607,10.);
#12863=VECTOR('',#43610,10.);
#12864=VECTOR('',#43611,10.);
#12865=VECTOR('',#43612,10.);
#12866=VECTOR('',#43613,10.);
#12867=VECTOR('',#43616,10.);
#12868=VECTOR('',#43617,10.);
#12869=VECTOR('',#43620,10.);
#12870=VECTOR('',#43621,10.);
#12871=VECTOR('',#43622,10.);
#12872=VECTOR('',#43625,10.);
#12873=VECTOR('',#43626,10.);
#12874=VECTOR('',#43627,10.);
#12875=VECTOR('',#43628,10.);
#12876=VECTOR('',#43631,10.);
#12877=VECTOR('',#43632,10.);
#12878=VECTOR('',#43635,10.);
#12879=VECTOR('',#43636,10.);
#12880=VECTOR('',#43637,10.);
#12881=VECTOR('',#43640,10.);
#12882=VECTOR('',#43641,10.);
#12883=VECTOR('',#43642,10.);
#12884=VECTOR('',#43643,10.);
#12885=VECTOR('',#43646,10.);
#12886=VECTOR('',#43647,10.);
#12887=VECTOR('',#43650,10.);
#12888=VECTOR('',#43651,10.);
#12889=VECTOR('',#43652,10.);
#12890=VECTOR('',#43653,10.);
#12891=VECTOR('',#43656,10.);
#12892=VECTOR('',#43657,10.);
#12893=VECTOR('',#43658,10.);
#12894=VECTOR('',#43659,10.);
#12895=VECTOR('',#43662,10.);
#12896=VECTOR('',#43665,10.);
#12897=VECTOR('',#43666,10.);
#12898=VECTOR('',#43669,10.);
#12899=VECTOR('',#43672,10.);
#12900=VECTOR('',#43673,10.);
#12901=VECTOR('',#43676,10.);
#12902=VECTOR('',#43679,10.);
#12903=VECTOR('',#43680,10.);
#12904=VECTOR('',#43683,10.);
#12905=VECTOR('',#43684,10.);
#12906=VECTOR('',#43685,10.);
#12907=VECTOR('',#43688,10.);
#12908=VECTOR('',#43691,10.);
#12909=VECTOR('',#43692,10.);
#12910=VECTOR('',#43697,7.);
#12911=VECTOR('',#43702,10.);
#12912=VECTOR('',#43715,6.75);
#12913=VECTOR('',#43718,7.);
#12914=VECTOR('',#43725,6.75);
#12915=VECTOR('',#43728,7.);
#12916=VECTOR('',#43735,6.75);
#12917=VECTOR('',#43738,7.);
#12918=VECTOR('',#43745,6.75);
#12919=VECTOR('',#43750,7.);
#12920=VECTOR('',#43753,10.);
#12921=VECTOR('',#43764,7.);
#12922=VECTOR('',#43767,7.);
#12923=VECTOR('',#43770,7.);
#12924=VECTOR('',#43773,10.);
#12925=VECTOR('',#43790,25.2232233047034);
#12926=VECTOR('',#43797,25.);
#12927=VECTOR('',#43804,25.4);
#12928=VECTOR('',#43807,24.5267766952966);
#12929=VECTOR('',#43832,10.);
#12930=VECTOR('',#43843,10.);
#12931=VECTOR('',#43846,10.);
#12932=VECTOR('',#43847,10.);
#12933=VECTOR('',#43850,10.);
#12934=VECTOR('',#43851,10.);
#12935=VECTOR('',#43854,10.);
#12936=VECTOR('',#43855,10.);
#12937=VECTOR('',#43858,10.);
#12938=VECTOR('',#43859,10.);
#12939=VECTOR('',#43862,10.);
#12940=VECTOR('',#43863,10.);
#12941=VECTOR('',#43866,10.);
#12942=VECTOR('',#43867,10.);
#12943=VECTOR('',#43870,10.);
#12944=VECTOR('',#43871,10.);
#12945=VECTOR('',#43874,10.);
#12946=VECTOR('',#43875,10.);
#12947=VECTOR('',#43878,10.);
#12948=VECTOR('',#43879,10.);
#12949=VECTOR('',#43884,10.);
#12950=VECTOR('',#43885,10.);
#12951=VECTOR('',#43922,2.20000000000001);
#12952=VECTOR('',#43927,23.61565);
#12953=VECTOR('',#43932,21.8313);
#12954=VECTOR('',#43941,17.72);
#12955=VECTOR('',#43946,17.47);
#12956=VECTOR('',#43951,15.72);
#12957=VECTOR('',#43956,13.72);
#12958=VECTOR('',#43961,10.);
#12959=VECTOR('',#43962,10.);
#12960=VECTOR('',#43965,10.);
#12961=VECTOR('',#43966,10.);
#12962=VECTOR('',#43969,10.);
#12963=VECTOR('',#43972,13.47);
#12964=VECTOR('',#43977,10.);
#12965=VECTOR('',#43986,11.9);
#12966=VECTOR('',#43989,12.3);
#12967=VECTOR('',#43992,12.35);
#12968=VECTOR('',#44005,24.69);
#12969=VECTOR('',#44014,24.5);
#12970=VECTOR('',#44021,29.59);
#12971=VECTOR('',#44034,29.4);
#12972=VECTOR('',#44051,32.385);
#12973=VECTOR('',#44056,32.585);
#12974=VECTOR('',#44059,32.385);
#12975=VECTOR('',#44062,23.95);
#12976=VECTOR('',#44067,22.62065);
#12977=VECTOR('',#44072,21.8413);
#12978=VECTOR('',#44077,22.77065);
#12979=VECTOR('',#44086,29.1655);
#12980=VECTOR('',#44093,29.5655);
#12981=VECTOR('',#44098,29.2655);
#12982=VECTOR('',#44105,28.3587781164969);
#12983=VECTOR('',#44110,27.3267351683296);
#12984=VECTOR('',#44115,26.6550961100811);
#12985=VECTOR('',#44128,25.6346416389917);
#12986=VECTOR('',#44139,25.8846416389917);
#12987=VECTOR('',#44144,22.5243990607509);
#12988=VECTOR('',#44151,22.7743990607509);
#12989=VECTOR('',#44732,22.5743990607509);
#12990=VECTOR('',#44737,22.011553150687);
#12991=VECTOR('',#44738,22.011553150687);
#12992=VECTOR('',#44743,25.6346416389917);
#12993=VECTOR('',#44750,17.894);
#12994=VECTOR('',#44755,17.494);
#12995=VECTOR('',#44760,17.794);
#12996=VECTOR('',#44771,24.746);
#12997=VECTOR('',#44778,25.146);
#12998=VECTOR('',#44783,24.846);
#12999=VECTOR('',#44790,23.9381298772848);
#13000=VECTOR('',#44795,23.0066610487235);
#13001=VECTOR('',#44800,22.4355961100811);
#13002=VECTOR('',#44813,21.4356897166516);
#13003=VECTOR('',#44824,21.6856897166516);
#13004=VECTOR('',#44829,18.568471118769);
#13005=VECTOR('',#44836,18.818471118769);
#13006=VECTOR('',#45365,18.618471118769);
#13007=VECTOR('',#45370,18.0894454950083);
#13008=VECTOR('',#45371,18.0894454950083);
#13009=VECTOR('',#45376,21.4356897166516);
#13010=VECTOR('',#45383,13.894);
#13011=VECTOR('',#45388,13.494);
#13012=VECTOR('',#45393,13.794);
#13013=VECTOR('',#45402,10.);
#13014=VECTOR('',#45403,10.);
#13015=VECTOR('',#45404,10.);
#13016=VECTOR('',#45405,10.);
#13017=VECTOR('',#45408,10.);
#13018=VECTOR('',#45409,10.);
#13019=VECTOR('',#45410,10.);
#13020=VECTOR('',#45411,10.);
#13021=VECTOR('',#45412,10.);
#13022=VECTOR('',#45415,10.);
#13023=VECTOR('',#45416,10.);
#13024=VECTOR('',#45419,10.);
#13025=VECTOR('',#45420,10.);
#13026=VECTOR('',#45423,10.);
#13027=VECTOR('',#45424,10.);
#13028=VECTOR('',#45425,10.);
#13029=VECTOR('',#45444,20.35);
#13030=VECTOR('',#45449,20.5);
#13031=VECTOR('',#45452,20.35);
#13032=VECTOR('',#45457,10.);
#13033=VECTOR('',#45458,10.);
#13034=VECTOR('',#45459,10.);
#13035=VECTOR('',#45464,10.);
#13036=VECTOR('',#45471,10.);
#13037=VECTOR('',#45472,10.);
#13038=VECTOR('',#45473,10.);
#13039=VECTOR('',#45474,10.);
#13040=VECTOR('',#45477,10.);
#13041=VECTOR('',#45478,10.);
#13042=VECTOR('',#45481,10.);
#13043=VECTOR('',#45482,10.);
#13044=VECTOR('',#45483,10.);
#13045=VECTOR('',#45486,10.);
#13046=VECTOR('',#45487,10.);
#13047=VECTOR('',#45488,10.);
#13048=VECTOR('',#45489,10.);
#13049=VECTOR('',#45490,10.);
#13050=VECTOR('',#45493,10.);
#13051=VECTOR('',#45494,10.);
#13052=VECTOR('',#45495,10.);
#13053=VECTOR('',#45498,10.);
#13054=VECTOR('',#45499,10.);
#13055=VECTOR('',#45504,10.);
#13056=VECTOR('',#45505,10.);
#13057=VECTOR('',#45506,10.);
#13058=VECTOR('',#45507,10.);
#13059=VECTOR('',#45510,10.);
#13060=VECTOR('',#45517,10.);
#13061=VECTOR('',#45518,10.);
#13062=VECTOR('',#45519,10.);
#13063=VECTOR('',#45520,10.);
#13064=VECTOR('',#45523,10.);
#13065=VECTOR('',#45524,10.);
#13066=VECTOR('',#45525,10.);
#13067=VECTOR('',#45526,10.);
#13068=VECTOR('',#45527,10.);
#13069=VECTOR('',#45530,10.);
#13070=VECTOR('',#45531,10.);
#13071=VECTOR('',#45532,10.);
#13072=VECTOR('',#45533,10.);
#13073=VECTOR('',#45536,10.);
#13074=VECTOR('',#45537,10.);
#13075=VECTOR('',#45540,10.);
#13076=VECTOR('',#45541,10.);
#13077=VECTOR('',#45542,10.);
#13078=VECTOR('',#45553,10.);
#13079=VECTOR('',#45558,10.);
#13080=VECTOR('',#45559,10.);
#13081=VECTOR('',#45562,10.);
#13082=VECTOR('',#45563,10.);
#13083=VECTOR('',#45566,10.);
#13084=VECTOR('',#45567,10.);
#13085=VECTOR('',#45568,10.);
#13086=VECTOR('',#45573,19.8);
#13087=VECTOR('',#45576,10.);
#13088=VECTOR('',#45577,10.);
#13089=VECTOR('',#45578,10.);
#13090=VECTOR('',#45583,10.);
#13091=VECTOR('',#45590,10.);
#13092=VECTOR('',#45591,10.);
#13093=VECTOR('',#45592,10.);
#13094=VECTOR('',#45593,10.);
#13095=VECTOR('',#45596,10.);
#13096=VECTOR('',#45597,10.);
#13097=VECTOR('',#45600,10.);
#13098=VECTOR('',#45601,10.);
#13099=VECTOR('',#45602,10.);
#13100=VECTOR('',#45605,10.);
#13101=VECTOR('',#45606,10.);
#13102=VECTOR('',#45609,10.);
#13103=VECTOR('',#45610,10.);
#13104=VECTOR('',#45613,10.);
#13105=VECTOR('',#45614,10.);
#13106=VECTOR('',#45617,10.);
#13107=VECTOR('',#45620,10.);
#13108=VECTOR('',#45621,10.);
#13109=VECTOR('',#45622,10.);
#13110=VECTOR('',#45625,10.);
#13111=VECTOR('',#45626,10.);
#13112=VECTOR('',#45629,10.);
#13113=VECTOR('',#45630,10.);
#13114=VECTOR('',#45633,10.);
#13115=VECTOR('',#45634,10.);
#13116=VECTOR('',#45635,10.);
#13117=VECTOR('',#45636,10.);
#13118=VECTOR('',#45639,10.);
#13119=VECTOR('',#45640,10.);
#13120=VECTOR('',#45641,10.);
#13121=VECTOR('',#45644,10.);
#13122=VECTOR('',#45645,10.);
#13123=VECTOR('',#45650,10.);
#13124=VECTOR('',#45651,10.);
#13125=VECTOR('',#45652,10.);
#13126=VECTOR('',#45653,10.);
#13127=VECTOR('',#45656,10.);
#13128=VECTOR('',#45663,10.);
#13129=VECTOR('',#45664,10.);
#13130=VECTOR('',#45665,10.);
#13131=VECTOR('',#45666,10.);
#13132=VECTOR('',#45667,10.);
#13133=VECTOR('',#45670,10.);
#13134=VECTOR('',#45671,10.);
#13135=VECTOR('',#45674,10.);
#13136=VECTOR('',#45681,10.);
#13137=VECTOR('',#45682,10.);
#13138=VECTOR('',#45683,10.);
#13139=VECTOR('',#45690,10.);
#13140=VECTOR('',#45691,10.);
#13141=VECTOR('',#45692,10.);
#13142=VECTOR('',#45693,10.);
#13143=VECTOR('',#45694,10.);
#13144=VECTOR('',#45697,10.);
#13145=VECTOR('',#45698,10.);
#13146=VECTOR('',#45699,10.);
#13147=VECTOR('',#45702,10.);
#13148=VECTOR('',#45705,10.);
#13149=VECTOR('',#45706,10.);
#13150=VECTOR('',#45707,10.);
#13151=VECTOR('',#45710,10.);
#13152=VECTOR('',#45713,10.);
#13153=VECTOR('',#45714,10.);
#13154=VECTOR('',#45715,10.);
#13155=VECTOR('',#45718,10.);
#13156=VECTOR('',#45719,10.);
#13157=VECTOR('',#45728,10.);
#13158=VECTOR('',#45731,10.);
#13159=VECTOR('',#45732,10.);
#13160=VECTOR('',#45737,10.);
#13161=VECTOR('',#45740,10.);
#13162=VECTOR('',#45743,10.);
#13163=VECTOR('',#45746,10.);
#13164=VECTOR('',#45747,10.);
#13165=VECTOR('',#45750,10.);
#13166=VECTOR('',#45753,10.);
#13167=VECTOR('',#45756,10.);
#13168=VECTOR('',#45757,10.);
#13169=VECTOR('',#45758,10.);
#13170=VECTOR('',#45771,10.);
#13171=VECTOR('',#45772,10.);
#13172=VECTOR('',#45783,10.);
#13173=VECTOR('',#45788,10.);
#13174=VECTOR('',#45791,10.);
#13175=VECTOR('',#45794,10.);
#13176=VECTOR('',#45797,12.75);
#13177=VECTOR('',#45810,10.);
#13178=VECTOR('',#45811,10.);
#13179=VECTOR('',#45814,10.);
#13180=VECTOR('',#45815,10.);
#13181=VECTOR('',#45818,10.);
#13182=VECTOR('',#45825,10.);
#13183=VECTOR('',#45826,10.);
#13184=VECTOR('',#45827,10.);
#13185=VECTOR('',#45830,10.);
#13186=VECTOR('',#45831,10.);
#13187=VECTOR('',#45834,10.);
#13188=VECTOR('',#45835,10.);
#13189=VECTOR('',#45838,10.);
#13190=VECTOR('',#45841,10.);
#13191=VECTOR('',#45842,10.);
#13192=VECTOR('',#45845,10.);
#13193=VECTOR('',#45846,10.);
#13194=VECTOR('',#45849,10.);
#13195=VECTOR('',#45856,10.);
#13196=VECTOR('',#45857,10.);
#13197=VECTOR('',#45864,10.);
#13198=VECTOR('',#45877,10.);
#13199=VECTOR('',#45878,10.);
#13200=VECTOR('',#45881,10.);
#13201=VECTOR('',#45882,10.);
#13202=VECTOR('',#45883,10.);
#13203=VECTOR('',#45886,10.);
#13204=VECTOR('',#45887,10.);
#13205=VECTOR('',#45890,10.);
#13206=VECTOR('',#45891,10.);
#13207=VECTOR('',#45894,10.);
#13208=VECTOR('',#45895,10.);
#13209=VECTOR('',#45906,13.075);
#13210=VECTOR('',#45909,10.);
#13211=VECTOR('',#45912,10.);
#13212=VECTOR('',#45921,10.);
#13213=VECTOR('',#45942,1.95);
#13214=VECTOR('',#45945,10.);
#13215=VECTOR('',#45948,10.);
#13216=VECTOR('',#45951,10.);
#13217=VECTOR('',#45954,10.);
#13218=VECTOR('',#45959,10.);
#13219=VECTOR('',#45960,10.);
#13220=VECTOR('',#45961,10.);
#13221=VECTOR('',#45968,10.);
#13222=VECTOR('',#45969,10.);
#13223=VECTOR('',#45970,10.);
#13224=VECTOR('',#45973,10.);
#13225=VECTOR('',#45974,10.);
#13226=VECTOR('',#45977,10.);
#13227=VECTOR('',#45978,10.);
#13228=VECTOR('',#45979,10.);
#13229=VECTOR('',#45982,10.);
#13230=VECTOR('',#45983,10.);
#13231=VECTOR('',#45984,10.);
#13232=VECTOR('',#45987,10.);
#13233=VECTOR('',#45988,10.);
#13234=VECTOR('',#45991,10.);
#13235=VECTOR('',#45994,10.);
#13236=VECTOR('',#46021,20.9831675294297);
#13237=VECTOR('',#46028,22.1);
#13238=VECTOR('',#46037,19.75);
#13239=VECTOR('',#46040,23.1453899562452);
#13240=VECTOR('',#46047,24.);
#13241=VECTOR('',#46054,24.7086590704751);
#13242=VECTOR('',#46061,25.2);
#13243=VECTOR('',#46068,25.5145642342283);
#13244=VECTOR('',#46075,25.6);
#13245=VECTOR('',#46088,24.82);
#13246=VECTOR('',#46093,25.12);
#13247=VECTOR('',#46102,26.8);
#13248=VECTOR('',#46105,26.2);
#13249=VECTOR('',#46114,19.55);
#13250=VECTOR('',#46119,21.65);
#13251=VECTOR('',#46124,23.3);
#13252=VECTOR('',#46129,24.4);
#13253=VECTOR('',#46134,24.56);
#13254=VECTOR('',#46139,24.32);
#13255=VECTOR('',#46144,6.35);
#13256=VECTOR('',#46149,6.35);
#13257=VECTOR('',#46152,6.35);
#13258=VECTOR('',#46155,6.35);
#13259=VECTOR('',#46158,6.35);
#13260=VECTOR('',#46161,6.35);
#13261=VECTOR('',#46164,6.35);
#13262=VECTOR('',#46167,6.35);
#13263=VECTOR('',#46170,6.35);
#13264=VECTOR('',#46173,6.35);
#13265=VECTOR('',#46176,6.35);
#13266=VECTOR('',#46179,6.35);
#13267=VECTOR('',#46182,6.35);
#13268=VECTOR('',#46185,6.35);
#13269=VECTOR('',#46188,6.35);
#13270=VECTOR('',#46191,6.35);
#13271=VECTOR('',#46194,6.35);
#13272=VECTOR('',#46197,6.35);
#13273=VECTOR('',#46200,6.35);
#13274=VECTOR('',#46203,6.35);
#13275=VECTOR('',#46206,6.35);
#13276=VECTOR('',#46209,6.35);
#13277=VECTOR('',#46212,6.35);
#13278=VECTOR('',#46215,6.35);
#13279=VECTOR('',#46218,6.35);
#13280=VECTOR('',#46221,6.35);
#13281=VECTOR('',#46224,6.35);
#13282=VECTOR('',#46227,6.35);
#13283=VECTOR('',#46230,6.35);
#13284=VECTOR('',#46233,5.57784);
#13285=VECTOR('',#46238,5.57784);
#13286=VECTOR('',#46243,5.57784);
#13287=VECTOR('',#46246,5.57784);
#13288=VECTOR('',#46249,5.57784);
#13289=VECTOR('',#46252,5.57784);
#13290=VECTOR('',#46255,5.57784);
#13291=VECTOR('',#46258,5.57784);
#13292=VECTOR('',#46261,5.57784);
#13293=VECTOR('',#46264,5.57784);
#13294=VECTOR('',#46267,5.57784);
#13295=VECTOR('',#46270,5.57784);
#13296=VECTOR('',#46273,5.57784);
#13297=VECTOR('',#46276,5.57784);
#13298=VECTOR('',#46279,5.57784);
#13299=VECTOR('',#46282,5.57784);
#13300=VECTOR('',#46285,5.57784);
#13301=VECTOR('',#46288,5.57784);
#13302=VECTOR('',#46291,5.57784);
#13303=VECTOR('',#46294,5.57784);
#13304=VECTOR('',#46297,5.57784);
#13305=VECTOR('',#46300,5.57784);
#13306=VECTOR('',#46303,5.57784);
#13307=VECTOR('',#46306,5.57784);
#13308=VECTOR('',#46309,5.57784);
#13309=VECTOR('',#46312,5.57784);
#13310=VECTOR('',#46315,5.57784);
#13311=VECTOR('',#46318,5.57784);
#13312=VECTOR('',#46321,5.57784);
#13313=VECTOR('',#46326,5.47677669529664);
#13314=VECTOR('',#46333,5.95);
#13315=VECTOR('',#46344,10.);
#13316=VECTOR('',#46345,10.);
#13317=VECTOR('',#46346,10.);
#13318=VECTOR('',#46347,10.);
#13319=VECTOR('',#46356,10.);
#13320=VECTOR('',#46357,10.);
#13321=VECTOR('',#46358,10.);
#13322=VECTOR('',#46363,10.);
#13323=VECTOR('',#46372,10.);
#13324=VECTOR('',#46373,10.);
#13325=VECTOR('',#46374,10.);
#13326=VECTOR('',#46377,10.);
#13327=VECTOR('',#46400,10.);
#13328=VECTOR('',#46401,10.);
#13329=VECTOR('',#46402,10.);
#13330=VECTOR('',#46403,10.);
#13331=VECTOR('',#46408,10.);
#13332=VECTOR('',#46411,10.);
#13333=VECTOR('',#46412,10.);
#13334=VECTOR('',#46419,10.);
#13335=VECTOR('',#46420,10.);
#13336=VECTOR('',#46421,10.);
#13337=VECTOR('',#46422,10.);
#13338=VECTOR('',#46427,10.);
#13339=VECTOR('',#46430,10.);
#13340=VECTOR('',#46431,10.);
#13341=VECTOR('',#46438,10.);
#13342=VECTOR('',#46439,10.);
#13343=VECTOR('',#46440,10.);
#13344=VECTOR('',#46441,10.);
#13345=VECTOR('',#46446,10.);
#13346=VECTOR('',#46449,10.);
#13347=VECTOR('',#46450,10.);
#13348=VECTOR('',#46457,10.);
#13349=VECTOR('',#46458,10.);
#13350=VECTOR('',#46459,10.);
#13351=VECTOR('',#46460,10.);
#13352=VECTOR('',#46465,10.);
#13353=VECTOR('',#46468,10.);
#13354=VECTOR('',#46469,10.);
#13355=VECTOR('',#46476,10.);
#13356=VECTOR('',#46477,10.);
#13357=VECTOR('',#46478,10.);
#13358=VECTOR('',#46479,10.);
#13359=VECTOR('',#46484,10.);
#13360=VECTOR('',#46487,10.);
#13361=VECTOR('',#46488,10.);
#13362=VECTOR('',#46495,10.);
#13363=VECTOR('',#46496,10.);
#13364=VECTOR('',#46497,10.);
#13365=VECTOR('',#46498,10.);
#13366=VECTOR('',#46503,10.);
#13367=VECTOR('',#46506,10.);
#13368=VECTOR('',#46507,10.);
#13369=VECTOR('',#46514,10.);
#13370=VECTOR('',#46515,10.);
#13371=VECTOR('',#46516,10.);
#13372=VECTOR('',#46517,10.);
#13373=VECTOR('',#46522,10.);
#13374=VECTOR('',#46525,10.);
#13375=VECTOR('',#46526,10.);
#13376=VECTOR('',#46533,10.);
#13377=VECTOR('',#46534,10.);
#13378=VECTOR('',#46535,10.);
#13379=VECTOR('',#46536,10.);
#13380=VECTOR('',#46541,10.);
#13381=VECTOR('',#46544,10.);
#13382=VECTOR('',#46545,10.);
#13383=VECTOR('',#46552,10.);
#13384=VECTOR('',#46553,10.);
#13385=VECTOR('',#46554,10.);
#13386=VECTOR('',#46555,10.);
#13387=VECTOR('',#46560,10.);
#13388=VECTOR('',#46563,10.);
#13389=VECTOR('',#46564,10.);
#13390=VECTOR('',#46571,10.);
#13391=VECTOR('',#46572,10.);
#13392=VECTOR('',#46573,10.);
#13393=VECTOR('',#46574,10.);
#13394=VECTOR('',#46579,10.);
#13395=VECTOR('',#46582,10.);
#13396=VECTOR('',#46583,10.);
#13397=VECTOR('',#46590,10.);
#13398=VECTOR('',#46591,10.);
#13399=VECTOR('',#46592,10.);
#13400=VECTOR('',#46593,10.);
#13401=VECTOR('',#46598,10.);
#13402=VECTOR('',#46601,10.);
#13403=VECTOR('',#46602,10.);
#13404=VECTOR('',#46609,10.);
#13405=VECTOR('',#46610,10.);
#13406=VECTOR('',#46611,10.);
#13407=VECTOR('',#46612,10.);
#13408=VECTOR('',#46617,10.);
#13409=VECTOR('',#46620,10.);
#13410=VECTOR('',#46621,10.);
#13411=VECTOR('',#46628,10.);
#13412=VECTOR('',#46629,10.);
#13413=VECTOR('',#46630,10.);
#13414=VECTOR('',#46631,10.);
#13415=VECTOR('',#46636,10.);
#13416=VECTOR('',#46639,10.);
#13417=VECTOR('',#46640,10.);
#13418=VECTOR('',#46647,10.);
#13419=VECTOR('',#46648,10.);
#13420=VECTOR('',#46649,10.);
#13421=VECTOR('',#46650,10.);
#13422=VECTOR('',#46655,10.);
#13423=VECTOR('',#46658,10.);
#13424=VECTOR('',#46659,10.);
#13425=VECTOR('',#46666,10.);
#13426=VECTOR('',#46667,10.);
#13427=VECTOR('',#46668,10.);
#13428=VECTOR('',#46669,10.);
#13429=VECTOR('',#46674,10.);
#13430=VECTOR('',#46677,10.);
#13431=VECTOR('',#46678,10.);
#13432=VECTOR('',#46685,10.);
#13433=VECTOR('',#46686,10.);
#13434=VECTOR('',#46687,10.);
#13435=VECTOR('',#46688,10.);
#13436=VECTOR('',#46693,10.);
#13437=VECTOR('',#46696,10.);
#13438=VECTOR('',#46697,10.);
#13439=VECTOR('',#46704,10.);
#13440=VECTOR('',#46705,10.);
#13441=VECTOR('',#46706,10.);
#13442=VECTOR('',#46707,10.);
#13443=VECTOR('',#46712,10.);
#13444=VECTOR('',#46715,10.);
#13445=VECTOR('',#46716,10.);
#13446=VECTOR('',#46723,10.);
#13447=VECTOR('',#46724,10.);
#13448=VECTOR('',#46725,10.);
#13449=VECTOR('',#46726,10.);
#13450=VECTOR('',#46731,10.);
#13451=VECTOR('',#46736,10.);
#13452=VECTOR('',#46737,10.);
#13453=VECTOR('',#46746,10.);
#13454=VECTOR('',#46747,10.);
#13455=VECTOR('',#46748,10.);
#13456=VECTOR('',#46749,10.);
#13457=VECTOR('',#46754,10.);
#13458=VECTOR('',#46757,10.);
#13459=VECTOR('',#46758,10.);
#13460=VECTOR('',#46765,10.);
#13461=VECTOR('',#46766,10.);
#13462=VECTOR('',#46767,10.);
#13463=VECTOR('',#46768,10.);
#13464=VECTOR('',#46773,10.);
#13465=VECTOR('',#46776,10.);
#13466=VECTOR('',#46777,10.);
#13467=VECTOR('',#46784,10.);
#13468=VECTOR('',#46785,10.);
#13469=VECTOR('',#46786,10.);
#13470=VECTOR('',#46787,10.);
#13471=VECTOR('',#46792,10.);
#13472=VECTOR('',#46795,10.);
#13473=VECTOR('',#46796,10.);
#13474=VECTOR('',#46803,10.);
#13475=VECTOR('',#46804,10.);
#13476=VECTOR('',#46805,10.);
#13477=VECTOR('',#46806,10.);
#13478=VECTOR('',#46811,10.);
#13479=VECTOR('',#46814,10.);
#13480=VECTOR('',#46815,10.);
#13481=VECTOR('',#46822,10.);
#13482=VECTOR('',#46823,10.);
#13483=VECTOR('',#46824,10.);
#13484=VECTOR('',#46825,10.);
#13485=VECTOR('',#46830,10.);
#13486=VECTOR('',#46833,10.);
#13487=VECTOR('',#46834,10.);
#13488=VECTOR('',#46841,10.);
#13489=VECTOR('',#46842,10.);
#13490=VECTOR('',#46843,10.);
#13491=VECTOR('',#46844,10.);
#13492=VECTOR('',#46849,10.);
#13493=VECTOR('',#46852,10.);
#13494=VECTOR('',#46853,10.);
#13495=VECTOR('',#46860,10.);
#13496=VECTOR('',#46861,10.);
#13497=VECTOR('',#46862,10.);
#13498=VECTOR('',#46863,10.);
#13499=VECTOR('',#46868,10.);
#13500=VECTOR('',#46871,10.);
#13501=VECTOR('',#46872,10.);
#13502=VECTOR('',#46879,10.);
#13503=VECTOR('',#46880,10.);
#13504=VECTOR('',#46881,10.);
#13505=VECTOR('',#46882,10.);
#13506=VECTOR('',#46887,10.);
#13507=VECTOR('',#46890,10.);
#13508=VECTOR('',#46891,10.);
#13509=VECTOR('',#46898,10.);
#13510=VECTOR('',#46899,10.);
#13511=VECTOR('',#46900,10.);
#13512=VECTOR('',#46901,10.);
#13513=VECTOR('',#46906,10.);
#13514=VECTOR('',#46909,10.);
#13515=VECTOR('',#46910,10.);
#13516=VECTOR('',#46917,10.);
#13517=VECTOR('',#46918,10.);
#13518=VECTOR('',#46919,10.);
#13519=VECTOR('',#46920,10.);
#13520=VECTOR('',#46925,10.);
#13521=VECTOR('',#46928,10.);
#13522=VECTOR('',#46929,10.);
#13523=VECTOR('',#46936,10.);
#13524=VECTOR('',#46937,10.);
#13525=VECTOR('',#46938,10.);
#13526=VECTOR('',#46939,10.);
#13527=VECTOR('',#46944,10.);
#13528=VECTOR('',#46947,10.);
#13529=VECTOR('',#46948,10.);
#13530=VECTOR('',#46955,10.);
#13531=VECTOR('',#46956,10.);
#13532=VECTOR('',#46957,10.);
#13533=VECTOR('',#46958,10.);
#13534=VECTOR('',#46963,10.);
#13535=VECTOR('',#46966,10.);
#13536=VECTOR('',#46967,10.);
#13537=VECTOR('',#46974,10.);
#13538=VECTOR('',#46975,10.);
#13539=VECTOR('',#46976,10.);
#13540=VECTOR('',#46977,10.);
#13541=VECTOR('',#46982,10.);
#13542=VECTOR('',#46985,10.);
#13543=VECTOR('',#46986,10.);
#13544=VECTOR('',#46993,10.);
#13545=VECTOR('',#46994,10.);
#13546=VECTOR('',#46995,10.);
#13547=VECTOR('',#46996,10.);
#13548=VECTOR('',#47001,10.);
#13549=VECTOR('',#47004,10.);
#13550=VECTOR('',#47005,10.);
#13551=VECTOR('',#47012,10.);
#13552=VECTOR('',#47013,10.);
#13553=VECTOR('',#47014,10.);
#13554=VECTOR('',#47015,10.);
#13555=VECTOR('',#47020,10.);
#13556=VECTOR('',#47023,10.);
#13557=VECTOR('',#47024,10.);
#13558=VECTOR('',#47031,10.);
#13559=VECTOR('',#47032,10.);
#13560=VECTOR('',#47033,10.);
#13561=VECTOR('',#47034,10.);
#13562=VECTOR('',#47039,10.);
#13563=VECTOR('',#47042,10.);
#13564=VECTOR('',#47043,10.);
#13565=VECTOR('',#47050,10.);
#13566=VECTOR('',#47051,10.);
#13567=VECTOR('',#47052,10.);
#13568=VECTOR('',#47053,10.);
#13569=VECTOR('',#47058,10.);
#13570=VECTOR('',#47061,10.);
#13571=VECTOR('',#47062,10.);
#13572=VECTOR('',#47069,10.);
#13573=VECTOR('',#47070,10.);
#13574=VECTOR('',#47071,10.);
#13575=VECTOR('',#47072,10.);
#13576=VECTOR('',#47077,10.);
#13577=VECTOR('',#47080,10.);
#13578=VECTOR('',#47081,10.);
#13579=VECTOR('',#47090,7.17);
#13580=VECTOR('',#47091,7.17);
#13581=VECTOR('',#47094,6.76);
#13582=VECTOR('',#47101,8.9203817394342);
#13583=VECTOR('',#47132,10.);
#13584=VECTOR('',#47133,10.);
#13585=VECTOR('',#47134,10.);
#13586=VECTOR('',#47137,10.);
#13587=VECTOR('',#47138,10.);
#13588=VECTOR('',#47139,10.);
#13589=VECTOR('',#47142,10.);
#13590=VECTOR('',#47143,10.);
#13591=VECTOR('',#47144,10.);
#13592=VECTOR('',#47147,10.);
#13593=VECTOR('',#47148,10.);
#13594=VECTOR('',#47151,10.);
#13595=VECTOR('',#47154,10.);
#13596=VECTOR('',#47155,10.);
#13597=VECTOR('',#47156,10.);
#13598=VECTOR('',#47159,10.);
#13599=VECTOR('',#47162,10.);
#13600=VECTOR('',#47163,10.);
#13601=VECTOR('',#47164,10.);
#13602=VECTOR('',#47167,10.);
#13603=VECTOR('',#47168,10.);
#13604=VECTOR('',#47171,10.);
#13605=VECTOR('',#47174,10.);
#13606=VECTOR('',#47175,10.);
#13607=VECTOR('',#47176,10.);
#13608=VECTOR('',#47179,10.);
#13609=VECTOR('',#47180,10.);
#13610=VECTOR('',#47183,10.);
#13611=VECTOR('',#47186,10.);
#13612=VECTOR('',#47189,10.);
#13613=VECTOR('',#47192,10.);
#13614=VECTOR('',#47193,10.);
#13615=VECTOR('',#47196,10.);
#13616=VECTOR('',#47197,10.);
#13617=VECTOR('',#47200,10.);
#13618=VECTOR('',#47201,10.);
#13619=VECTOR('',#47204,10.);
#13620=VECTOR('',#47205,10.);
#13621=VECTOR('',#47208,10.);
#13622=VECTOR('',#47209,10.);
#13623=VECTOR('',#47212,10.);
#13624=VECTOR('',#47213,10.);
#13625=VECTOR('',#47216,10.);
#13626=VECTOR('',#47217,10.);
#13627=VECTOR('',#47220,10.);
#13628=VECTOR('',#47221,10.);
#13629=VECTOR('',#47224,10.);
#13630=VECTOR('',#47225,10.);
#13631=VECTOR('',#47246,6.8);
#13632=VECTOR('',#47251,8.35);
#13633=VECTOR('',#47260,6.4);
#13634=CIRCLE('',#34368,40.);
#13635=CIRCLE('',#34369,40.);
#13636=CIRCLE('',#34370,39.5527864045);
#13637=CIRCLE('',#34371,39.5527864045);
#13638=CIRCLE('',#34373,37.4472135955);
#13639=CIRCLE('',#34374,37.4472135955);
#13640=CIRCLE('',#34376,40.);
#13641=CIRCLE('',#34378,36.5);
#13642=CIRCLE('',#34380,33.2);
#13643=CIRCLE('',#34382,26.5);
#13644=CIRCLE('',#34383,26.);
#13645=CIRCLE('',#34384,26.);
#13646=CIRCLE('',#34386,26.);
#13647=CIRCLE('',#34388,29.58);
#13648=CIRCLE('',#34390,31.5);
#13649=CIRCLE('',#34391,32.3535533905933);
#13650=CIRCLE('',#34392,32.3535533905933);
#13651=CIRCLE('',#34394,33.6464466094067);
#13652=CIRCLE('',#34395,33.6464466094067);
#13653=CIRCLE('',#34397,25.16);
#13654=CIRCLE('',#34399,34.0540295903842);
#13655=CIRCLE('',#34400,34.0540295903842);
#13656=CIRCLE('',#34402,36.5);
#13657=CIRCLE('',#34404,126.506803038084);
#13658=CIRCLE('',#34405,126.506803038084);
#13659=CIRCLE('',#34406,127.416025147169);
#13660=CIRCLE('',#34407,127.416025147169);
#13661=CIRCLE('',#34409,131.083974852831);
#13662=CIRCLE('',#34410,131.083974852831);
#13663=CIRCLE('',#34412,121.);
#13664=CIRCLE('',#34414,131.8);
#13665=CIRCLE('',#34415,131.8);
#13666=CIRCLE('',#34417,134.2);
#13667=CIRCLE('',#34418,134.2);
#13668=CIRCLE('',#34420,134.675561720794);
#13669=CIRCLE('',#34421,134.675561720794);
#13670=CIRCLE('',#34423,135.824438279206);
#13671=CIRCLE('',#34424,135.824438279206);
#13672=CIRCLE('',#34426,136.);
#13673=CIRCLE('',#34427,136.);
#13674=CIRCLE('',#34429,136.);
#13675=CIRCLE('',#34432,136.);
#13676=CIRCLE('',#34433,136.);
#13677=CIRCLE('',#34434,136.);
#13678=CIRCLE('',#34437,136.);
#13679=CIRCLE('',#34439,136.);
#13680=CIRCLE('',#34442,136.);
#13681=CIRCLE('',#34445,136.);
#13682=CIRCLE('',#34448,136.);
#13683=CIRCLE('',#34451,136.);
#13684=CIRCLE('',#34454,136.);
#13685=CIRCLE('',#34457,136.);
#13686=CIRCLE('',#34460,136.);
#13687=CIRCLE('',#34463,136.);
#13688=CIRCLE('',#34466,136.);
#13689=CIRCLE('',#34469,136.);
#13690=CIRCLE('',#34472,136.);
#13691=CIRCLE('',#34475,136.);
#13692=CIRCLE('',#34478,136.);
#13693=CIRCLE('',#34481,136.);
#13694=CIRCLE('',#34484,136.);
#13695=CIRCLE('',#34487,136.);
#13696=CIRCLE('',#34490,136.);
#13697=CIRCLE('',#34493,136.);
#13698=CIRCLE('',#34496,136.);
#13699=CIRCLE('',#34499,136.);
#13700=CIRCLE('',#34502,136.);
#13701=CIRCLE('',#34505,136.);
#13702=CIRCLE('',#34508,136.);
#13703=CIRCLE('',#34511,136.);
#13704=CIRCLE('',#34514,136.);
#13705=CIRCLE('',#34517,136.);
#13706=CIRCLE('',#34520,136.);
#13707=CIRCLE('',#34523,136.);
#13708=CIRCLE('',#34526,136.);
#13709=CIRCLE('',#34529,136.);
#13710=CIRCLE('',#34532,136.);
#13711=CIRCLE('',#34535,136.);
#13712=CIRCLE('',#34538,136.);
#13713=CIRCLE('',#34541,136.);
#13714=CIRCLE('',#34544,136.);
#13715=CIRCLE('',#34547,136.);
#13716=CIRCLE('',#34550,136.);
#13717=CIRCLE('',#34553,136.);
#13718=CIRCLE('',#34556,136.);
#13719=CIRCLE('',#34559,136.);
#13720=CIRCLE('',#34562,136.);
#13721=CIRCLE('',#34565,136.);
#13722=CIRCLE('',#34568,136.);
#13723=CIRCLE('',#34571,136.);
#13724=CIRCLE('',#34574,136.);
#13725=CIRCLE('',#34577,136.);
#13726=CIRCLE('',#34580,136.);
#13727=CIRCLE('',#34583,136.);
#13728=CIRCLE('',#34586,136.);
#13729=CIRCLE('',#34589,136.);
#13730=CIRCLE('',#34592,136.);
#13731=CIRCLE('',#34595,136.);
#13732=CIRCLE('',#34598,136.);
#13733=CIRCLE('',#34601,136.);
#13734=CIRCLE('',#34604,136.);
#13735=CIRCLE('',#34607,136.);
#13736=CIRCLE('',#34610,136.);
#13737=CIRCLE('',#34613,136.);
#13738=CIRCLE('',#34616,136.);
#13739=CIRCLE('',#34619,136.);
#13740=CIRCLE('',#34622,136.);
#13741=CIRCLE('',#34625,136.);
#13742=CIRCLE('',#34628,136.);
#13743=CIRCLE('',#34631,136.);
#13744=CIRCLE('',#34634,136.);
#13745=CIRCLE('',#34637,136.);
#13746=CIRCLE('',#34640,136.);
#13747=CIRCLE('',#34643,136.);
#13748=CIRCLE('',#34646,136.);
#13749=CIRCLE('',#34649,136.);
#13750=CIRCLE('',#34652,136.);
#13751=CIRCLE('',#34655,136.);
#13752=CIRCLE('',#34658,136.);
#13753=CIRCLE('',#34661,136.);
#13754=CIRCLE('',#34664,136.);
#13755=CIRCLE('',#34667,136.);
#13756=CIRCLE('',#34670,136.);
#13757=CIRCLE('',#34673,136.);
#13758=CIRCLE('',#34676,136.);
#13759=CIRCLE('',#34679,136.);
#13760=CIRCLE('',#34682,136.);
#13761=CIRCLE('',#34685,136.);
#13762=CIRCLE('',#34688,136.);
#13763=CIRCLE('',#34691,136.);
#13764=CIRCLE('',#34694,136.);
#13765=CIRCLE('',#34697,136.);
#13766=CIRCLE('',#34700,136.);
#13767=CIRCLE('',#34703,136.);
#13768=CIRCLE('',#34706,136.);
#13769=CIRCLE('',#34709,136.);
#13770=CIRCLE('',#34712,136.);
#13771=CIRCLE('',#34715,136.);
#13772=CIRCLE('',#34718,136.);
#13773=CIRCLE('',#34721,136.);
#13774=CIRCLE('',#34724,136.);
#13775=CIRCLE('',#34727,136.);
#13776=CIRCLE('',#34730,136.);
#13777=CIRCLE('',#34733,136.);
#13778=CIRCLE('',#34736,136.);
#13779=CIRCLE('',#34739,136.);
#13780=CIRCLE('',#34742,136.);
#13781=CIRCLE('',#34745,136.);
#13782=CIRCLE('',#34748,136.);
#13783=CIRCLE('',#34751,136.);
#13784=CIRCLE('',#34754,136.);
#13785=CIRCLE('',#34757,136.);
#13786=CIRCLE('',#34760,136.);
#13787=CIRCLE('',#34763,136.);
#13788=CIRCLE('',#34766,136.);
#13789=CIRCLE('',#34769,136.);
#13790=CIRCLE('',#34772,136.);
#13791=CIRCLE('',#34775,136.);
#13792=CIRCLE('',#34778,136.);
#13793=CIRCLE('',#34781,136.);
#13794=CIRCLE('',#34784,136.);
#13795=CIRCLE('',#34787,136.);
#13796=CIRCLE('',#34790,136.);
#13797=CIRCLE('',#34793,136.);
#13798=CIRCLE('',#34796,136.);
#13799=CIRCLE('',#34799,136.);
#13800=CIRCLE('',#34802,136.);
#13801=CIRCLE('',#34805,136.);
#13802=CIRCLE('',#34808,136.);
#13803=CIRCLE('',#34811,136.);
#13804=CIRCLE('',#34814,136.);
#13805=CIRCLE('',#34817,136.);
#13806=CIRCLE('',#34820,136.);
#13807=CIRCLE('',#34823,136.);
#13808=CIRCLE('',#34826,136.);
#13809=CIRCLE('',#34829,136.);
#13810=CIRCLE('',#34832,136.);
#13811=CIRCLE('',#34835,136.);
#13812=CIRCLE('',#34838,136.);
#13813=CIRCLE('',#34841,136.);
#13814=CIRCLE('',#34844,136.);
#13815=CIRCLE('',#34847,136.);
#13816=CIRCLE('',#34850,136.);
#13817=CIRCLE('',#34853,136.);
#13818=CIRCLE('',#34856,136.);
#13819=CIRCLE('',#34859,136.);
#13820=CIRCLE('',#34862,136.);
#13821=CIRCLE('',#34865,51.5);
#13822=CIRCLE('',#34866,52.);
#13823=CIRCLE('',#34868,14.5);
#13824=CIRCLE('',#34869,15.);
#13825=CIRCLE('',#34871,51.5);
#13826=CIRCLE('',#34872,52.);
#13827=CIRCLE('',#34874,14.5);
#13828=CIRCLE('',#34875,15.);
#13829=CIRCLE('',#34877,51.5);
#13830=CIRCLE('',#34878,52.);
#13831=CIRCLE('',#34880,14.5);
#13832=CIRCLE('',#34881,15.);
#13833=CIRCLE('',#34883,52.);
#13834=CIRCLE('',#34884,51.5);
#13835=CIRCLE('',#34886,15.);
#13836=CIRCLE('',#34887,14.5);
#13837=CIRCLE('',#34889,52.);
#13838=CIRCLE('',#34890,51.5);
#13839=CIRCLE('',#34892,15.);
#13840=CIRCLE('',#34893,14.5);
#13841=CIRCLE('',#34895,15.);
#13842=CIRCLE('',#34897,52.);
#13843=CIRCLE('',#34899,15.);
#13844=CIRCLE('',#34901,52.);
#13845=CIRCLE('',#34903,15.);
#13846=CIRCLE('',#34905,52.);
#13847=CIRCLE('',#34907,7.18);
#13848=CIRCLE('',#34908,7.18);
#13849=CIRCLE('',#34909,7.18);
#13850=CIRCLE('',#34910,7.18);
#13851=CIRCLE('',#34911,7.18);
#13852=CIRCLE('',#35921,127.371647073124);
#13853=CIRCLE('',#35922,127.371647073124);
#13854=CIRCLE('',#35923,127.);
#13855=CIRCLE('',#35924,127.);
#13856=CIRCLE('',#35926,128.628352926876);
#13857=CIRCLE('',#35927,128.628352926876);
#13858=CIRCLE('',#35929,127.);
#13859=CIRCLE('',#35961,138.506803038084);
#13860=CIRCLE('',#35962,138.506803038084);
#13861=CIRCLE('',#35963,139.);
#13862=CIRCLE('',#35964,139.);
#13863=CIRCLE('',#35966,139.);
#13864=CIRCLE('',#35967,139.);
#13865=CIRCLE('',#35970,129.5);
#13866=CIRCLE('',#35972,137.5);
#13867=CIRCLE('',#35974,138.646446609407);
#13868=CIRCLE('',#35976,138.353553390593);
#13869=CIRCLE('',#36123,7.18);
#13870=CIRCLE('',#36125,7.18);
#13871=CIRCLE('',#36127,7.18);
#13872=CIRCLE('',#36129,7.18);
#13873=CIRCLE('',#36131,7.18);
#13874=CIRCLE('',#36133,27.);
#13875=CIRCLE('',#36134,23.);
#13876=CIRCLE('',#36136,23.);
#13877=CIRCLE('',#36138,15.);
#13878=CIRCLE('',#36140,52.);
#13879=CIRCLE('',#36142,15.);
#13880=CIRCLE('',#36144,52.);
#13881=CIRCLE('',#36147,25.16);
#13882=CIRCLE('',#36150,27.);
#13883=CIRCLE('',#36153,29.58);
#13884=CIRCLE('',#36155,32.6);
#13885=CIRCLE('',#36157,32.6);
#13886=CIRCLE('',#36160,46.);
#13887=CIRCLE('',#36162,123.);
#13888=CIRCLE('',#36164,126.5);
#13889=CIRCLE('',#36174,11.59764);
#13890=CIRCLE('',#36178,3.4268292682927);
#13891=CIRCLE('',#36179,2.63157427110059);
#13892=CIRCLE('',#36182,12.);
#13893=CIRCLE('',#36219,7.25);
#13894=CIRCLE('',#36220,6.75);
#13895=CIRCLE('',#36222,7.25);
#13896=CIRCLE('',#36223,7.25);
#13897=CIRCLE('',#36224,25.4);
#13898=CIRCLE('',#36225,7.25);
#13899=CIRCLE('',#36227,6.75);
#13900=CIRCLE('',#36229,6.75);
#13901=CIRCLE('',#36231,6.75);
#13902=CIRCLE('',#36233,6.75);
#13903=CIRCLE('',#36235,6.75);
#13904=CIRCLE('',#36237,6.75);
#13905=CIRCLE('',#36239,6.75);
#13906=CIRCLE('',#36241,7.25);
#13907=CIRCLE('',#36243,7.25);
#13908=CIRCLE('',#36244,7.25);
#13909=CIRCLE('',#36245,25.4);
#13910=CIRCLE('',#36246,7.25);
#13911=CIRCLE('',#36257,25.4);
#13912=CIRCLE('',#36258,25.4);
#13913=CIRCLE('',#36259,25.0464466094067);
#13914=CIRCLE('',#36260,25.0464466094067);
#13915=CIRCLE('',#36262,24.9535533905933);
#13916=CIRCLE('',#36263,24.9535533905933);
#13917=CIRCLE('',#36266,24.1);
#13918=CIRCLE('',#36270,11.59764);
#13919=CIRCLE('',#36275,12.61364);
#13920=CIRCLE('',#36276,12.61364);
#13921=CIRCLE('',#36278,12.61364);
#13922=CIRCLE('',#36279,12.61364);
#13923=CIRCLE('',#36280,12.61364);
#13924=CIRCLE('',#36282,2.20000000000001);
#13925=CIRCLE('',#36293,2.20000000000001);
#13926=CIRCLE('',#36298,12.61364);
#13927=CIRCLE('',#36300,12.61364);
#13928=CIRCLE('',#36308,12.61364);
#13929=CIRCLE('',#36313,21.8313);
#13930=CIRCLE('',#36315,21.8313);
#13931=CIRCLE('',#36317,17.97);
#13932=CIRCLE('',#36319,17.47);
#13933=CIRCLE('',#36321,17.47);
#13934=CIRCLE('',#36323,13.97);
#13935=CIRCLE('',#36325,13.47);
#13936=CIRCLE('',#36327,13.47);
#13937=CIRCLE('',#36330,13.47);
#13938=CIRCLE('',#36331,13.47);
#13939=CIRCLE('',#36334,11.9);
#13940=CIRCLE('',#36336,11.9);
#13941=CIRCLE('',#36343,24.5);
#13942=CIRCLE('',#36344,24.5);
#13943=CIRCLE('',#36345,24.88);
#13944=CIRCLE('',#36347,32.185);
#13945=CIRCLE('',#36349,24.5);
#13946=CIRCLE('',#36351,29.78);
#13947=CIRCLE('',#36352,29.4);
#13948=CIRCLE('',#36353,29.4);
#13949=CIRCLE('',#36355,32.185);
#13950=CIRCLE('',#36357,29.4);
#13951=CIRCLE('',#36359,26.2);
#13952=CIRCLE('',#36360,0.8);
#13953=CIRCLE('',#36361,24.6);
#13954=CIRCLE('',#36363,23.7);
#13955=CIRCLE('',#36365,32.585);
#13956=CIRCLE('',#36367,32.585);
#13957=CIRCLE('',#36370,23.4);
#13958=CIRCLE('',#36372,21.8413);
#13959=CIRCLE('',#36374,21.8413);
#13960=CIRCLE('',#36379,29.5655);
#13961=CIRCLE('',#36380,28.7655);
#13962=CIRCLE('',#36382,29.5655);
#13963=CIRCLE('',#36384,28.9655);
#13964=CIRCLE('',#36386,28.508778116497);
#13965=CIRCLE('',#36388,28.208778116497);
#13966=CIRCLE('',#36390,26.4446922201623);
#13967=CIRCLE('',#36392,26.8655);
#13968=CIRCLE('',#36396,25.8846416389917);
#13969=CIRCLE('',#36397,25.8846416389917);
#13970=CIRCLE('',#36398,25.3846416389917);
#13971=CIRCLE('',#36400,22.4888907487754);
#13972=CIRCLE('',#36402,25.8846416389917);
#13973=CIRCLE('',#36404,22.2743990607509);
#13974=CIRCLE('',#36405,22.7743990607509);
#13975=CIRCLE('',#36406,22.7743990607509);
#13976=CIRCLE('',#36408,22.7743990607509);
#13977=CIRCLE('',#36410,21.5342155525986);
#13978=CIRCLE('',#36412,2.52960515816076);
#13979=CIRCLE('',#36413,0.3);
#13980=CIRCLE('',#36414,2.22978791005503);
#13981=CIRCLE('',#36415,2.52960515816076);
#13982=CIRCLE('',#36417,2.8696636114714);
#13983=CIRCLE('',#36418,2.8696636114714);
#13984=CIRCLE('',#36420,2.56984636336567);
#13985=CIRCLE('',#36421,0.3);
#13986=CIRCLE('',#36425,2.52960515816076);
#13987=CIRCLE('',#36426,0.3);
#13988=CIRCLE('',#36427,2.22978791005503);
#13989=CIRCLE('',#36428,2.52960515816076);
#13990=CIRCLE('',#36430,2.8696636114714);
#13991=CIRCLE('',#36431,2.8696636114714);
#13992=CIRCLE('',#36433,2.56984636336567);
#13993=CIRCLE('',#36434,0.3);
#13994=CIRCLE('',#36438,2.52960515816076);
#13995=CIRCLE('',#36439,0.3);
#13996=CIRCLE('',#36440,2.22978791005503);
#13997=CIRCLE('',#36441,2.52960515816076);
#13998=CIRCLE('',#36443,2.8696636114714);
#13999=CIRCLE('',#36444,2.8696636114714);
#14000=CIRCLE('',#36446,2.56984636336567);
#14001=CIRCLE('',#36447,0.3);
#14002=CIRCLE('',#36451,2.52960515816076);
#14003=CIRCLE('',#36452,0.3);
#14004=CIRCLE('',#36453,2.22978791005503);
#14005=CIRCLE('',#36454,2.52960515816076);
#14006=CIRCLE('',#36456,2.8696636114714);
#14007=CIRCLE('',#36457,2.8696636114714);
#14008=CIRCLE('',#36459,2.56984636336567);
#14009=CIRCLE('',#36460,0.3);
#14010=CIRCLE('',#36464,2.52960515816076);
#14011=CIRCLE('',#36465,0.3);
#14012=CIRCLE('',#36466,2.22978791005503);
#14013=CIRCLE('',#36467,2.52960515816076);
#14014=CIRCLE('',#36469,2.8696636114714);
#14015=CIRCLE('',#36470,2.8696636114714);
#14016=CIRCLE('',#36472,2.56984636336567);
#14017=CIRCLE('',#36473,0.3);
#14018=CIRCLE('',#36477,2.52960515816076);
#14019=CIRCLE('',#36478,0.3);
#14020=CIRCLE('',#36479,2.22978791005503);
#14021=CIRCLE('',#36480,2.52960515816076);
#14022=CIRCLE('',#36482,2.8696636114714);
#14023=CIRCLE('',#36483,2.8696636114714);
#14024=CIRCLE('',#36485,2.56984636336567);
#14025=CIRCLE('',#36486,0.3);
#14026=CIRCLE('',#36490,2.52960515816076);
#14027=CIRCLE('',#36491,0.3);
#14028=CIRCLE('',#36492,2.22978791005503);
#14029=CIRCLE('',#36493,2.52960515816076);
#14030=CIRCLE('',#36495,2.8696636114714);
#14031=CIRCLE('',#36496,2.8696636114714);
#14032=CIRCLE('',#36498,2.56984636336567);
#14033=CIRCLE('',#36499,0.3);
#14034=CIRCLE('',#36503,2.52960515816076);
#14035=CIRCLE('',#36504,0.3);
#14036=CIRCLE('',#36505,2.22978791005503);
#14037=CIRCLE('',#36506,2.52960515816076);
#14038=CIRCLE('',#36508,2.8696636114714);
#14039=CIRCLE('',#36509,2.8696636114714);
#14040=CIRCLE('',#36511,2.56984636336567);
#14041=CIRCLE('',#36512,0.3);
#14042=CIRCLE('',#36516,2.52960515816076);
#14043=CIRCLE('',#36517,0.3);
#14044=CIRCLE('',#36518,2.22978791005503);
#14045=CIRCLE('',#36519,2.52960515816076);
#14046=CIRCLE('',#36521,2.8696636114714);
#14047=CIRCLE('',#36522,2.8696636114714);
#14048=CIRCLE('',#36524,2.56984636336567);
#14049=CIRCLE('',#36525,0.3);
#14050=CIRCLE('',#36529,2.52960515816076);
#14051=CIRCLE('',#36530,0.3);
#14052=CIRCLE('',#36531,2.22978791005503);
#14053=CIRCLE('',#36532,2.52960515816076);
#14054=CIRCLE('',#36534,2.8696636114714);
#14055=CIRCLE('',#36535,2.8696636114714);
#14056=CIRCLE('',#36537,2.56984636336567);
#14057=CIRCLE('',#36538,0.3);
#14058=CIRCLE('',#36542,2.52960515816076);
#14059=CIRCLE('',#36543,0.3);
#14060=CIRCLE('',#36544,2.22978791005503);
#14061=CIRCLE('',#36545,2.52960515816076);
#14062=CIRCLE('',#36547,2.8696636114714);
#14063=CIRCLE('',#36548,2.8696636114714);
#14064=CIRCLE('',#36550,2.56984636336567);
#14065=CIRCLE('',#36551,0.3);
#14066=CIRCLE('',#36555,2.52960515816076);
#14067=CIRCLE('',#36556,0.3);
#14068=CIRCLE('',#36557,2.22978791005503);
#14069=CIRCLE('',#36558,2.52960515816076);
#14070=CIRCLE('',#36560,2.8696636114714);
#14071=CIRCLE('',#36561,2.8696636114714);
#14072=CIRCLE('',#36563,2.56984636336567);
#14073=CIRCLE('',#36564,0.3);
#14074=CIRCLE('',#36568,2.52960515816076);
#14075=CIRCLE('',#36569,0.3);
#14076=CIRCLE('',#36570,2.22978791005503);
#14077=CIRCLE('',#36571,2.52960515816076);
#14078=CIRCLE('',#36573,2.8696636114714);
#14079=CIRCLE('',#36574,2.8696636114714);
#14080=CIRCLE('',#36576,2.56984636336567);
#14081=CIRCLE('',#36577,0.3);
#14082=CIRCLE('',#36581,2.52960515816076);
#14083=CIRCLE('',#36582,0.3);
#14084=CIRCLE('',#36583,2.22978791005503);
#14085=CIRCLE('',#36584,2.52960515816076);
#14086=CIRCLE('',#36586,2.8696636114714);
#14087=CIRCLE('',#36587,2.8696636114714);
#14088=CIRCLE('',#36589,2.56984636336567);
#14089=CIRCLE('',#36590,0.3);
#14090=CIRCLE('',#36594,2.52960515816076);
#14091=CIRCLE('',#36595,0.3);
#14092=CIRCLE('',#36596,2.22978791005503);
#14093=CIRCLE('',#36597,2.52960515816076);
#14094=CIRCLE('',#36599,2.8696636114714);
#14095=CIRCLE('',#36600,2.8696636114714);
#14096=CIRCLE('',#36602,2.56984636336567);
#14097=CIRCLE('',#36603,0.3);
#14098=CIRCLE('',#36607,2.52960515816076);
#14099=CIRCLE('',#36608,0.3);
#14100=CIRCLE('',#36609,2.22978791005503);
#14101=CIRCLE('',#36610,2.52960515816076);
#14102=CIRCLE('',#36612,2.8696636114714);
#14103=CIRCLE('',#36613,2.8696636114714);
#14104=CIRCLE('',#36615,2.56984636336567);
#14105=CIRCLE('',#36616,0.3);
#14106=CIRCLE('',#36620,2.52960515816076);
#14107=CIRCLE('',#36621,0.3);
#14108=CIRCLE('',#36622,2.22978791005503);
#14109=CIRCLE('',#36623,2.52960515816076);
#14110=CIRCLE('',#36625,2.8696636114714);
#14111=CIRCLE('',#36626,2.8696636114714);
#14112=CIRCLE('',#36628,2.56984636336567);
#14113=CIRCLE('',#36629,0.3);
#14114=CIRCLE('',#36633,2.52960515816076);
#14115=CIRCLE('',#36634,0.3);
#14116=CIRCLE('',#36635,2.22978791005503);
#14117=CIRCLE('',#36636,2.52960515816076);
#14118=CIRCLE('',#36638,2.8696636114714);
#14119=CIRCLE('',#36639,2.8696636114714);
#14120=CIRCLE('',#36641,2.56984636336567);
#14121=CIRCLE('',#36642,0.3);
#14122=CIRCLE('',#36646,2.52960515816076);
#14123=CIRCLE('',#36647,0.3);
#14124=CIRCLE('',#36648,2.22978791005503);
#14125=CIRCLE('',#36649,2.52960515816076);
#14126=CIRCLE('',#36651,2.8696636114714);
#14127=CIRCLE('',#36652,2.8696636114714);
#14128=CIRCLE('',#36654,2.56984636336567);
#14129=CIRCLE('',#36655,0.3);
#14130=CIRCLE('',#36659,2.52960515816076);
#14131=CIRCLE('',#36660,0.3);
#14132=CIRCLE('',#36661,2.22978791005503);
#14133=CIRCLE('',#36662,2.52960515816076);
#14134=CIRCLE('',#36664,2.8696636114714);
#14135=CIRCLE('',#36665,2.8696636114714);
#14136=CIRCLE('',#36667,2.56984636336567);
#14137=CIRCLE('',#36668,0.3);
#14138=CIRCLE('',#36672,2.52960515816076);
#14139=CIRCLE('',#36673,0.3);
#14140=CIRCLE('',#36674,2.22978791005503);
#14141=CIRCLE('',#36675,2.52960515816076);
#14142=CIRCLE('',#36677,2.8696636114714);
#14143=CIRCLE('',#36678,2.8696636114714);
#14144=CIRCLE('',#36680,2.56984636336567);
#14145=CIRCLE('',#36681,0.3);
#14146=CIRCLE('',#36685,2.52960515816076);
#14147=CIRCLE('',#36686,0.3);
#14148=CIRCLE('',#36687,2.22978791005503);
#14149=CIRCLE('',#36688,2.52960515816076);
#14150=CIRCLE('',#36690,2.8696636114714);
#14151=CIRCLE('',#36691,2.8696636114714);
#14152=CIRCLE('',#36693,2.56984636336567);
#14153=CIRCLE('',#36694,0.3);
#14154=CIRCLE('',#36698,22.3743990607509);
#14155=CIRCLE('',#36701,25.3846416389917);
#14156=CIRCLE('',#36703,18.294);
#14157=CIRCLE('',#36705,17.494);
#14158=CIRCLE('',#36707,17.494);
#14159=CIRCLE('',#36709,18.094);
#14160=CIRCLE('',#36713,25.146);
#14161=CIRCLE('',#36714,24.346);
#14162=CIRCLE('',#36716,25.146);
#14163=CIRCLE('',#36718,24.546);
#14164=CIRCLE('',#36720,24.0881298772848);
#14165=CIRCLE('',#36722,23.7881298772848);
#14166=CIRCLE('',#36724,22.2251922201623);
#14167=CIRCLE('',#36726,22.646);
#14168=CIRCLE('',#36730,21.6856897166516);
#14169=CIRCLE('',#36731,21.6856897166516);
#14170=CIRCLE('',#36732,21.1856897166516);
#14171=CIRCLE('',#36734,18.5104574586244);
#14172=CIRCLE('',#36736,21.6856897166516);
#14173=CIRCLE('',#36738,18.318471118769);
#14174=CIRCLE('',#36739,18.818471118769);
#14175=CIRCLE('',#36740,18.818471118769);
#14176=CIRCLE('',#36742,18.818471118769);
#14177=CIRCLE('',#36744,17.6684335313922);
#14178=CIRCLE('',#36746,2.35177984678802);
#14179=CIRCLE('',#36747,0.3);
#14180=CIRCLE('',#36748,2.05196259868229);
#14181=CIRCLE('',#36749,2.35177984678802);
#14182=CIRCLE('',#36751,2.64748892284415);
#14183=CIRCLE('',#36752,2.64748892284415);
#14184=CIRCLE('',#36754,2.34767167473842);
#14185=CIRCLE('',#36755,0.3);
#14186=CIRCLE('',#36759,2.35177984678802);
#14187=CIRCLE('',#36760,0.3);
#14188=CIRCLE('',#36761,2.05196259868229);
#14189=CIRCLE('',#36762,2.35177984678802);
#14190=CIRCLE('',#36764,2.64748892284415);
#14191=CIRCLE('',#36765,2.64748892284415);
#14192=CIRCLE('',#36767,2.34767167473842);
#14193=CIRCLE('',#36768,0.3);
#14194=CIRCLE('',#36772,2.35177984678802);
#14195=CIRCLE('',#36773,0.3);
#14196=CIRCLE('',#36774,2.05196259868229);
#14197=CIRCLE('',#36775,2.35177984678802);
#14198=CIRCLE('',#36777,2.64748892284415);
#14199=CIRCLE('',#36778,2.64748892284415);
#14200=CIRCLE('',#36780,2.34767167473842);
#14201=CIRCLE('',#36781,0.3);
#14202=CIRCLE('',#36785,2.35177984678802);
#14203=CIRCLE('',#36786,0.3);
#14204=CIRCLE('',#36787,2.05196259868229);
#14205=CIRCLE('',#36788,2.35177984678802);
#14206=CIRCLE('',#36790,2.64748892284415);
#14207=CIRCLE('',#36791,2.64748892284415);
#14208=CIRCLE('',#36793,2.34767167473842);
#14209=CIRCLE('',#36794,0.3);
#14210=CIRCLE('',#36798,2.35177984678802);
#14211=CIRCLE('',#36799,0.3);
#14212=CIRCLE('',#36800,2.05196259868229);
#14213=CIRCLE('',#36801,2.35177984678802);
#14214=CIRCLE('',#36803,2.64748892284415);
#14215=CIRCLE('',#36804,2.64748892284415);
#14216=CIRCLE('',#36806,2.34767167473842);
#14217=CIRCLE('',#36807,0.3);
#14218=CIRCLE('',#36811,2.35177984678802);
#14219=CIRCLE('',#36812,0.3);
#14220=CIRCLE('',#36813,2.05196259868229);
#14221=CIRCLE('',#36814,2.35177984678802);
#14222=CIRCLE('',#36816,2.64748892284415);
#14223=CIRCLE('',#36817,2.64748892284415);
#14224=CIRCLE('',#36819,2.34767167473842);
#14225=CIRCLE('',#36820,0.3);
#14226=CIRCLE('',#36824,2.35177984678802);
#14227=CIRCLE('',#36825,0.3);
#14228=CIRCLE('',#36826,2.05196259868229);
#14229=CIRCLE('',#36827,2.35177984678802);
#14230=CIRCLE('',#36829,2.64748892284415);
#14231=CIRCLE('',#36830,2.64748892284415);
#14232=CIRCLE('',#36832,2.34767167473842);
#14233=CIRCLE('',#36833,0.3);
#14234=CIRCLE('',#36837,2.35177984678802);
#14235=CIRCLE('',#36838,0.3);
#14236=CIRCLE('',#36839,2.05196259868229);
#14237=CIRCLE('',#36840,2.35177984678802);
#14238=CIRCLE('',#36842,2.64748892284415);
#14239=CIRCLE('',#36843,2.64748892284415);
#14240=CIRCLE('',#36845,2.34767167473842);
#14241=CIRCLE('',#36846,0.3);
#14242=CIRCLE('',#36850,2.35177984678802);
#14243=CIRCLE('',#36851,0.3);
#14244=CIRCLE('',#36852,2.05196259868229);
#14245=CIRCLE('',#36853,2.35177984678802);
#14246=CIRCLE('',#36855,2.64748892284415);
#14247=CIRCLE('',#36856,2.64748892284415);
#14248=CIRCLE('',#36858,2.34767167473842);
#14249=CIRCLE('',#36859,0.3);
#14250=CIRCLE('',#36863,2.35177984678802);
#14251=CIRCLE('',#36864,0.3);
#14252=CIRCLE('',#36865,2.05196259868229);
#14253=CIRCLE('',#36866,2.35177984678802);
#14254=CIRCLE('',#36868,2.64748892284415);
#14255=CIRCLE('',#36869,2.64748892284415);
#14256=CIRCLE('',#36871,2.34767167473842);
#14257=CIRCLE('',#36872,0.3);
#14258=CIRCLE('',#36876,2.35177984678802);
#14259=CIRCLE('',#36877,0.3);
#14260=CIRCLE('',#36878,2.05196259868229);
#14261=CIRCLE('',#36879,2.35177984678802);
#14262=CIRCLE('',#36881,2.64748892284415);
#14263=CIRCLE('',#36882,2.64748892284415);
#14264=CIRCLE('',#36884,2.34767167473842);
#14265=CIRCLE('',#36885,0.3);
#14266=CIRCLE('',#36889,2.35177984678802);
#14267=CIRCLE('',#36890,0.3);
#14268=CIRCLE('',#36891,2.05196259868229);
#14269=CIRCLE('',#36892,2.35177984678802);
#14270=CIRCLE('',#36894,2.64748892284415);
#14271=CIRCLE('',#36895,2.64748892284415);
#14272=CIRCLE('',#36897,2.34767167473842);
#14273=CIRCLE('',#36898,0.3);
#14274=CIRCLE('',#36902,2.35177984678802);
#14275=CIRCLE('',#36903,0.3);
#14276=CIRCLE('',#36904,2.05196259868229);
#14277=CIRCLE('',#36905,2.35177984678802);
#14278=CIRCLE('',#36907,2.64748892284415);
#14279=CIRCLE('',#36908,2.64748892284415);
#14280=CIRCLE('',#36910,2.34767167473842);
#14281=CIRCLE('',#36911,0.3);
#14282=CIRCLE('',#36915,2.35177984678802);
#14283=CIRCLE('',#36916,0.3);
#14284=CIRCLE('',#36917,2.05196259868229);
#14285=CIRCLE('',#36918,2.35177984678802);
#14286=CIRCLE('',#36920,2.64748892284415);
#14287=CIRCLE('',#36921,2.64748892284415);
#14288=CIRCLE('',#36923,2.34767167473842);
#14289=CIRCLE('',#36924,0.3);
#14290=CIRCLE('',#36928,2.35177984678802);
#14291=CIRCLE('',#36929,0.3);
#14292=CIRCLE('',#36930,2.05196259868229);
#14293=CIRCLE('',#36931,2.35177984678802);
#14294=CIRCLE('',#36933,2.64748892284415);
#14295=CIRCLE('',#36934,2.64748892284415);
#14296=CIRCLE('',#36936,2.34767167473842);
#14297=CIRCLE('',#36937,0.3);
#14298=CIRCLE('',#36941,2.35177984678802);
#14299=CIRCLE('',#36942,0.3);
#14300=CIRCLE('',#36943,2.05196259868229);
#14301=CIRCLE('',#36944,2.35177984678802);
#14302=CIRCLE('',#36946,2.64748892284415);
#14303=CIRCLE('',#36947,2.64748892284415);
#14304=CIRCLE('',#36949,2.34767167473842);
#14305=CIRCLE('',#36950,0.3);
#14306=CIRCLE('',#36954,2.35177984678802);
#14307=CIRCLE('',#36955,0.3);
#14308=CIRCLE('',#36956,2.05196259868229);
#14309=CIRCLE('',#36957,2.35177984678802);
#14310=CIRCLE('',#36959,2.64748892284415);
#14311=CIRCLE('',#36960,2.64748892284415);
#14312=CIRCLE('',#36962,2.34767167473842);
#14313=CIRCLE('',#36963,0.3);
#14314=CIRCLE('',#36967,2.35177984678802);
#14315=CIRCLE('',#36968,0.3);
#14316=CIRCLE('',#36969,2.05196259868229);
#14317=CIRCLE('',#36970,2.35177984678802);
#14318=CIRCLE('',#36972,2.64748892284415);
#14319=CIRCLE('',#36973,2.64748892284415);
#14320=CIRCLE('',#36975,2.34767167473842);
#14321=CIRCLE('',#36976,0.3);
#14322=CIRCLE('',#36980,2.35177984678802);
#14323=CIRCLE('',#36981,0.3);
#14324=CIRCLE('',#36982,2.05196259868229);
#14325=CIRCLE('',#36983,2.35177984678802);
#14326=CIRCLE('',#36985,2.64748892284415);
#14327=CIRCLE('',#36986,2.64748892284415);
#14328=CIRCLE('',#36988,2.34767167473842);
#14329=CIRCLE('',#36989,0.3);
#14330=CIRCLE('',#36993,2.35177984678802);
#14331=CIRCLE('',#36994,0.3);
#14332=CIRCLE('',#36995,2.05196259868229);
#14333=CIRCLE('',#36996,2.35177984678802);
#14334=CIRCLE('',#36998,2.64748892284415);
#14335=CIRCLE('',#36999,2.64748892284415);
#14336=CIRCLE('',#37001,2.34767167473842);
#14337=CIRCLE('',#37002,0.3);
#14338=CIRCLE('',#37006,18.418471118769);
#14339=CIRCLE('',#37009,21.1856897166516);
#14340=CIRCLE('',#37011,14.294);
#14341=CIRCLE('',#37013,13.494);
#14342=CIRCLE('',#37015,13.494);
#14343=CIRCLE('',#37017,14.094);
#14344=CIRCLE('',#37026,20.2);
#14345=CIRCLE('',#37027,13.6);
#14346=CIRCLE('',#37029,13.6);
#14347=CIRCLE('',#37031,20.2);
#14348=CIRCLE('',#37033,20.5);
#14349=CIRCLE('',#37035,20.5);
#14350=CIRCLE('',#37040,17.8588235294118);
#14351=CIRCLE('',#37041,13.25);
#14352=CIRCLE('',#37049,13.25);
#14353=CIRCLE('',#37053,12.75);
#14354=CIRCLE('',#37060,13.25);
#14355=CIRCLE('',#37061,12.75);
#14356=CIRCLE('',#37063,17.8588235294118);
#14357=CIRCLE('',#37069,17.8588235294118);
#14358=CIRCLE('',#37072,17.8588235294118);
#14359=CIRCLE('',#37073,13.25);
#14360=CIRCLE('',#37088,13.25);
#14361=CIRCLE('',#37092,12.75);
#14362=CIRCLE('',#37097,17.8588235294118);
#14363=CIRCLE('',#37100,13.25);
#14364=CIRCLE('',#37109,13.25);
#14365=CIRCLE('',#37110,12.75);
#14366=CIRCLE('',#37122,12.75);
#14367=CIRCLE('',#37124,13.25);
#14368=CIRCLE('',#37125,12.75);
#14369=CIRCLE('',#37128,12.75);
#14370=CIRCLE('',#37130,12.75);
#14371=CIRCLE('',#37133,12.75);
#14372=CIRCLE('',#37134,12.75);
#14373=CIRCLE('',#37135,12.75);
#14374=CIRCLE('',#37136,12.75);
#14375=CIRCLE('',#37137,12.75);
#14376=CIRCLE('',#37138,12.75);
#14377=CIRCLE('',#37139,12.75);
#14378=CIRCLE('',#37141,13.25);
#14379=CIRCLE('',#37146,17.8588235294118);
#14380=CIRCLE('',#37155,13.25);
#14381=CIRCLE('',#37158,13.25);
#14382=CIRCLE('',#37162,13.25);
#14383=CIRCLE('',#37172,17.8588235294118);
#14384=CIRCLE('',#37174,13.3071428571429);
#14385=CIRCLE('',#37187,1.95);
#14386=CIRCLE('',#37188,1.95);
#14387=CIRCLE('',#37189,1.75);
#14388=CIRCLE('',#37191,1.95);
#14389=CIRCLE('',#37192,1.95);
#14390=CIRCLE('',#37193,1.95);
#14391=CIRCLE('',#37194,1.95);
#14392=CIRCLE('',#37195,1.95);
#14393=CIRCLE('',#37198,1.55000000000001);
#14394=CIRCLE('',#37208,1.55000000000001);
#14395=CIRCLE('',#37212,0.999999999999996);
#14396=CIRCLE('',#37213,1.29999999999999);
#14397=CIRCLE('',#37217,20.5035615807565);
#14398=CIRCLE('',#37218,20.5035615807565);
#14399=CIRCLE('',#37219,21.4627734781028);
#14400=CIRCLE('',#37220,21.4627734781028);
#14401=CIRCLE('',#37222,22.7372265218972);
#14402=CIRCLE('',#37223,22.7372265218972);
#14403=CIRCLE('',#37225,18.5);
#14404=CIRCLE('',#37227,23.5535533905933);
#14405=CIRCLE('',#37228,23.5535533905933);
#14406=CIRCLE('',#37230,24.4464466094067);
#14407=CIRCLE('',#37231,24.4464466094067);
#14408=CIRCLE('',#37233,24.9708715315434);
#14409=CIRCLE('',#37234,24.9708715315434);
#14410=CIRCLE('',#37236,25.4291284684566);
#14411=CIRCLE('',#37237,25.4291284684566);
#14412=CIRCLE('',#37239,25.6);
#14413=CIRCLE('',#37240,25.6);
#14414=CIRCLE('',#37242,25.6);
#14415=CIRCLE('',#37244,24.52);
#14416=CIRCLE('',#37245,24.32);
#14417=CIRCLE('',#37247,25.12);
#14418=CIRCLE('',#37249,25.12);
#14419=CIRCLE('',#37251,26.8);
#14420=CIRCLE('',#37253,26.8);
#14421=CIRCLE('',#37257,18.4);
#14422=CIRCLE('',#37259,20.7);
#14423=CIRCLE('',#37261,22.6);
#14424=CIRCLE('',#37263,24.);
#14425=CIRCLE('',#37265,24.8);
#14426=CIRCLE('',#37267,24.32);
#14427=CIRCLE('',#37271,6.28269);
#14428=CIRCLE('',#37301,5.57784);
#14429=CIRCLE('',#37303,5.57784);
#14430=CIRCLE('',#37332,5.05);
#14431=CIRCLE('',#37333,5.90355339059328);
#14432=CIRCLE('',#37334,5.90355339059328);
#14433=CIRCLE('',#37336,6.28269);
#14434=CIRCLE('',#37337,6.28269);
#14435=CIRCLE('',#37338,6.28269);
#14436=CIRCLE('',#37342,10.4);
#14437=CIRCLE('',#37343,7.17);
#14438=CIRCLE('',#37346,11.);
#14439=CIRCLE('',#37347,11.);
#14440=CIRCLE('',#37349,10.4);
#14441=CIRCLE('',#37357,6.28269);
#14442=CIRCLE('',#37358,6.28269);
#14443=CIRCLE('',#37359,5.57784);
#14444=CIRCLE('',#37364,7.17);
#14445=CIRCLE('',#37367,7.17);
#14446=CIRCLE('',#37370,7.17);
#14447=CIRCLE('',#37373,7.17);
#14448=CIRCLE('',#37376,7.17);
#14449=CIRCLE('',#37379,7.17);
#14450=CIRCLE('',#37382,7.17);
#14451=CIRCLE('',#37385,7.17);
#14452=CIRCLE('',#37388,7.17);
#14453=CIRCLE('',#37391,7.17);
#14454=CIRCLE('',#37394,7.17);
#14455=CIRCLE('',#37397,7.17);
#14456=CIRCLE('',#37400,7.17);
#14457=CIRCLE('',#37403,7.17);
#14458=CIRCLE('',#37406,7.17);
#14459=CIRCLE('',#37409,7.17);
#14460=CIRCLE('',#37412,7.17);
#14461=CIRCLE('',#37415,7.17);
#14462=CIRCLE('',#37418,7.17);
#14463=CIRCLE('',#37421,7.17);
#14464=CIRCLE('',#37424,7.17);
#14465=CIRCLE('',#37427,7.17);
#14466=CIRCLE('',#37430,7.17);
#14467=CIRCLE('',#37433,7.17);
#14468=CIRCLE('',#37436,7.17);
#14469=CIRCLE('',#37439,7.17);
#14470=CIRCLE('',#37442,7.17);
#14471=CIRCLE('',#37445,7.17);
#14472=CIRCLE('',#37448,7.17);
#14473=CIRCLE('',#37451,7.17);
#14474=CIRCLE('',#37454,7.17);
#14475=CIRCLE('',#37457,7.17);
#14476=CIRCLE('',#37460,7.17);
#14477=CIRCLE('',#37463,7.17);
#14478=CIRCLE('',#37466,7.17);
#14479=CIRCLE('',#37467,7.17);
#14480=CIRCLE('',#37470,7.17);
#14481=CIRCLE('',#37471,7.17);
#14482=CIRCLE('',#37474,7.17);
#14483=CIRCLE('',#37477,7.17);
#14484=CIRCLE('',#37480,7.17);
#14485=CIRCLE('',#37483,7.17);
#14486=CIRCLE('',#37486,7.17);
#14487=CIRCLE('',#37489,7.17);
#14488=CIRCLE('',#37492,7.17);
#14489=CIRCLE('',#37495,7.17);
#14490=CIRCLE('',#37498,7.17);
#14491=CIRCLE('',#37501,7.17);
#14492=CIRCLE('',#37504,7.17);
#14493=CIRCLE('',#37507,7.17);
#14494=CIRCLE('',#37510,7.17);
#14495=CIRCLE('',#37513,7.17);
#14496=CIRCLE('',#37516,7.17);
#14497=CIRCLE('',#37519,7.17);
#14498=CIRCLE('',#37522,7.17);
#14499=CIRCLE('',#37525,7.17);
#14500=CIRCLE('',#37528,7.17);
#14501=CIRCLE('',#37531,7.17);
#14502=CIRCLE('',#37534,7.17);
#14503=CIRCLE('',#37537,7.17);
#14504=CIRCLE('',#37540,7.17);
#14505=CIRCLE('',#37543,7.17);
#14506=CIRCLE('',#37546,7.17);
#14507=CIRCLE('',#37549,7.17);
#14508=CIRCLE('',#37552,7.17);
#14509=CIRCLE('',#37555,7.17);
#14510=CIRCLE('',#37558,7.17);
#14511=CIRCLE('',#37561,7.17);
#14512=CIRCLE('',#37564,7.17);
#14513=CIRCLE('',#37567,7.17);
#14514=CIRCLE('',#37570,7.17);
#14515=CIRCLE('',#37573,7.17);
#14516=CIRCLE('',#37576,7.17);
#14517=CIRCLE('',#37579,7.17);
#14518=CIRCLE('',#37581,7.17);
#14519=CIRCLE('',#37585,8.45882352941176);
#14520=CIRCLE('',#37586,9.38193994945664);
#14521=CIRCLE('',#37587,9.38193994945664);
#14522=CIRCLE('',#37588,9.38193994945664);
#14523=CIRCLE('',#37589,9.38193994945664);
#14524=CIRCLE('',#37590,9.38193994945664);
#14525=CIRCLE('',#37591,9.38193994945664);
#14526=CIRCLE('',#37599,7.1);
#14527=CIRCLE('',#37626,8.925);
#14528=CIRCLE('',#37633,6.4);
#14529=CIRCLE('',#37634,6.4);
#14530=CIRCLE('',#37636,7.2);
#14531=CIRCLE('',#37638,6.4);
#14532=VERTEX_POINT('',#47306);
#14533=VERTEX_POINT('',#47307);
#14534=VERTEX_POINT('',#47310);
#14535=VERTEX_POINT('',#47312);
#14536=VERTEX_POINT('',#47316);
#14537=VERTEX_POINT('',#47318);
#14538=VERTEX_POINT('',#47322);
#14539=VERTEX_POINT('',#47326);
#14540=VERTEX_POINT('',#47330);
#14541=VERTEX_POINT('',#47333);
#14542=VERTEX_POINT('',#47335);
#14543=VERTEX_POINT('',#47337);
#14544=VERTEX_POINT('',#47341);
#14545=VERTEX_POINT('',#47345);
#14546=VERTEX_POINT('',#47348);
#14547=VERTEX_POINT('',#47350);
#14548=VERTEX_POINT('',#47352);
#14549=VERTEX_POINT('',#47356);
#14550=VERTEX_POINT('',#47358);
#14551=VERTEX_POINT('',#47362);
#14552=VERTEX_POINT('',#47365);
#14553=VERTEX_POINT('',#47367);
#14554=VERTEX_POINT('',#47371);
#14555=VERTEX_POINT('',#47375);
#14556=VERTEX_POINT('',#47376);
#14557=VERTEX_POINT('',#47379);
#14558=VERTEX_POINT('',#47381);
#14559=VERTEX_POINT('',#47385);
#14560=VERTEX_POINT('',#47387);
#14561=VERTEX_POINT('',#47391);
#14562=VERTEX_POINT('',#47395);
#14563=VERTEX_POINT('',#47397);
#14564=VERTEX_POINT('',#47401);
#14565=VERTEX_POINT('',#47403);
#14566=VERTEX_POINT('',#47407);
#14567=VERTEX_POINT('',#47409);
#14568=VERTEX_POINT('',#47413);
#14569=VERTEX_POINT('',#47415);
#14570=VERTEX_POINT('',#47419);
#14571=VERTEX_POINT('',#47421);
#14572=VERTEX_POINT('',#47425);
#14573=VERTEX_POINT('',#47427);
#14574=VERTEX_POINT('',#47429);
#14575=VERTEX_POINT('',#47431);
#14576=VERTEX_POINT('',#47433);
#14577=VERTEX_POINT('',#47435);
#14578=VERTEX_POINT('',#47437);
#14579=VERTEX_POINT('',#47440);
#14580=VERTEX_POINT('',#47442);
#14581=VERTEX_POINT('',#47444);
#14582=VERTEX_POINT('',#47446);
#14583=VERTEX_POINT('',#47449);
#14584=VERTEX_POINT('',#47450);
#14585=VERTEX_POINT('',#47452);
#14586=VERTEX_POINT('',#47454);
#14587=VERTEX_POINT('',#47456);
#14588=VERTEX_POINT('',#47458);
#14589=VERTEX_POINT('',#47460);
#14590=VERTEX_POINT('',#47462);
#14591=VERTEX_POINT('',#47465);
#14592=VERTEX_POINT('',#47466);
#14593=VERTEX_POINT('',#47468);
#14594=VERTEX_POINT('',#47470);
#14595=VERTEX_POINT('',#47472);
#14596=VERTEX_POINT('',#47474);
#14597=VERTEX_POINT('',#47476);
#14598=VERTEX_POINT('',#47478);
#14599=VERTEX_POINT('',#47481);
#14600=VERTEX_POINT('',#47482);
#14601=VERTEX_POINT('',#47484);
#14602=VERTEX_POINT('',#47486);
#14603=VERTEX_POINT('',#47488);
#14604=VERTEX_POINT('',#47490);
#14605=VERTEX_POINT('',#47492);
#14606=VERTEX_POINT('',#47494);
#14607=VERTEX_POINT('',#47497);
#14608=VERTEX_POINT('',#47498);
#14609=VERTEX_POINT('',#47500);
#14610=VERTEX_POINT('',#47502);
#14611=VERTEX_POINT('',#47504);
#14612=VERTEX_POINT('',#47506);
#14613=VERTEX_POINT('',#47508);
#14614=VERTEX_POINT('',#47510);
#14615=VERTEX_POINT('',#47513);
#14616=VERTEX_POINT('',#47514);
#14617=VERTEX_POINT('',#47516);
#14618=VERTEX_POINT('',#47518);
#14619=VERTEX_POINT('',#47520);
#14620=VERTEX_POINT('',#47522);
#14621=VERTEX_POINT('',#47524);
#14622=VERTEX_POINT('',#47526);
#14623=VERTEX_POINT('',#47529);
#14624=VERTEX_POINT('',#47530);
#14625=VERTEX_POINT('',#47532);
#14626=VERTEX_POINT('',#47534);
#14627=VERTEX_POINT('',#47536);
#14628=VERTEX_POINT('',#47538);
#14629=VERTEX_POINT('',#47540);
#14630=VERTEX_POINT('',#47542);
#14631=VERTEX_POINT('',#47545);
#14632=VERTEX_POINT('',#47546);
#14633=VERTEX_POINT('',#47548);
#14634=VERTEX_POINT('',#47550);
#14635=VERTEX_POINT('',#47552);
#14636=VERTEX_POINT('',#47554);
#14637=VERTEX_POINT('',#47556);
#14638=VERTEX_POINT('',#47558);
#14639=VERTEX_POINT('',#47561);
#14640=VERTEX_POINT('',#47562);
#14641=VERTEX_POINT('',#47564);
#14642=VERTEX_POINT('',#47566);
#14643=VERTEX_POINT('',#47568);
#14644=VERTEX_POINT('',#47570);
#14645=VERTEX_POINT('',#47572);
#14646=VERTEX_POINT('',#47574);
#14647=VERTEX_POINT('',#47577);
#14648=VERTEX_POINT('',#47578);
#14649=VERTEX_POINT('',#47580);
#14650=VERTEX_POINT('',#47582);
#14651=VERTEX_POINT('',#47584);
#14652=VERTEX_POINT('',#47586);
#14653=VERTEX_POINT('',#47588);
#14654=VERTEX_POINT('',#47590);
#14655=VERTEX_POINT('',#47593);
#14656=VERTEX_POINT('',#47594);
#14657=VERTEX_POINT('',#47596);
#14658=VERTEX_POINT('',#47598);
#14659=VERTEX_POINT('',#47600);
#14660=VERTEX_POINT('',#47602);
#14661=VERTEX_POINT('',#47604);
#14662=VERTEX_POINT('',#47606);
#14663=VERTEX_POINT('',#47609);
#14664=VERTEX_POINT('',#47610);
#14665=VERTEX_POINT('',#47612);
#14666=VERTEX_POINT('',#47614);
#14667=VERTEX_POINT('',#47616);
#14668=VERTEX_POINT('',#47618);
#14669=VERTEX_POINT('',#47620);
#14670=VERTEX_POINT('',#47622);
#14671=VERTEX_POINT('',#47625);
#14672=VERTEX_POINT('',#47626);
#14673=VERTEX_POINT('',#47628);
#14674=VERTEX_POINT('',#47630);
#14675=VERTEX_POINT('',#47632);
#14676=VERTEX_POINT('',#47634);
#14677=VERTEX_POINT('',#47636);
#14678=VERTEX_POINT('',#47638);
#14679=VERTEX_POINT('',#47641);
#14680=VERTEX_POINT('',#47642);
#14681=VERTEX_POINT('',#47644);
#14682=VERTEX_POINT('',#47646);
#14683=VERTEX_POINT('',#47648);
#14684=VERTEX_POINT('',#47650);
#14685=VERTEX_POINT('',#47652);
#14686=VERTEX_POINT('',#47654);
#14687=VERTEX_POINT('',#47657);
#14688=VERTEX_POINT('',#47658);
#14689=VERTEX_POINT('',#47660);
#14690=VERTEX_POINT('',#47662);
#14691=VERTEX_POINT('',#47664);
#14692=VERTEX_POINT('',#47666);
#14693=VERTEX_POINT('',#47668);
#14694=VERTEX_POINT('',#47670);
#14695=VERTEX_POINT('',#47673);
#14696=VERTEX_POINT('',#47674);
#14697=VERTEX_POINT('',#47676);
#14698=VERTEX_POINT('',#47678);
#14699=VERTEX_POINT('',#47680);
#14700=VERTEX_POINT('',#47682);
#14701=VERTEX_POINT('',#47684);
#14702=VERTEX_POINT('',#47686);
#14703=VERTEX_POINT('',#47689);
#14704=VERTEX_POINT('',#47690);
#14705=VERTEX_POINT('',#47692);
#14706=VERTEX_POINT('',#47694);
#14707=VERTEX_POINT('',#47696);
#14708=VERTEX_POINT('',#47698);
#14709=VERTEX_POINT('',#47700);
#14710=VERTEX_POINT('',#47702);
#14711=VERTEX_POINT('',#47705);
#14712=VERTEX_POINT('',#47706);
#14713=VERTEX_POINT('',#47708);
#14714=VERTEX_POINT('',#47710);
#14715=VERTEX_POINT('',#47712);
#14716=VERTEX_POINT('',#47714);
#14717=VERTEX_POINT('',#47716);
#14718=VERTEX_POINT('',#47718);
#14719=VERTEX_POINT('',#47721);
#14720=VERTEX_POINT('',#47722);
#14721=VERTEX_POINT('',#47724);
#14722=VERTEX_POINT('',#47726);
#14723=VERTEX_POINT('',#47728);
#14724=VERTEX_POINT('',#47730);
#14725=VERTEX_POINT('',#47732);
#14726=VERTEX_POINT('',#47734);
#14727=VERTEX_POINT('',#47737);
#14728=VERTEX_POINT('',#47738);
#14729=VERTEX_POINT('',#47740);
#14730=VERTEX_POINT('',#47742);
#14731=VERTEX_POINT('',#47744);
#14732=VERTEX_POINT('',#47746);
#14733=VERTEX_POINT('',#47748);
#14734=VERTEX_POINT('',#47750);
#14735=VERTEX_POINT('',#47753);
#14736=VERTEX_POINT('',#47754);
#14737=VERTEX_POINT('',#47756);
#14738=VERTEX_POINT('',#47758);
#14739=VERTEX_POINT('',#47760);
#14740=VERTEX_POINT('',#47762);
#14741=VERTEX_POINT('',#47764);
#14742=VERTEX_POINT('',#47766);
#14743=VERTEX_POINT('',#47769);
#14744=VERTEX_POINT('',#47770);
#14745=VERTEX_POINT('',#47772);
#14746=VERTEX_POINT('',#47774);
#14747=VERTEX_POINT('',#47776);
#14748=VERTEX_POINT('',#47778);
#14749=VERTEX_POINT('',#47780);
#14750=VERTEX_POINT('',#47782);
#14751=VERTEX_POINT('',#47785);
#14752=VERTEX_POINT('',#47786);
#14753=VERTEX_POINT('',#47788);
#14754=VERTEX_POINT('',#47790);
#14755=VERTEX_POINT('',#47792);
#14756=VERTEX_POINT('',#47794);
#14757=VERTEX_POINT('',#47796);
#14758=VERTEX_POINT('',#47798);
#14759=VERTEX_POINT('',#47801);
#14760=VERTEX_POINT('',#47802);
#14761=VERTEX_POINT('',#47804);
#14762=VERTEX_POINT('',#47806);
#14763=VERTEX_POINT('',#47808);
#14764=VERTEX_POINT('',#47810);
#14765=VERTEX_POINT('',#47812);
#14766=VERTEX_POINT('',#47814);
#14767=VERTEX_POINT('',#47817);
#14768=VERTEX_POINT('',#47818);
#14769=VERTEX_POINT('',#47820);
#14770=VERTEX_POINT('',#47822);
#14771=VERTEX_POINT('',#47824);
#14772=VERTEX_POINT('',#47826);
#14773=VERTEX_POINT('',#47828);
#14774=VERTEX_POINT('',#47830);
#14775=VERTEX_POINT('',#47833);
#14776=VERTEX_POINT('',#47834);
#14777=VERTEX_POINT('',#47836);
#14778=VERTEX_POINT('',#47838);
#14779=VERTEX_POINT('',#47840);
#14780=VERTEX_POINT('',#47842);
#14781=VERTEX_POINT('',#47844);
#14782=VERTEX_POINT('',#47846);
#14783=VERTEX_POINT('',#47849);
#14784=VERTEX_POINT('',#47850);
#14785=VERTEX_POINT('',#47852);
#14786=VERTEX_POINT('',#47854);
#14787=VERTEX_POINT('',#47856);
#14788=VERTEX_POINT('',#47858);
#14789=VERTEX_POINT('',#47860);
#14790=VERTEX_POINT('',#47862);
#14791=VERTEX_POINT('',#47865);
#14792=VERTEX_POINT('',#47866);
#14793=VERTEX_POINT('',#47868);
#14794=VERTEX_POINT('',#47870);
#14795=VERTEX_POINT('',#47872);
#14796=VERTEX_POINT('',#47874);
#14797=VERTEX_POINT('',#47876);
#14798=VERTEX_POINT('',#47878);
#14799=VERTEX_POINT('',#47881);
#14800=VERTEX_POINT('',#47882);
#14801=VERTEX_POINT('',#47884);
#14802=VERTEX_POINT('',#47886);
#14803=VERTEX_POINT('',#47888);
#14804=VERTEX_POINT('',#47890);
#14805=VERTEX_POINT('',#47892);
#14806=VERTEX_POINT('',#47894);
#14807=VERTEX_POINT('',#47897);
#14808=VERTEX_POINT('',#47898);
#14809=VERTEX_POINT('',#47900);
#14810=VERTEX_POINT('',#47902);
#14811=VERTEX_POINT('',#47904);
#14812=VERTEX_POINT('',#47906);
#14813=VERTEX_POINT('',#47908);
#14814=VERTEX_POINT('',#47910);
#14815=VERTEX_POINT('',#47913);
#14816=VERTEX_POINT('',#47914);
#14817=VERTEX_POINT('',#47916);
#14818=VERTEX_POINT('',#47918);
#14819=VERTEX_POINT('',#47920);
#14820=VERTEX_POINT('',#47922);
#14821=VERTEX_POINT('',#47924);
#14822=VERTEX_POINT('',#47926);
#14823=VERTEX_POINT('',#47929);
#14824=VERTEX_POINT('',#47930);
#14825=VERTEX_POINT('',#47932);
#14826=VERTEX_POINT('',#47934);
#14827=VERTEX_POINT('',#47936);
#14828=VERTEX_POINT('',#47938);
#14829=VERTEX_POINT('',#47940);
#14830=VERTEX_POINT('',#47942);
#14831=VERTEX_POINT('',#47945);
#14832=VERTEX_POINT('',#47946);
#14833=VERTEX_POINT('',#47948);
#14834=VERTEX_POINT('',#47950);
#14835=VERTEX_POINT('',#47952);
#14836=VERTEX_POINT('',#47954);
#14837=VERTEX_POINT('',#47956);
#14838=VERTEX_POINT('',#47958);
#14839=VERTEX_POINT('',#47961);
#14840=VERTEX_POINT('',#47962);
#14841=VERTEX_POINT('',#47964);
#14842=VERTEX_POINT('',#47966);
#14843=VERTEX_POINT('',#47968);
#14844=VERTEX_POINT('',#47970);
#14845=VERTEX_POINT('',#47972);
#14846=VERTEX_POINT('',#47974);
#14847=VERTEX_POINT('',#47977);
#14848=VERTEX_POINT('',#47978);
#14849=VERTEX_POINT('',#47980);
#14850=VERTEX_POINT('',#47982);
#14851=VERTEX_POINT('',#47984);
#14852=VERTEX_POINT('',#47986);
#14853=VERTEX_POINT('',#47988);
#14854=VERTEX_POINT('',#47990);
#14855=VERTEX_POINT('',#47993);
#14856=VERTEX_POINT('',#47994);
#14857=VERTEX_POINT('',#47996);
#14858=VERTEX_POINT('',#47998);
#14859=VERTEX_POINT('',#48000);
#14860=VERTEX_POINT('',#48002);
#14861=VERTEX_POINT('',#48004);
#14862=VERTEX_POINT('',#48006);
#14863=VERTEX_POINT('',#48009);
#14864=VERTEX_POINT('',#48010);
#14865=VERTEX_POINT('',#48012);
#14866=VERTEX_POINT('',#48014);
#14867=VERTEX_POINT('',#48016);
#14868=VERTEX_POINT('',#48018);
#14869=VERTEX_POINT('',#48020);
#14870=VERTEX_POINT('',#48022);
#14871=VERTEX_POINT('',#48025);
#14872=VERTEX_POINT('',#48026);
#14873=VERTEX_POINT('',#48028);
#14874=VERTEX_POINT('',#48030);
#14875=VERTEX_POINT('',#48032);
#14876=VERTEX_POINT('',#48034);
#14877=VERTEX_POINT('',#48036);
#14878=VERTEX_POINT('',#48038);
#14879=VERTEX_POINT('',#48041);
#14880=VERTEX_POINT('',#48042);
#14881=VERTEX_POINT('',#48044);
#14882=VERTEX_POINT('',#48046);
#14883=VERTEX_POINT('',#48048);
#14884=VERTEX_POINT('',#48050);
#14885=VERTEX_POINT('',#48052);
#14886=VERTEX_POINT('',#48054);
#14887=VERTEX_POINT('',#48057);
#14888=VERTEX_POINT('',#48058);
#14889=VERTEX_POINT('',#48060);
#14890=VERTEX_POINT('',#48062);
#14891=VERTEX_POINT('',#48064);
#14892=VERTEX_POINT('',#48066);
#14893=VERTEX_POINT('',#48068);
#14894=VERTEX_POINT('',#48070);
#14895=VERTEX_POINT('',#48073);
#14896=VERTEX_POINT('',#48074);
#14897=VERTEX_POINT('',#48076);
#14898=VERTEX_POINT('',#48078);
#14899=VERTEX_POINT('',#48080);
#14900=VERTEX_POINT('',#48082);
#14901=VERTEX_POINT('',#48084);
#14902=VERTEX_POINT('',#48086);
#14903=VERTEX_POINT('',#48089);
#14904=VERTEX_POINT('',#48090);
#14905=VERTEX_POINT('',#48092);
#14906=VERTEX_POINT('',#48094);
#14907=VERTEX_POINT('',#48096);
#14908=VERTEX_POINT('',#48098);
#14909=VERTEX_POINT('',#48100);
#14910=VERTEX_POINT('',#48102);
#14911=VERTEX_POINT('',#48105);
#14912=VERTEX_POINT('',#48106);
#14913=VERTEX_POINT('',#48108);
#14914=VERTEX_POINT('',#48110);
#14915=VERTEX_POINT('',#48112);
#14916=VERTEX_POINT('',#48114);
#14917=VERTEX_POINT('',#48116);
#14918=VERTEX_POINT('',#48118);
#14919=VERTEX_POINT('',#48121);
#14920=VERTEX_POINT('',#48122);
#14921=VERTEX_POINT('',#48124);
#14922=VERTEX_POINT('',#48126);
#14923=VERTEX_POINT('',#48128);
#14924=VERTEX_POINT('',#48130);
#14925=VERTEX_POINT('',#48132);
#14926=VERTEX_POINT('',#48134);
#14927=VERTEX_POINT('',#48137);
#14928=VERTEX_POINT('',#48138);
#14929=VERTEX_POINT('',#48140);
#14930=VERTEX_POINT('',#48142);
#14931=VERTEX_POINT('',#48144);
#14932=VERTEX_POINT('',#48146);
#14933=VERTEX_POINT('',#48148);
#14934=VERTEX_POINT('',#48150);
#14935=VERTEX_POINT('',#48153);
#14936=VERTEX_POINT('',#48154);
#14937=VERTEX_POINT('',#48156);
#14938=VERTEX_POINT('',#48158);
#14939=VERTEX_POINT('',#48160);
#14940=VERTEX_POINT('',#48162);
#14941=VERTEX_POINT('',#48164);
#14942=VERTEX_POINT('',#48166);
#14943=VERTEX_POINT('',#48169);
#14944=VERTEX_POINT('',#48170);
#14945=VERTEX_POINT('',#48172);
#14946=VERTEX_POINT('',#48174);
#14947=VERTEX_POINT('',#48176);
#14948=VERTEX_POINT('',#48178);
#14949=VERTEX_POINT('',#48180);
#14950=VERTEX_POINT('',#48182);
#14951=VERTEX_POINT('',#48185);
#14952=VERTEX_POINT('',#48186);
#14953=VERTEX_POINT('',#48188);
#14954=VERTEX_POINT('',#48190);
#14955=VERTEX_POINT('',#48192);
#14956=VERTEX_POINT('',#48194);
#14957=VERTEX_POINT('',#48196);
#14958=VERTEX_POINT('',#48198);
#14959=VERTEX_POINT('',#48201);
#14960=VERTEX_POINT('',#48202);
#14961=VERTEX_POINT('',#48204);
#14962=VERTEX_POINT('',#48206);
#14963=VERTEX_POINT('',#48208);
#14964=VERTEX_POINT('',#48210);
#14965=VERTEX_POINT('',#48212);
#14966=VERTEX_POINT('',#48214);
#14967=VERTEX_POINT('',#48217);
#14968=VERTEX_POINT('',#48218);
#14969=VERTEX_POINT('',#48220);
#14970=VERTEX_POINT('',#48222);
#14971=VERTEX_POINT('',#48224);
#14972=VERTEX_POINT('',#48226);
#14973=VERTEX_POINT('',#48228);
#14974=VERTEX_POINT('',#48230);
#14975=VERTEX_POINT('',#48233);
#14976=VERTEX_POINT('',#48234);
#14977=VERTEX_POINT('',#48236);
#14978=VERTEX_POINT('',#48238);
#14979=VERTEX_POINT('',#48240);
#14980=VERTEX_POINT('',#48242);
#14981=VERTEX_POINT('',#48244);
#14982=VERTEX_POINT('',#48246);
#14983=VERTEX_POINT('',#48249);
#14984=VERTEX_POINT('',#48250);
#14985=VERTEX_POINT('',#48252);
#14986=VERTEX_POINT('',#48254);
#14987=VERTEX_POINT('',#48256);
#14988=VERTEX_POINT('',#48258);
#14989=VERTEX_POINT('',#48260);
#14990=VERTEX_POINT('',#48262);
#14991=VERTEX_POINT('',#48265);
#14992=VERTEX_POINT('',#48266);
#14993=VERTEX_POINT('',#48268);
#14994=VERTEX_POINT('',#48270);
#14995=VERTEX_POINT('',#48272);
#14996=VERTEX_POINT('',#48274);
#14997=VERTEX_POINT('',#48276);
#14998=VERTEX_POINT('',#48278);
#14999=VERTEX_POINT('',#48281);
#15000=VERTEX_POINT('',#48282);
#15001=VERTEX_POINT('',#48284);
#15002=VERTEX_POINT('',#48286);
#15003=VERTEX_POINT('',#48288);
#15004=VERTEX_POINT('',#48290);
#15005=VERTEX_POINT('',#48292);
#15006=VERTEX_POINT('',#48294);
#15007=VERTEX_POINT('',#48297);
#15008=VERTEX_POINT('',#48298);
#15009=VERTEX_POINT('',#48300);
#15010=VERTEX_POINT('',#48302);
#15011=VERTEX_POINT('',#48304);
#15012=VERTEX_POINT('',#48306);
#15013=VERTEX_POINT('',#48308);
#15014=VERTEX_POINT('',#48310);
#15015=VERTEX_POINT('',#48313);
#15016=VERTEX_POINT('',#48314);
#15017=VERTEX_POINT('',#48316);
#15018=VERTEX_POINT('',#48318);
#15019=VERTEX_POINT('',#48320);
#15020=VERTEX_POINT('',#48322);
#15021=VERTEX_POINT('',#48324);
#15022=VERTEX_POINT('',#48326);
#15023=VERTEX_POINT('',#48329);
#15024=VERTEX_POINT('',#48330);
#15025=VERTEX_POINT('',#48332);
#15026=VERTEX_POINT('',#48334);
#15027=VERTEX_POINT('',#48336);
#15028=VERTEX_POINT('',#48338);
#15029=VERTEX_POINT('',#48340);
#15030=VERTEX_POINT('',#48342);
#15031=VERTEX_POINT('',#48345);
#15032=VERTEX_POINT('',#48346);
#15033=VERTEX_POINT('',#48348);
#15034=VERTEX_POINT('',#48350);
#15035=VERTEX_POINT('',#48352);
#15036=VERTEX_POINT('',#48354);
#15037=VERTEX_POINT('',#48356);
#15038=VERTEX_POINT('',#48358);
#15039=VERTEX_POINT('',#48361);
#15040=VERTEX_POINT('',#48362);
#15041=VERTEX_POINT('',#48364);
#15042=VERTEX_POINT('',#48366);
#15043=VERTEX_POINT('',#48368);
#15044=VERTEX_POINT('',#48370);
#15045=VERTEX_POINT('',#48372);
#15046=VERTEX_POINT('',#48374);
#15047=VERTEX_POINT('',#48377);
#15048=VERTEX_POINT('',#48378);
#15049=VERTEX_POINT('',#48380);
#15050=VERTEX_POINT('',#48382);
#15051=VERTEX_POINT('',#48384);
#15052=VERTEX_POINT('',#48386);
#15053=VERTEX_POINT('',#48388);
#15054=VERTEX_POINT('',#48390);
#15055=VERTEX_POINT('',#48393);
#15056=VERTEX_POINT('',#48394);
#15057=VERTEX_POINT('',#48396);
#15058=VERTEX_POINT('',#48398);
#15059=VERTEX_POINT('',#48400);
#15060=VERTEX_POINT('',#48402);
#15061=VERTEX_POINT('',#48404);
#15062=VERTEX_POINT('',#48406);
#15063=VERTEX_POINT('',#48409);
#15064=VERTEX_POINT('',#48410);
#15065=VERTEX_POINT('',#48412);
#15066=VERTEX_POINT('',#48414);
#15067=VERTEX_POINT('',#48416);
#15068=VERTEX_POINT('',#48418);
#15069=VERTEX_POINT('',#48420);
#15070=VERTEX_POINT('',#48422);
#15071=VERTEX_POINT('',#48425);
#15072=VERTEX_POINT('',#48426);
#15073=VERTEX_POINT('',#48428);
#15074=VERTEX_POINT('',#48430);
#15075=VERTEX_POINT('',#48432);
#15076=VERTEX_POINT('',#48434);
#15077=VERTEX_POINT('',#48436);
#15078=VERTEX_POINT('',#48438);
#15079=VERTEX_POINT('',#48441);
#15080=VERTEX_POINT('',#48442);
#15081=VERTEX_POINT('',#48444);
#15082=VERTEX_POINT('',#48446);
#15083=VERTEX_POINT('',#48448);
#15084=VERTEX_POINT('',#48450);
#15085=VERTEX_POINT('',#48452);
#15086=VERTEX_POINT('',#48454);
#15087=VERTEX_POINT('',#48457);
#15088=VERTEX_POINT('',#48458);
#15089=VERTEX_POINT('',#48460);
#15090=VERTEX_POINT('',#48462);
#15091=VERTEX_POINT('',#48464);
#15092=VERTEX_POINT('',#48466);
#15093=VERTEX_POINT('',#48468);
#15094=VERTEX_POINT('',#48470);
#15095=VERTEX_POINT('',#48473);
#15096=VERTEX_POINT('',#48474);
#15097=VERTEX_POINT('',#48476);
#15098=VERTEX_POINT('',#48478);
#15099=VERTEX_POINT('',#48480);
#15100=VERTEX_POINT('',#48482);
#15101=VERTEX_POINT('',#48484);
#15102=VERTEX_POINT('',#48486);
#15103=VERTEX_POINT('',#48489);
#15104=VERTEX_POINT('',#48490);
#15105=VERTEX_POINT('',#48492);
#15106=VERTEX_POINT('',#48494);
#15107=VERTEX_POINT('',#48496);
#15108=VERTEX_POINT('',#48498);
#15109=VERTEX_POINT('',#48500);
#15110=VERTEX_POINT('',#48502);
#15111=VERTEX_POINT('',#48505);
#15112=VERTEX_POINT('',#48506);
#15113=VERTEX_POINT('',#48508);
#15114=VERTEX_POINT('',#48510);
#15115=VERTEX_POINT('',#48512);
#15116=VERTEX_POINT('',#48514);
#15117=VERTEX_POINT('',#48516);
#15118=VERTEX_POINT('',#48518);
#15119=VERTEX_POINT('',#48521);
#15120=VERTEX_POINT('',#48522);
#15121=VERTEX_POINT('',#48524);
#15122=VERTEX_POINT('',#48526);
#15123=VERTEX_POINT('',#48528);
#15124=VERTEX_POINT('',#48530);
#15125=VERTEX_POINT('',#48532);
#15126=VERTEX_POINT('',#48534);
#15127=VERTEX_POINT('',#48537);
#15128=VERTEX_POINT('',#48538);
#15129=VERTEX_POINT('',#48540);
#15130=VERTEX_POINT('',#48542);
#15131=VERTEX_POINT('',#48544);
#15132=VERTEX_POINT('',#48546);
#15133=VERTEX_POINT('',#48548);
#15134=VERTEX_POINT('',#48550);
#15135=VERTEX_POINT('',#48553);
#15136=VERTEX_POINT('',#48554);
#15137=VERTEX_POINT('',#48556);
#15138=VERTEX_POINT('',#48558);
#15139=VERTEX_POINT('',#48560);
#15140=VERTEX_POINT('',#48562);
#15141=VERTEX_POINT('',#48564);
#15142=VERTEX_POINT('',#48566);
#15143=VERTEX_POINT('',#48569);
#15144=VERTEX_POINT('',#48570);
#15145=VERTEX_POINT('',#48572);
#15146=VERTEX_POINT('',#48574);
#15147=VERTEX_POINT('',#48576);
#15148=VERTEX_POINT('',#48578);
#15149=VERTEX_POINT('',#48580);
#15150=VERTEX_POINT('',#48582);
#15151=VERTEX_POINT('',#48586);
#15152=VERTEX_POINT('',#48587);
#15153=VERTEX_POINT('',#48589);
#15154=VERTEX_POINT('',#48594);
#15155=VERTEX_POINT('',#48601);
#15156=VERTEX_POINT('',#48603);
#15157=VERTEX_POINT('',#48610);
#15158=VERTEX_POINT('',#48612);
#15159=VERTEX_POINT('',#48619);
#15160=VERTEX_POINT('',#48621);
#15161=VERTEX_POINT('',#48628);
#15162=VERTEX_POINT('',#48630);
#15163=VERTEX_POINT('',#48637);
#15164=VERTEX_POINT('',#48639);
#15165=VERTEX_POINT('',#48646);
#15166=VERTEX_POINT('',#48648);
#15167=VERTEX_POINT('',#48655);
#15168=VERTEX_POINT('',#48657);
#15169=VERTEX_POINT('',#48664);
#15170=VERTEX_POINT('',#48666);
#15171=VERTEX_POINT('',#48676);
#15172=VERTEX_POINT('',#48678);
#15173=VERTEX_POINT('',#48682);
#15174=VERTEX_POINT('',#48686);
#15175=VERTEX_POINT('',#48690);
#15176=VERTEX_POINT('',#48694);
#15177=VERTEX_POINT('',#48698);
#15178=VERTEX_POINT('',#48702);
#15179=VERTEX_POINT('',#48704);
#15180=VERTEX_POINT('',#48706);
#15181=VERTEX_POINT('',#48708);
#15182=VERTEX_POINT('',#48710);
#15183=VERTEX_POINT('',#48713);
#15184=VERTEX_POINT('',#48714);
#15185=VERTEX_POINT('',#48717);
#15186=VERTEX_POINT('',#48721);
#15187=VERTEX_POINT('',#48725);
#15188=VERTEX_POINT('',#48727);
#15189=VERTEX_POINT('',#48731);
#15190=VERTEX_POINT('',#48733);
#15191=VERTEX_POINT('',#48737);
#15192=VERTEX_POINT('',#48741);
#15193=VERTEX_POINT('',#48748);
#15194=VERTEX_POINT('',#48749);
#15195=VERTEX_POINT('',#48751);
#15196=VERTEX_POINT('',#48768);
#15197=VERTEX_POINT('',#48769);
#15198=VERTEX_POINT('',#48771);
#15199=VERTEX_POINT('',#48775);
#15200=VERTEX_POINT('',#48776);
#15201=VERTEX_POINT('',#48778);
#15202=VERTEX_POINT('',#48782);
#15203=VERTEX_POINT('',#48783);
#15204=VERTEX_POINT('',#48785);
#15205=VERTEX_POINT('',#48792);
#15206=VERTEX_POINT('',#48793);
#15207=VERTEX_POINT('',#48795);
#15208=VERTEX_POINT('',#48823);
#15209=VERTEX_POINT('',#48824);
#15210=VERTEX_POINT('',#48826);
#15211=VERTEX_POINT('',#48830);
#15212=VERTEX_POINT('',#48831);
#15213=VERTEX_POINT('',#48834);
#15214=VERTEX_POINT('',#48841);
#15215=VERTEX_POINT('',#48842);
#15216=VERTEX_POINT('',#48844);
#15217=VERTEX_POINT('',#48848);
#15218=VERTEX_POINT('',#48849);
#15219=VERTEX_POINT('',#48852);
#15220=VERTEX_POINT('',#48862);
#15221=VERTEX_POINT('',#48869);
#15222=VERTEX_POINT('',#48878);
#15223=VERTEX_POINT('',#48879);
#15224=VERTEX_POINT('',#48881);
#15225=VERTEX_POINT('',#48885);
#15226=VERTEX_POINT('',#48886);
#15227=VERTEX_POINT('',#48888);
#15228=VERTEX_POINT('',#48892);
#15229=VERTEX_POINT('',#48893);
#15230=VERTEX_POINT('',#48895);
#15231=VERTEX_POINT('',#48902);
#15232=VERTEX_POINT('',#48903);
#15233=VERTEX_POINT('',#48905);
#15234=VERTEX_POINT('',#48933);
#15235=VERTEX_POINT('',#48934);
#15236=VERTEX_POINT('',#48936);
#15237=VERTEX_POINT('',#48940);
#15238=VERTEX_POINT('',#48941);
#15239=VERTEX_POINT('',#48943);
#15240=VERTEX_POINT('',#48947);
#15241=VERTEX_POINT('',#48948);
#15242=VERTEX_POINT('',#48950);
#15243=VERTEX_POINT('',#48957);
#15244=VERTEX_POINT('',#48958);
#15245=VERTEX_POINT('',#48960);
#15246=VERTEX_POINT('',#48988);
#15247=VERTEX_POINT('',#48989);
#15248=VERTEX_POINT('',#48992);
#15249=VERTEX_POINT('',#48996);
#15250=VERTEX_POINT('',#49000);
#15251=VERTEX_POINT('',#49002);
#15252=VERTEX_POINT('',#49006);
#15253=VERTEX_POINT('',#49008);
#15254=VERTEX_POINT('',#49012);
#15255=VERTEX_POINT('',#49016);
#15256=VERTEX_POINT('',#49023);
#15257=VERTEX_POINT('',#49024);
#15258=VERTEX_POINT('',#49026);
#15259=VERTEX_POINT('',#49043);
#15260=VERTEX_POINT('',#49044);
#15261=VERTEX_POINT('',#49046);
#15262=VERTEX_POINT('',#49050);
#15263=VERTEX_POINT('',#49051);
#15264=VERTEX_POINT('',#49053);
#15265=VERTEX_POINT('',#49057);
#15266=VERTEX_POINT('',#49058);
#15267=VERTEX_POINT('',#49060);
#15268=VERTEX_POINT('',#49067);
#15269=VERTEX_POINT('',#49068);
#15270=VERTEX_POINT('',#49070);
#15271=VERTEX_POINT('',#49098);
#15272=VERTEX_POINT('',#49099);
#15273=VERTEX_POINT('',#49101);
#15274=VERTEX_POINT('',#49105);
#15275=VERTEX_POINT('',#49106);
#15276=VERTEX_POINT('',#49109);
#15277=VERTEX_POINT('',#49116);
#15278=VERTEX_POINT('',#49117);
#15279=VERTEX_POINT('',#49119);
#15280=VERTEX_POINT('',#49123);
#15281=VERTEX_POINT('',#49124);
#15282=VERTEX_POINT('',#49127);
#15283=VERTEX_POINT('',#49137);
#15284=VERTEX_POINT('',#49144);
#15285=VERTEX_POINT('',#49153);
#15286=VERTEX_POINT('',#49154);
#15287=VERTEX_POINT('',#49156);
#15288=VERTEX_POINT('',#49160);
#15289=VERTEX_POINT('',#49161);
#15290=VERTEX_POINT('',#49163);
#15291=VERTEX_POINT('',#49167);
#15292=VERTEX_POINT('',#49168);
#15293=VERTEX_POINT('',#49170);
#15294=VERTEX_POINT('',#49177);
#15295=VERTEX_POINT('',#49178);
#15296=VERTEX_POINT('',#49180);
#15297=VERTEX_POINT('',#49208);
#15298=VERTEX_POINT('',#49209);
#15299=VERTEX_POINT('',#49211);
#15300=VERTEX_POINT('',#49215);
#15301=VERTEX_POINT('',#49216);
#15302=VERTEX_POINT('',#49218);
#15303=VERTEX_POINT('',#49222);
#15304=VERTEX_POINT('',#49223);
#15305=VERTEX_POINT('',#49225);
#15306=VERTEX_POINT('',#49232);
#15307=VERTEX_POINT('',#49233);
#15308=VERTEX_POINT('',#49235);
#15309=VERTEX_POINT('',#49263);
#15310=VERTEX_POINT('',#49264);
#15311=VERTEX_POINT('',#49267);
#15312=VERTEX_POINT('',#49271);
#15313=VERTEX_POINT('',#49275);
#15314=VERTEX_POINT('',#49277);
#15315=VERTEX_POINT('',#49281);
#15316=VERTEX_POINT('',#49283);
#15317=VERTEX_POINT('',#49287);
#15318=VERTEX_POINT('',#49291);
#15319=VERTEX_POINT('',#49298);
#15320=VERTEX_POINT('',#49299);
#15321=VERTEX_POINT('',#49301);
#15322=VERTEX_POINT('',#49318);
#15323=VERTEX_POINT('',#49319);
#15324=VERTEX_POINT('',#49321);
#15325=VERTEX_POINT('',#49325);
#15326=VERTEX_POINT('',#49326);
#15327=VERTEX_POINT('',#49328);
#15328=VERTEX_POINT('',#49332);
#15329=VERTEX_POINT('',#49333);
#15330=VERTEX_POINT('',#49335);
#15331=VERTEX_POINT('',#49342);
#15332=VERTEX_POINT('',#49343);
#15333=VERTEX_POINT('',#49345);
#15334=VERTEX_POINT('',#49373);
#15335=VERTEX_POINT('',#49374);
#15336=VERTEX_POINT('',#49376);
#15337=VERTEX_POINT('',#49380);
#15338=VERTEX_POINT('',#49381);
#15339=VERTEX_POINT('',#49384);
#15340=VERTEX_POINT('',#49391);
#15341=VERTEX_POINT('',#49392);
#15342=VERTEX_POINT('',#49394);
#15343=VERTEX_POINT('',#49398);
#15344=VERTEX_POINT('',#49399);
#15345=VERTEX_POINT('',#49402);
#15346=VERTEX_POINT('',#49412);
#15347=VERTEX_POINT('',#49419);
#15348=VERTEX_POINT('',#49428);
#15349=VERTEX_POINT('',#49429);
#15350=VERTEX_POINT('',#49431);
#15351=VERTEX_POINT('',#49435);
#15352=VERTEX_POINT('',#49436);
#15353=VERTEX_POINT('',#49438);
#15354=VERTEX_POINT('',#49442);
#15355=VERTEX_POINT('',#49443);
#15356=VERTEX_POINT('',#49445);
#15357=VERTEX_POINT('',#49452);
#15358=VERTEX_POINT('',#49453);
#15359=VERTEX_POINT('',#49455);
#15360=VERTEX_POINT('',#49483);
#15361=VERTEX_POINT('',#49484);
#15362=VERTEX_POINT('',#49486);
#15363=VERTEX_POINT('',#49490);
#15364=VERTEX_POINT('',#49491);
#15365=VERTEX_POINT('',#49493);
#15366=VERTEX_POINT('',#49497);
#15367=VERTEX_POINT('',#49498);
#15368=VERTEX_POINT('',#49500);
#15369=VERTEX_POINT('',#49507);
#15370=VERTEX_POINT('',#49508);
#15371=VERTEX_POINT('',#49510);
#15372=VERTEX_POINT('',#49538);
#15373=VERTEX_POINT('',#49539);
#15374=VERTEX_POINT('',#49542);
#15375=VERTEX_POINT('',#49546);
#15376=VERTEX_POINT('',#49550);
#15377=VERTEX_POINT('',#49552);
#15378=VERTEX_POINT('',#49556);
#15379=VERTEX_POINT('',#49558);
#15380=VERTEX_POINT('',#49562);
#15381=VERTEX_POINT('',#49566);
#15382=VERTEX_POINT('',#49573);
#15383=VERTEX_POINT('',#49574);
#15384=VERTEX_POINT('',#49576);
#15385=VERTEX_POINT('',#49593);
#15386=VERTEX_POINT('',#49594);
#15387=VERTEX_POINT('',#49596);
#15388=VERTEX_POINT('',#49600);
#15389=VERTEX_POINT('',#49601);
#15390=VERTEX_POINT('',#49603);
#15391=VERTEX_POINT('',#49607);
#15392=VERTEX_POINT('',#49608);
#15393=VERTEX_POINT('',#49610);
#15394=VERTEX_POINT('',#49617);
#15395=VERTEX_POINT('',#49618);
#15396=VERTEX_POINT('',#49620);
#15397=VERTEX_POINT('',#49648);
#15398=VERTEX_POINT('',#49649);
#15399=VERTEX_POINT('',#49651);
#15400=VERTEX_POINT('',#49655);
#15401=VERTEX_POINT('',#49656);
#15402=VERTEX_POINT('',#49659);
#15403=VERTEX_POINT('',#49666);
#15404=VERTEX_POINT('',#49667);
#15405=VERTEX_POINT('',#49669);
#15406=VERTEX_POINT('',#49673);
#15407=VERTEX_POINT('',#49674);
#15408=VERTEX_POINT('',#49677);
#15409=VERTEX_POINT('',#49687);
#15410=VERTEX_POINT('',#49694);
#15411=VERTEX_POINT('',#49703);
#15412=VERTEX_POINT('',#49704);
#15413=VERTEX_POINT('',#49706);
#15414=VERTEX_POINT('',#49710);
#15415=VERTEX_POINT('',#49711);
#15416=VERTEX_POINT('',#49713);
#15417=VERTEX_POINT('',#49717);
#15418=VERTEX_POINT('',#49718);
#15419=VERTEX_POINT('',#49720);
#15420=VERTEX_POINT('',#49727);
#15421=VERTEX_POINT('',#49728);
#15422=VERTEX_POINT('',#49730);
#15423=VERTEX_POINT('',#49758);
#15424=VERTEX_POINT('',#49759);
#15425=VERTEX_POINT('',#49761);
#15426=VERTEX_POINT('',#49765);
#15427=VERTEX_POINT('',#49766);
#15428=VERTEX_POINT('',#49768);
#15429=VERTEX_POINT('',#49772);
#15430=VERTEX_POINT('',#49773);
#15431=VERTEX_POINT('',#49775);
#15432=VERTEX_POINT('',#49782);
#15433=VERTEX_POINT('',#49783);
#15434=VERTEX_POINT('',#49785);
#15435=VERTEX_POINT('',#49813);
#15436=VERTEX_POINT('',#49814);
#15437=VERTEX_POINT('',#49817);
#15438=VERTEX_POINT('',#49821);
#15439=VERTEX_POINT('',#49825);
#15440=VERTEX_POINT('',#49827);
#15441=VERTEX_POINT('',#49831);
#15442=VERTEX_POINT('',#49833);
#15443=VERTEX_POINT('',#49837);
#15444=VERTEX_POINT('',#49841);
#15445=VERTEX_POINT('',#49848);
#15446=VERTEX_POINT('',#49849);
#15447=VERTEX_POINT('',#49851);
#15448=VERTEX_POINT('',#49868);
#15449=VERTEX_POINT('',#49869);
#15450=VERTEX_POINT('',#49871);
#15451=VERTEX_POINT('',#49875);
#15452=VERTEX_POINT('',#49876);
#15453=VERTEX_POINT('',#49878);
#15454=VERTEX_POINT('',#49882);
#15455=VERTEX_POINT('',#49883);
#15456=VERTEX_POINT('',#49885);
#15457=VERTEX_POINT('',#49892);
#15458=VERTEX_POINT('',#49893);
#15459=VERTEX_POINT('',#49895);
#15460=VERTEX_POINT('',#49923);
#15461=VERTEX_POINT('',#49924);
#15462=VERTEX_POINT('',#49926);
#15463=VERTEX_POINT('',#49930);
#15464=VERTEX_POINT('',#49931);
#15465=VERTEX_POINT('',#49934);
#15466=VERTEX_POINT('',#49941);
#15467=VERTEX_POINT('',#49942);
#15468=VERTEX_POINT('',#49944);
#15469=VERTEX_POINT('',#49948);
#15470=VERTEX_POINT('',#49949);
#15471=VERTEX_POINT('',#49952);
#15472=VERTEX_POINT('',#49962);
#15473=VERTEX_POINT('',#49969);
#15474=VERTEX_POINT('',#49978);
#15475=VERTEX_POINT('',#49979);
#15476=VERTEX_POINT('',#49981);
#15477=VERTEX_POINT('',#49985);
#15478=VERTEX_POINT('',#49986);
#15479=VERTEX_POINT('',#49988);
#15480=VERTEX_POINT('',#49992);
#15481=VERTEX_POINT('',#49993);
#15482=VERTEX_POINT('',#49995);
#15483=VERTEX_POINT('',#50002);
#15484=VERTEX_POINT('',#50003);
#15485=VERTEX_POINT('',#50005);
#15486=VERTEX_POINT('',#50033);
#15487=VERTEX_POINT('',#50034);
#15488=VERTEX_POINT('',#50036);
#15489=VERTEX_POINT('',#50040);
#15490=VERTEX_POINT('',#50041);
#15491=VERTEX_POINT('',#50043);
#15492=VERTEX_POINT('',#50047);
#15493=VERTEX_POINT('',#50048);
#15494=VERTEX_POINT('',#50050);
#15495=VERTEX_POINT('',#50057);
#15496=VERTEX_POINT('',#50058);
#15497=VERTEX_POINT('',#50060);
#15498=VERTEX_POINT('',#50088);
#15499=VERTEX_POINT('',#50089);
#15500=VERTEX_POINT('',#50092);
#15501=VERTEX_POINT('',#50096);
#15502=VERTEX_POINT('',#50100);
#15503=VERTEX_POINT('',#50102);
#15504=VERTEX_POINT('',#50106);
#15505=VERTEX_POINT('',#50108);
#15506=VERTEX_POINT('',#50112);
#15507=VERTEX_POINT('',#50116);
#15508=VERTEX_POINT('',#50123);
#15509=VERTEX_POINT('',#50124);
#15510=VERTEX_POINT('',#50126);
#15511=VERTEX_POINT('',#50143);
#15512=VERTEX_POINT('',#50144);
#15513=VERTEX_POINT('',#50146);
#15514=VERTEX_POINT('',#50150);
#15515=VERTEX_POINT('',#50151);
#15516=VERTEX_POINT('',#50153);
#15517=VERTEX_POINT('',#50157);
#15518=VERTEX_POINT('',#50158);
#15519=VERTEX_POINT('',#50160);
#15520=VERTEX_POINT('',#50167);
#15521=VERTEX_POINT('',#50168);
#15522=VERTEX_POINT('',#50170);
#15523=VERTEX_POINT('',#50198);
#15524=VERTEX_POINT('',#50199);
#15525=VERTEX_POINT('',#50201);
#15526=VERTEX_POINT('',#50205);
#15527=VERTEX_POINT('',#50206);
#15528=VERTEX_POINT('',#50209);
#15529=VERTEX_POINT('',#50216);
#15530=VERTEX_POINT('',#50217);
#15531=VERTEX_POINT('',#50219);
#15532=VERTEX_POINT('',#50223);
#15533=VERTEX_POINT('',#50224);
#15534=VERTEX_POINT('',#50227);
#15535=VERTEX_POINT('',#50237);
#15536=VERTEX_POINT('',#50244);
#15537=VERTEX_POINT('',#50253);
#15538=VERTEX_POINT('',#50254);
#15539=VERTEX_POINT('',#50256);
#15540=VERTEX_POINT('',#50260);
#15541=VERTEX_POINT('',#50261);
#15542=VERTEX_POINT('',#50263);
#15543=VERTEX_POINT('',#50267);
#15544=VERTEX_POINT('',#50268);
#15545=VERTEX_POINT('',#50270);
#15546=VERTEX_POINT('',#50277);
#15547=VERTEX_POINT('',#50278);
#15548=VERTEX_POINT('',#50280);
#15549=VERTEX_POINT('',#50308);
#15550=VERTEX_POINT('',#50309);
#15551=VERTEX_POINT('',#50311);
#15552=VERTEX_POINT('',#50315);
#15553=VERTEX_POINT('',#50316);
#15554=VERTEX_POINT('',#50318);
#15555=VERTEX_POINT('',#50322);
#15556=VERTEX_POINT('',#50323);
#15557=VERTEX_POINT('',#50325);
#15558=VERTEX_POINT('',#50332);
#15559=VERTEX_POINT('',#50333);
#15560=VERTEX_POINT('',#50335);
#15561=VERTEX_POINT('',#50363);
#15562=VERTEX_POINT('',#50364);
#15563=VERTEX_POINT('',#50367);
#15564=VERTEX_POINT('',#50371);
#15565=VERTEX_POINT('',#50375);
#15566=VERTEX_POINT('',#50377);
#15567=VERTEX_POINT('',#50381);
#15568=VERTEX_POINT('',#50383);
#15569=VERTEX_POINT('',#50387);
#15570=VERTEX_POINT('',#50391);
#15571=VERTEX_POINT('',#50398);
#15572=VERTEX_POINT('',#50399);
#15573=VERTEX_POINT('',#50401);
#15574=VERTEX_POINT('',#50418);
#15575=VERTEX_POINT('',#50419);
#15576=VERTEX_POINT('',#50421);
#15577=VERTEX_POINT('',#50425);
#15578=VERTEX_POINT('',#50426);
#15579=VERTEX_POINT('',#50428);
#15580=VERTEX_POINT('',#50432);
#15581=VERTEX_POINT('',#50433);
#15582=VERTEX_POINT('',#50435);
#15583=VERTEX_POINT('',#50442);
#15584=VERTEX_POINT('',#50443);
#15585=VERTEX_POINT('',#50445);
#15586=VERTEX_POINT('',#50473);
#15587=VERTEX_POINT('',#50474);
#15588=VERTEX_POINT('',#50476);
#15589=VERTEX_POINT('',#50480);
#15590=VERTEX_POINT('',#50481);
#15591=VERTEX_POINT('',#50484);
#15592=VERTEX_POINT('',#50491);
#15593=VERTEX_POINT('',#50492);
#15594=VERTEX_POINT('',#50494);
#15595=VERTEX_POINT('',#50498);
#15596=VERTEX_POINT('',#50499);
#15597=VERTEX_POINT('',#50502);
#15598=VERTEX_POINT('',#50512);
#15599=VERTEX_POINT('',#50519);
#15600=VERTEX_POINT('',#50528);
#15601=VERTEX_POINT('',#50529);
#15602=VERTEX_POINT('',#50531);
#15603=VERTEX_POINT('',#50535);
#15604=VERTEX_POINT('',#50536);
#15605=VERTEX_POINT('',#50538);
#15606=VERTEX_POINT('',#50542);
#15607=VERTEX_POINT('',#50543);
#15608=VERTEX_POINT('',#50545);
#15609=VERTEX_POINT('',#50552);
#15610=VERTEX_POINT('',#50553);
#15611=VERTEX_POINT('',#50555);
#15612=VERTEX_POINT('',#50583);
#15613=VERTEX_POINT('',#50584);
#15614=VERTEX_POINT('',#50586);
#15615=VERTEX_POINT('',#50590);
#15616=VERTEX_POINT('',#50591);
#15617=VERTEX_POINT('',#50593);
#15618=VERTEX_POINT('',#50597);
#15619=VERTEX_POINT('',#50598);
#15620=VERTEX_POINT('',#50600);
#15621=VERTEX_POINT('',#50607);
#15622=VERTEX_POINT('',#50608);
#15623=VERTEX_POINT('',#50610);
#15624=VERTEX_POINT('',#50638);
#15625=VERTEX_POINT('',#50639);
#15626=VERTEX_POINT('',#50642);
#15627=VERTEX_POINT('',#50646);
#15628=VERTEX_POINT('',#50650);
#15629=VERTEX_POINT('',#50652);
#15630=VERTEX_POINT('',#50656);
#15631=VERTEX_POINT('',#50658);
#15632=VERTEX_POINT('',#50662);
#15633=VERTEX_POINT('',#50666);
#15634=VERTEX_POINT('',#50673);
#15635=VERTEX_POINT('',#50674);
#15636=VERTEX_POINT('',#50676);
#15637=VERTEX_POINT('',#50693);
#15638=VERTEX_POINT('',#50694);
#15639=VERTEX_POINT('',#50696);
#15640=VERTEX_POINT('',#50700);
#15641=VERTEX_POINT('',#50701);
#15642=VERTEX_POINT('',#50703);
#15643=VERTEX_POINT('',#50707);
#15644=VERTEX_POINT('',#50708);
#15645=VERTEX_POINT('',#50710);
#15646=VERTEX_POINT('',#50717);
#15647=VERTEX_POINT('',#50718);
#15648=VERTEX_POINT('',#50720);
#15649=VERTEX_POINT('',#50748);
#15650=VERTEX_POINT('',#50749);
#15651=VERTEX_POINT('',#50751);
#15652=VERTEX_POINT('',#50755);
#15653=VERTEX_POINT('',#50756);
#15654=VERTEX_POINT('',#50759);
#15655=VERTEX_POINT('',#50766);
#15656=VERTEX_POINT('',#50767);
#15657=VERTEX_POINT('',#50769);
#15658=VERTEX_POINT('',#50773);
#15659=VERTEX_POINT('',#50774);
#15660=VERTEX_POINT('',#50777);
#15661=VERTEX_POINT('',#50787);
#15662=VERTEX_POINT('',#50794);
#15663=VERTEX_POINT('',#50803);
#15664=VERTEX_POINT('',#50804);
#15665=VERTEX_POINT('',#50806);
#15666=VERTEX_POINT('',#50810);
#15667=VERTEX_POINT('',#50811);
#15668=VERTEX_POINT('',#50813);
#15669=VERTEX_POINT('',#50817);
#15670=VERTEX_POINT('',#50818);
#15671=VERTEX_POINT('',#50820);
#15672=VERTEX_POINT('',#50827);
#15673=VERTEX_POINT('',#50828);
#15674=VERTEX_POINT('',#50830);
#15675=VERTEX_POINT('',#50858);
#15676=VERTEX_POINT('',#50859);
#15677=VERTEX_POINT('',#50861);
#15678=VERTEX_POINT('',#50865);
#15679=VERTEX_POINT('',#50866);
#15680=VERTEX_POINT('',#50868);
#15681=VERTEX_POINT('',#50872);
#15682=VERTEX_POINT('',#50873);
#15683=VERTEX_POINT('',#50875);
#15684=VERTEX_POINT('',#50882);
#15685=VERTEX_POINT('',#50883);
#15686=VERTEX_POINT('',#50885);
#15687=VERTEX_POINT('',#50913);
#15688=VERTEX_POINT('',#50914);
#15689=VERTEX_POINT('',#50917);
#15690=VERTEX_POINT('',#50921);
#15691=VERTEX_POINT('',#50925);
#15692=VERTEX_POINT('',#50927);
#15693=VERTEX_POINT('',#50931);
#15694=VERTEX_POINT('',#50933);
#15695=VERTEX_POINT('',#50937);
#15696=VERTEX_POINT('',#50941);
#15697=VERTEX_POINT('',#50948);
#15698=VERTEX_POINT('',#50949);
#15699=VERTEX_POINT('',#50951);
#15700=VERTEX_POINT('',#50968);
#15701=VERTEX_POINT('',#50969);
#15702=VERTEX_POINT('',#50971);
#15703=VERTEX_POINT('',#50975);
#15704=VERTEX_POINT('',#50976);
#15705=VERTEX_POINT('',#50978);
#15706=VERTEX_POINT('',#50982);
#15707=VERTEX_POINT('',#50983);
#15708=VERTEX_POINT('',#50985);
#15709=VERTEX_POINT('',#50992);
#15710=VERTEX_POINT('',#50993);
#15711=VERTEX_POINT('',#50995);
#15712=VERTEX_POINT('',#51023);
#15713=VERTEX_POINT('',#51024);
#15714=VERTEX_POINT('',#51026);
#15715=VERTEX_POINT('',#51030);
#15716=VERTEX_POINT('',#51031);
#15717=VERTEX_POINT('',#51034);
#15718=VERTEX_POINT('',#51041);
#15719=VERTEX_POINT('',#51042);
#15720=VERTEX_POINT('',#51044);
#15721=VERTEX_POINT('',#51048);
#15722=VERTEX_POINT('',#51049);
#15723=VERTEX_POINT('',#51052);
#15724=VERTEX_POINT('',#51062);
#15725=VERTEX_POINT('',#51069);
#15726=VERTEX_POINT('',#51078);
#15727=VERTEX_POINT('',#51079);
#15728=VERTEX_POINT('',#51081);
#15729=VERTEX_POINT('',#51085);
#15730=VERTEX_POINT('',#51086);
#15731=VERTEX_POINT('',#51088);
#15732=VERTEX_POINT('',#51092);
#15733=VERTEX_POINT('',#51093);
#15734=VERTEX_POINT('',#51095);
#15735=VERTEX_POINT('',#51102);
#15736=VERTEX_POINT('',#51103);
#15737=VERTEX_POINT('',#51105);
#15738=VERTEX_POINT('',#51133);
#15739=VERTEX_POINT('',#51134);
#15740=VERTEX_POINT('',#51136);
#15741=VERTEX_POINT('',#51140);
#15742=VERTEX_POINT('',#51141);
#15743=VERTEX_POINT('',#51143);
#15744=VERTEX_POINT('',#51147);
#15745=VERTEX_POINT('',#51148);
#15746=VERTEX_POINT('',#51150);
#15747=VERTEX_POINT('',#51157);
#15748=VERTEX_POINT('',#51158);
#15749=VERTEX_POINT('',#51160);
#15750=VERTEX_POINT('',#51188);
#15751=VERTEX_POINT('',#51189);
#15752=VERTEX_POINT('',#51192);
#15753=VERTEX_POINT('',#51196);
#15754=VERTEX_POINT('',#51200);
#15755=VERTEX_POINT('',#51202);
#15756=VERTEX_POINT('',#51206);
#15757=VERTEX_POINT('',#51208);
#15758=VERTEX_POINT('',#51212);
#15759=VERTEX_POINT('',#51216);
#15760=VERTEX_POINT('',#51223);
#15761=VERTEX_POINT('',#51224);
#15762=VERTEX_POINT('',#51226);
#15763=VERTEX_POINT('',#51243);
#15764=VERTEX_POINT('',#51244);
#15765=VERTEX_POINT('',#51246);
#15766=VERTEX_POINT('',#51250);
#15767=VERTEX_POINT('',#51251);
#15768=VERTEX_POINT('',#51253);
#15769=VERTEX_POINT('',#51257);
#15770=VERTEX_POINT('',#51258);
#15771=VERTEX_POINT('',#51260);
#15772=VERTEX_POINT('',#51267);
#15773=VERTEX_POINT('',#51268);
#15774=VERTEX_POINT('',#51270);
#15775=VERTEX_POINT('',#51298);
#15776=VERTEX_POINT('',#51299);
#15777=VERTEX_POINT('',#51301);
#15778=VERTEX_POINT('',#51305);
#15779=VERTEX_POINT('',#51306);
#15780=VERTEX_POINT('',#51309);
#15781=VERTEX_POINT('',#51316);
#15782=VERTEX_POINT('',#51317);
#15783=VERTEX_POINT('',#51319);
#15784=VERTEX_POINT('',#51323);
#15785=VERTEX_POINT('',#51324);
#15786=VERTEX_POINT('',#51327);
#15787=VERTEX_POINT('',#51337);
#15788=VERTEX_POINT('',#51344);
#15789=VERTEX_POINT('',#51353);
#15790=VERTEX_POINT('',#51354);
#15791=VERTEX_POINT('',#51356);
#15792=VERTEX_POINT('',#51360);
#15793=VERTEX_POINT('',#51361);
#15794=VERTEX_POINT('',#51363);
#15795=VERTEX_POINT('',#51367);
#15796=VERTEX_POINT('',#51368);
#15797=VERTEX_POINT('',#51370);
#15798=VERTEX_POINT('',#51377);
#15799=VERTEX_POINT('',#51378);
#15800=VERTEX_POINT('',#51380);
#15801=VERTEX_POINT('',#51408);
#15802=VERTEX_POINT('',#51409);
#15803=VERTEX_POINT('',#51411);
#15804=VERTEX_POINT('',#51415);
#15805=VERTEX_POINT('',#51416);
#15806=VERTEX_POINT('',#51418);
#15807=VERTEX_POINT('',#51422);
#15808=VERTEX_POINT('',#51423);
#15809=VERTEX_POINT('',#51425);
#15810=VERTEX_POINT('',#51432);
#15811=VERTEX_POINT('',#51433);
#15812=VERTEX_POINT('',#51435);
#15813=VERTEX_POINT('',#51463);
#15814=VERTEX_POINT('',#51464);
#15815=VERTEX_POINT('',#51467);
#15816=VERTEX_POINT('',#51471);
#15817=VERTEX_POINT('',#51475);
#15818=VERTEX_POINT('',#51477);
#15819=VERTEX_POINT('',#51481);
#15820=VERTEX_POINT('',#51483);
#15821=VERTEX_POINT('',#51487);
#15822=VERTEX_POINT('',#51491);
#15823=VERTEX_POINT('',#51498);
#15824=VERTEX_POINT('',#51499);
#15825=VERTEX_POINT('',#51501);
#15826=VERTEX_POINT('',#51518);
#15827=VERTEX_POINT('',#51519);
#15828=VERTEX_POINT('',#51521);
#15829=VERTEX_POINT('',#51525);
#15830=VERTEX_POINT('',#51526);
#15831=VERTEX_POINT('',#51528);
#15832=VERTEX_POINT('',#51532);
#15833=VERTEX_POINT('',#51533);
#15834=VERTEX_POINT('',#51535);
#15835=VERTEX_POINT('',#51542);
#15836=VERTEX_POINT('',#51543);
#15837=VERTEX_POINT('',#51545);
#15838=VERTEX_POINT('',#51573);
#15839=VERTEX_POINT('',#51574);
#15840=VERTEX_POINT('',#51576);
#15841=VERTEX_POINT('',#51580);
#15842=VERTEX_POINT('',#51581);
#15843=VERTEX_POINT('',#51584);
#15844=VERTEX_POINT('',#51591);
#15845=VERTEX_POINT('',#51592);
#15846=VERTEX_POINT('',#51594);
#15847=VERTEX_POINT('',#51598);
#15848=VERTEX_POINT('',#51599);
#15849=VERTEX_POINT('',#51602);
#15850=VERTEX_POINT('',#51612);
#15851=VERTEX_POINT('',#51619);
#15852=VERTEX_POINT('',#51628);
#15853=VERTEX_POINT('',#51629);
#15854=VERTEX_POINT('',#51631);
#15855=VERTEX_POINT('',#51635);
#15856=VERTEX_POINT('',#51636);
#15857=VERTEX_POINT('',#51638);
#15858=VERTEX_POINT('',#51642);
#15859=VERTEX_POINT('',#51643);
#15860=VERTEX_POINT('',#51645);
#15861=VERTEX_POINT('',#51652);
#15862=VERTEX_POINT('',#51653);
#15863=VERTEX_POINT('',#51655);
#15864=VERTEX_POINT('',#51683);
#15865=VERTEX_POINT('',#51684);
#15866=VERTEX_POINT('',#51686);
#15867=VERTEX_POINT('',#51690);
#15868=VERTEX_POINT('',#51691);
#15869=VERTEX_POINT('',#51693);
#15870=VERTEX_POINT('',#51697);
#15871=VERTEX_POINT('',#51698);
#15872=VERTEX_POINT('',#51700);
#15873=VERTEX_POINT('',#51707);
#15874=VERTEX_POINT('',#51708);
#15875=VERTEX_POINT('',#51710);
#15876=VERTEX_POINT('',#51738);
#15877=VERTEX_POINT('',#51739);
#15878=VERTEX_POINT('',#51742);
#15879=VERTEX_POINT('',#51746);
#15880=VERTEX_POINT('',#51750);
#15881=VERTEX_POINT('',#51752);
#15882=VERTEX_POINT('',#51756);
#15883=VERTEX_POINT('',#51758);
#15884=VERTEX_POINT('',#51762);
#15885=VERTEX_POINT('',#51766);
#15886=VERTEX_POINT('',#51773);
#15887=VERTEX_POINT('',#51774);
#15888=VERTEX_POINT('',#51776);
#15889=VERTEX_POINT('',#51793);
#15890=VERTEX_POINT('',#51794);
#15891=VERTEX_POINT('',#51796);
#15892=VERTEX_POINT('',#51800);
#15893=VERTEX_POINT('',#51801);
#15894=VERTEX_POINT('',#51803);
#15895=VERTEX_POINT('',#51807);
#15896=VERTEX_POINT('',#51808);
#15897=VERTEX_POINT('',#51810);
#15898=VERTEX_POINT('',#51817);
#15899=VERTEX_POINT('',#51818);
#15900=VERTEX_POINT('',#51820);
#15901=VERTEX_POINT('',#51848);
#15902=VERTEX_POINT('',#51849);
#15903=VERTEX_POINT('',#51851);
#15904=VERTEX_POINT('',#51855);
#15905=VERTEX_POINT('',#51856);
#15906=VERTEX_POINT('',#51859);
#15907=VERTEX_POINT('',#51866);
#15908=VERTEX_POINT('',#51867);
#15909=VERTEX_POINT('',#51869);
#15910=VERTEX_POINT('',#51873);
#15911=VERTEX_POINT('',#51874);
#15912=VERTEX_POINT('',#51877);
#15913=VERTEX_POINT('',#51887);
#15914=VERTEX_POINT('',#51894);
#15915=VERTEX_POINT('',#51903);
#15916=VERTEX_POINT('',#51904);
#15917=VERTEX_POINT('',#51906);
#15918=VERTEX_POINT('',#51910);
#15919=VERTEX_POINT('',#51911);
#15920=VERTEX_POINT('',#51913);
#15921=VERTEX_POINT('',#51917);
#15922=VERTEX_POINT('',#51918);
#15923=VERTEX_POINT('',#51920);
#15924=VERTEX_POINT('',#51927);
#15925=VERTEX_POINT('',#51928);
#15926=VERTEX_POINT('',#51930);
#15927=VERTEX_POINT('',#51958);
#15928=VERTEX_POINT('',#51959);
#15929=VERTEX_POINT('',#51961);
#15930=VERTEX_POINT('',#51965);
#15931=VERTEX_POINT('',#51966);
#15932=VERTEX_POINT('',#51968);
#15933=VERTEX_POINT('',#51972);
#15934=VERTEX_POINT('',#51973);
#15935=VERTEX_POINT('',#51975);
#15936=VERTEX_POINT('',#51982);
#15937=VERTEX_POINT('',#51983);
#15938=VERTEX_POINT('',#51985);
#15939=VERTEX_POINT('',#52013);
#15940=VERTEX_POINT('',#52014);
#15941=VERTEX_POINT('',#52017);
#15942=VERTEX_POINT('',#52021);
#15943=VERTEX_POINT('',#52025);
#15944=VERTEX_POINT('',#52027);
#15945=VERTEX_POINT('',#52031);
#15946=VERTEX_POINT('',#52033);
#15947=VERTEX_POINT('',#52037);
#15948=VERTEX_POINT('',#52041);
#15949=VERTEX_POINT('',#52048);
#15950=VERTEX_POINT('',#52049);
#15951=VERTEX_POINT('',#52051);
#15952=VERTEX_POINT('',#52068);
#15953=VERTEX_POINT('',#52069);
#15954=VERTEX_POINT('',#52071);
#15955=VERTEX_POINT('',#52075);
#15956=VERTEX_POINT('',#52076);
#15957=VERTEX_POINT('',#52078);
#15958=VERTEX_POINT('',#52082);
#15959=VERTEX_POINT('',#52083);
#15960=VERTEX_POINT('',#52085);
#15961=VERTEX_POINT('',#52092);
#15962=VERTEX_POINT('',#52093);
#15963=VERTEX_POINT('',#52095);
#15964=VERTEX_POINT('',#52123);
#15965=VERTEX_POINT('',#52124);
#15966=VERTEX_POINT('',#52126);
#15967=VERTEX_POINT('',#52130);
#15968=VERTEX_POINT('',#52131);
#15969=VERTEX_POINT('',#52134);
#15970=VERTEX_POINT('',#52141);
#15971=VERTEX_POINT('',#52142);
#15972=VERTEX_POINT('',#52144);
#15973=VERTEX_POINT('',#52148);
#15974=VERTEX_POINT('',#52149);
#15975=VERTEX_POINT('',#52152);
#15976=VERTEX_POINT('',#52162);
#15977=VERTEX_POINT('',#52169);
#15978=VERTEX_POINT('',#52178);
#15979=VERTEX_POINT('',#52179);
#15980=VERTEX_POINT('',#52181);
#15981=VERTEX_POINT('',#52185);
#15982=VERTEX_POINT('',#52186);
#15983=VERTEX_POINT('',#52188);
#15984=VERTEX_POINT('',#52192);
#15985=VERTEX_POINT('',#52193);
#15986=VERTEX_POINT('',#52195);
#15987=VERTEX_POINT('',#52202);
#15988=VERTEX_POINT('',#52203);
#15989=VERTEX_POINT('',#52205);
#15990=VERTEX_POINT('',#52233);
#15991=VERTEX_POINT('',#52234);
#15992=VERTEX_POINT('',#52236);
#15993=VERTEX_POINT('',#52240);
#15994=VERTEX_POINT('',#52241);
#15995=VERTEX_POINT('',#52243);
#15996=VERTEX_POINT('',#52247);
#15997=VERTEX_POINT('',#52248);
#15998=VERTEX_POINT('',#52250);
#15999=VERTEX_POINT('',#52257);
#16000=VERTEX_POINT('',#52258);
#16001=VERTEX_POINT('',#52260);
#16002=VERTEX_POINT('',#52288);
#16003=VERTEX_POINT('',#52289);
#16004=VERTEX_POINT('',#52292);
#16005=VERTEX_POINT('',#52296);
#16006=VERTEX_POINT('',#52300);
#16007=VERTEX_POINT('',#52302);
#16008=VERTEX_POINT('',#52306);
#16009=VERTEX_POINT('',#52308);
#16010=VERTEX_POINT('',#52312);
#16011=VERTEX_POINT('',#52316);
#16012=VERTEX_POINT('',#52323);
#16013=VERTEX_POINT('',#52324);
#16014=VERTEX_POINT('',#52326);
#16015=VERTEX_POINT('',#52343);
#16016=VERTEX_POINT('',#52344);
#16017=VERTEX_POINT('',#52346);
#16018=VERTEX_POINT('',#52350);
#16019=VERTEX_POINT('',#52351);
#16020=VERTEX_POINT('',#52353);
#16021=VERTEX_POINT('',#52357);
#16022=VERTEX_POINT('',#52358);
#16023=VERTEX_POINT('',#52360);
#16024=VERTEX_POINT('',#52367);
#16025=VERTEX_POINT('',#52368);
#16026=VERTEX_POINT('',#52370);
#16027=VERTEX_POINT('',#52398);
#16028=VERTEX_POINT('',#52399);
#16029=VERTEX_POINT('',#52401);
#16030=VERTEX_POINT('',#52405);
#16031=VERTEX_POINT('',#52406);
#16032=VERTEX_POINT('',#52409);
#16033=VERTEX_POINT('',#52416);
#16034=VERTEX_POINT('',#52417);
#16035=VERTEX_POINT('',#52419);
#16036=VERTEX_POINT('',#52423);
#16037=VERTEX_POINT('',#52424);
#16038=VERTEX_POINT('',#52427);
#16039=VERTEX_POINT('',#52437);
#16040=VERTEX_POINT('',#52444);
#16041=VERTEX_POINT('',#52453);
#16042=VERTEX_POINT('',#52454);
#16043=VERTEX_POINT('',#52456);
#16044=VERTEX_POINT('',#52460);
#16045=VERTEX_POINT('',#52461);
#16046=VERTEX_POINT('',#52463);
#16047=VERTEX_POINT('',#52467);
#16048=VERTEX_POINT('',#52468);
#16049=VERTEX_POINT('',#52470);
#16050=VERTEX_POINT('',#52477);
#16051=VERTEX_POINT('',#52478);
#16052=VERTEX_POINT('',#52480);
#16053=VERTEX_POINT('',#52508);
#16054=VERTEX_POINT('',#52509);
#16055=VERTEX_POINT('',#52511);
#16056=VERTEX_POINT('',#52515);
#16057=VERTEX_POINT('',#52516);
#16058=VERTEX_POINT('',#52518);
#16059=VERTEX_POINT('',#52522);
#16060=VERTEX_POINT('',#52523);
#16061=VERTEX_POINT('',#52525);
#16062=VERTEX_POINT('',#52532);
#16063=VERTEX_POINT('',#52533);
#16064=VERTEX_POINT('',#52535);
#16065=VERTEX_POINT('',#52563);
#16066=VERTEX_POINT('',#52564);
#16067=VERTEX_POINT('',#52567);
#16068=VERTEX_POINT('',#52569);
#16069=VERTEX_POINT('',#52573);
#16070=VERTEX_POINT('',#52575);
#16071=VERTEX_POINT('',#52579);
#16072=VERTEX_POINT('',#52583);
#16073=VERTEX_POINT('',#52584);
#16074=VERTEX_POINT('',#52586);
#16075=VERTEX_POINT('',#52590);
#16076=VERTEX_POINT('',#52591);
#16077=VERTEX_POINT('',#52593);
#16078=VERTEX_POINT('',#52597);
#16079=VERTEX_POINT('',#52598);
#16080=VERTEX_POINT('',#52600);
#16081=VERTEX_POINT('',#52607);
#16082=VERTEX_POINT('',#52608);
#16083=VERTEX_POINT('',#52610);
#16084=VERTEX_POINT('',#52638);
#16085=VERTEX_POINT('',#52639);
#16086=VERTEX_POINT('',#52641);
#16087=VERTEX_POINT('',#52645);
#16088=VERTEX_POINT('',#52646);
#16089=VERTEX_POINT('',#52648);
#16090=VERTEX_POINT('',#52652);
#16091=VERTEX_POINT('',#52653);
#16092=VERTEX_POINT('',#52655);
#16093=VERTEX_POINT('',#52662);
#16094=VERTEX_POINT('',#52663);
#16095=VERTEX_POINT('',#52665);
#16096=VERTEX_POINT('',#52693);
#16097=VERTEX_POINT('',#52694);
#16098=VERTEX_POINT('',#52697);
#16099=VERTEX_POINT('',#52699);
#16100=VERTEX_POINT('',#52703);
#16101=VERTEX_POINT('',#52705);
#16102=VERTEX_POINT('',#52711);
#16103=VERTEX_POINT('',#52715);
#16104=VERTEX_POINT('',#52718);
#16105=VERTEX_POINT('',#52722);
#16106=VERTEX_POINT('',#52872);
#16107=VERTEX_POINT('',#52876);
#16108=VERTEX_POINT('',#52880);
#16109=VERTEX_POINT('',#52884);
#16110=VERTEX_POINT('',#52888);
#16111=VERTEX_POINT('',#52892);
#16112=VERTEX_POINT('',#52894);
#16113=VERTEX_POINT('',#52898);
#16114=VERTEX_POINT('',#52902);
#16115=VERTEX_POINT('',#52906);
#16116=VERTEX_POINT('',#52910);
#16117=VERTEX_POINT('',#52917);
#16118=VERTEX_POINT('',#52922);
#16119=VERTEX_POINT('',#52927);
#16120=VERTEX_POINT('',#52931);
#16121=VERTEX_POINT('',#52934);
#16122=VERTEX_POINT('',#52940);
#16123=VERTEX_POINT('',#52944);
#16124=VERTEX_POINT('',#52947);
#16125=VERTEX_POINT('',#52954);
#16126=VERTEX_POINT('',#52955);
#16127=VERTEX_POINT('',#52957);
#16128=VERTEX_POINT('',#52971);
#16129=VERTEX_POINT('',#52976);
#16130=VERTEX_POINT('',#52986);
#16131=VERTEX_POINT('',#52993);
#16132=VERTEX_POINT('',#53008);
#16133=VERTEX_POINT('',#53009);
#16134=VERTEX_POINT('',#53045);
#16135=VERTEX_POINT('',#53046);
#16136=VERTEX_POINT('',#53083);
#16137=VERTEX_POINT('',#53084);
#16138=VERTEX_POINT('',#53121);
#16139=VERTEX_POINT('',#53122);
#16140=VERTEX_POINT('',#53158);
#16141=VERTEX_POINT('',#53159);
#16142=VERTEX_POINT('',#53195);
#16143=VERTEX_POINT('',#53196);
#16144=VERTEX_POINT('',#53198);
#16145=VERTEX_POINT('',#53214);
#16146=VERTEX_POINT('',#53229);
#16147=VERTEX_POINT('',#53230);
#16148=VERTEX_POINT('',#53267);
#16149=VERTEX_POINT('',#53268);
#16150=VERTEX_POINT('',#53304);
#16151=VERTEX_POINT('',#53306);
#16152=VERTEX_POINT('',#53310);
#16153=VERTEX_POINT('',#53313);
#16154=VERTEX_POINT('',#53316);
#16155=VERTEX_POINT('',#53317);
#16156=VERTEX_POINT('',#53319);
#16157=VERTEX_POINT('',#53321);
#16158=VERTEX_POINT('',#53325);
#16159=VERTEX_POINT('',#53327);
#16160=VERTEX_POINT('',#53331);
#16161=VERTEX_POINT('',#53332);
#16162=VERTEX_POINT('',#53334);
#16163=VERTEX_POINT('',#53336);
#16164=VERTEX_POINT('',#53338);
#16165=VERTEX_POINT('',#53340);
#16166=VERTEX_POINT('',#53344);
#16167=VERTEX_POINT('',#53346);
#16168=VERTEX_POINT('',#53350);
#16169=VERTEX_POINT('',#53352);
#16170=VERTEX_POINT('',#53356);
#16171=VERTEX_POINT('',#53358);
#16172=VERTEX_POINT('',#53360);
#16173=VERTEX_POINT('',#53364);
#16174=VERTEX_POINT('',#53365);
#16175=VERTEX_POINT('',#53367);
#16176=VERTEX_POINT('',#53372);
#16177=VERTEX_POINT('',#53376);
#16178=VERTEX_POINT('',#53381);
#16179=VERTEX_POINT('',#53382);
#16180=VERTEX_POINT('',#53384);
#16181=VERTEX_POINT('',#53388);
#16182=VERTEX_POINT('',#53389);
#16183=VERTEX_POINT('',#53392);
#16184=VERTEX_POINT('',#53399);
#16185=VERTEX_POINT('',#53400);
#16186=VERTEX_POINT('',#53402);
#16187=VERTEX_POINT('',#53406);
#16188=VERTEX_POINT('',#53407);
#16189=VERTEX_POINT('',#53410);
#16190=VERTEX_POINT('',#53417);
#16191=VERTEX_POINT('',#53418);
#16192=VERTEX_POINT('',#53420);
#16193=VERTEX_POINT('',#53424);
#16194=VERTEX_POINT('',#53425);
#16195=VERTEX_POINT('',#53428);
#16196=VERTEX_POINT('',#53435);
#16197=VERTEX_POINT('',#53436);
#16198=VERTEX_POINT('',#53438);
#16199=VERTEX_POINT('',#53442);
#16200=VERTEX_POINT('',#53443);
#16201=VERTEX_POINT('',#53446);
#16202=VERTEX_POINT('',#53453);
#16203=VERTEX_POINT('',#53454);
#16204=VERTEX_POINT('',#53456);
#16205=VERTEX_POINT('',#53460);
#16206=VERTEX_POINT('',#53461);
#16207=VERTEX_POINT('',#53464);
#16208=VERTEX_POINT('',#53471);
#16209=VERTEX_POINT('',#53472);
#16210=VERTEX_POINT('',#53475);
#16211=VERTEX_POINT('',#53479);
#16212=VERTEX_POINT('',#53481);
#16213=VERTEX_POINT('',#53488);
#16214=VERTEX_POINT('',#53494);
#16215=VERTEX_POINT('',#53500);
#16216=VERTEX_POINT('',#53504);
#16217=VERTEX_POINT('',#53514);
#16218=VERTEX_POINT('',#53516);
#16219=VERTEX_POINT('',#53521);
#16220=VERTEX_POINT('',#53523);
#16221=VERTEX_POINT('',#53525);
#16222=VERTEX_POINT('',#53527);
#16223=VERTEX_POINT('',#53530);
#16224=VERTEX_POINT('',#53534);
#16225=VERTEX_POINT('',#53538);
#16226=VERTEX_POINT('',#53542);
#16227=VERTEX_POINT('',#53546);
#16228=VERTEX_POINT('',#53550);
#16229=VERTEX_POINT('',#53554);
#16230=VERTEX_POINT('',#53558);
#16231=VERTEX_POINT('',#53563);
#16232=VERTEX_POINT('',#53565);
#16233=VERTEX_POINT('',#53567);
#16234=VERTEX_POINT('',#53569);
#16235=VERTEX_POINT('',#53585);
#16236=VERTEX_POINT('',#53586);
#16237=VERTEX_POINT('',#53589);
#16238=VERTEX_POINT('',#53591);
#16239=VERTEX_POINT('',#53595);
#16240=VERTEX_POINT('',#53597);
#16241=VERTEX_POINT('',#53603);
#16242=VERTEX_POINT('',#53643);
#16243=VERTEX_POINT('',#53644);
#16244=VERTEX_POINT('',#53661);
#16245=VERTEX_POINT('',#53671);
#16246=VERTEX_POINT('',#53682);
#16247=VERTEX_POINT('',#53903);
#16248=VERTEX_POINT('',#53904);
#16249=VERTEX_POINT('',#53951);
#16250=VERTEX_POINT('',#53995);
#16251=VERTEX_POINT('',#54042);
#16252=VERTEX_POINT('',#54083);
#16253=VERTEX_POINT('',#54133);
#16254=VERTEX_POINT('',#54174);
#16255=VERTEX_POINT('',#54185);
#16256=VERTEX_POINT('',#54209);
#16257=VERTEX_POINT('',#54681);
#16258=VERTEX_POINT('',#54682);
#16259=VERTEX_POINT('',#54729);
#16260=VERTEX_POINT('',#54749);
#16261=VERTEX_POINT('',#54886);
#16262=VERTEX_POINT('',#54893);
#16263=VERTEX_POINT('',#54898);
#16264=VERTEX_POINT('',#54939);
#16265=VERTEX_POINT('',#54986);
#16266=VERTEX_POINT('',#55030);
#16267=VERTEX_POINT('',#55077);
#16268=VERTEX_POINT('',#55118);
#16269=VERTEX_POINT('',#55165);
#16270=VERTEX_POINT('',#55206);
#16271=VERTEX_POINT('',#55256);
#16272=VERTEX_POINT('',#55297);
#16273=VERTEX_POINT('',#55423);
#16274=VERTEX_POINT('',#55437);
#16275=VERTEX_POINT('',#55512);
#16276=VERTEX_POINT('',#55513);
#16277=VERTEX_POINT('',#55527);
#16278=VERTEX_POINT('',#55547);
#16279=VERTEX_POINT('',#55609);
#16280=VERTEX_POINT('',#55610);
#16281=VERTEX_POINT('',#55627);
#16282=VERTEX_POINT('',#55637);
#16283=VERTEX_POINT('',#55858);
#16284=VERTEX_POINT('',#55859);
#16285=VERTEX_POINT('',#55906);
#16286=VERTEX_POINT('',#56071);
#16287=VERTEX_POINT('',#56079);
#16288=VERTEX_POINT('',#56090);
#16289=VERTEX_POINT('',#56113);
#16290=VERTEX_POINT('',#56160);
#16291=VERTEX_POINT('',#56201);
#16292=VERTEX_POINT('',#56327);
#16293=VERTEX_POINT('',#56328);
#16294=VERTEX_POINT('',#56345);
#16295=VERTEX_POINT('',#56365);
#16296=VERTEX_POINT('',#56419);
#16297=VERTEX_POINT('',#56420);
#16298=VERTEX_POINT('',#56437);
#16299=VERTEX_POINT('',#56457);
#16300=VERTEX_POINT('',#56820);
#16301=VERTEX_POINT('',#56821);
#16302=VERTEX_POINT('',#56868);
#16303=VERTEX_POINT('',#56912);
#16304=VERTEX_POINT('',#56959);
#16305=VERTEX_POINT('',#57000);
#16306=VERTEX_POINT('',#57047);
#16307=VERTEX_POINT('',#57088);
#16308=VERTEX_POINT('',#57138);
#16309=VERTEX_POINT('',#57179);
#16310=VERTEX_POINT('',#57229);
#16311=VERTEX_POINT('',#57270);
#16312=VERTEX_POINT('',#57317);
#16313=VERTEX_POINT('',#57362);
#16314=VERTEX_POINT('',#57375);
#16315=VERTEX_POINT('',#57564);
#16316=VERTEX_POINT('',#57565);
#16317=VERTEX_POINT('',#57579);
#16318=VERTEX_POINT('',#57589);
#16319=VERTEX_POINT('',#57667);
#16320=VERTEX_POINT('',#57672);
#16321=VERTEX_POINT('',#57687);
#16322=VERTEX_POINT('',#57691);
#16323=VERTEX_POINT('',#57692);
#16324=VERTEX_POINT('',#57695);
#16325=VERTEX_POINT('',#57734);
#16326=VERTEX_POINT('',#57751);
#16327=VERTEX_POINT('',#57785);
#16328=VERTEX_POINT('',#57813);
#16329=VERTEX_POINT('',#57815);
#16330=VERTEX_POINT('',#57854);
#16331=VERTEX_POINT('',#57889);
#16332=VERTEX_POINT('',#57893);
#16333=VERTEX_POINT('',#57897);
#16334=VERTEX_POINT('',#57900);
#16335=VERTEX_POINT('',#57904);
#16336=VERTEX_POINT('',#57908);
#16337=VERTEX_POINT('',#57912);
#16338=VERTEX_POINT('',#57916);
#16339=VERTEX_POINT('',#57917);
#16340=VERTEX_POINT('',#57922);
#16341=VERTEX_POINT('',#57926);
#16342=VERTEX_POINT('',#57928);
#16343=VERTEX_POINT('',#57935);
#16344=VERTEX_POINT('',#57938);
#16345=VERTEX_POINT('',#57952);
#16346=VERTEX_POINT('',#57953);
#16347=VERTEX_POINT('',#57956);
#16348=VERTEX_POINT('',#57960);
#16349=VERTEX_POINT('',#57963);
#16350=VERTEX_POINT('',#57967);
#16351=VERTEX_POINT('',#57969);
#16352=VERTEX_POINT('',#57971);
#16353=VERTEX_POINT('',#57975);
#16354=VERTEX_POINT('',#57978);
#16355=VERTEX_POINT('',#57982);
#16356=VERTEX_POINT('',#57984);
#16357=VERTEX_POINT('',#57988);
#16358=VERTEX_POINT('',#57991);
#16359=VERTEX_POINT('',#57995);
#16360=VERTEX_POINT('',#58001);
#16361=VERTEX_POINT('',#58005);
#16362=VERTEX_POINT('',#58009);
#16363=VERTEX_POINT('',#58017);
#16364=VERTEX_POINT('',#58019);
#16365=VERTEX_POINT('',#58023);
#16366=VERTEX_POINT('',#58027);
#16367=VERTEX_POINT('',#58031);
#16368=VERTEX_POINT('',#58034);
#16369=VERTEX_POINT('',#58038);
#16370=VERTEX_POINT('',#58042);
#16371=VERTEX_POINT('',#58048);
#16372=VERTEX_POINT('',#58049);
#16373=VERTEX_POINT('',#58052);
#16374=VERTEX_POINT('',#58056);
#16375=VERTEX_POINT('',#58059);
#16376=VERTEX_POINT('',#58063);
#16377=VERTEX_POINT('',#58065);
#16378=VERTEX_POINT('',#58067);
#16379=VERTEX_POINT('',#58071);
#16380=VERTEX_POINT('',#58075);
#16381=VERTEX_POINT('',#58078);
#16382=VERTEX_POINT('',#58079);
#16383=VERTEX_POINT('',#58108);
#16384=VERTEX_POINT('',#58110);
#16385=VERTEX_POINT('',#58115);
#16386=VERTEX_POINT('',#58120);
#16387=VERTEX_POINT('',#58122);
#16388=VERTEX_POINT('',#58129);
#16389=VERTEX_POINT('',#58164);
#16390=VERTEX_POINT('',#58165);
#16391=VERTEX_POINT('',#58198);
#16392=VERTEX_POINT('',#58200);
#16393=VERTEX_POINT('',#58205);
#16394=VERTEX_POINT('',#58210);
#16395=VERTEX_POINT('',#58212);
#16396=VERTEX_POINT('',#58219);
#16397=VERTEX_POINT('',#58258);
#16398=VERTEX_POINT('',#58259);
#16399=VERTEX_POINT('',#58292);
#16400=VERTEX_POINT('',#58294);
#16401=VERTEX_POINT('',#58299);
#16402=VERTEX_POINT('',#58304);
#16403=VERTEX_POINT('',#58306);
#16404=VERTEX_POINT('',#58313);
#16405=VERTEX_POINT('',#58352);
#16406=VERTEX_POINT('',#58353);
#16407=VERTEX_POINT('',#58386);
#16408=VERTEX_POINT('',#58388);
#16409=VERTEX_POINT('',#58393);
#16410=VERTEX_POINT('',#58398);
#16411=VERTEX_POINT('',#58400);
#16412=VERTEX_POINT('',#58407);
#16413=VERTEX_POINT('',#58442);
#16414=VERTEX_POINT('',#58443);
#16415=VERTEX_POINT('',#58472);
#16416=VERTEX_POINT('',#58474);
#16417=VERTEX_POINT('',#58479);
#16418=VERTEX_POINT('',#58484);
#16419=VERTEX_POINT('',#58486);
#16420=VERTEX_POINT('',#58493);
#16421=VERTEX_POINT('',#58526);
#16422=VERTEX_POINT('',#58527);
#16423=VERTEX_POINT('',#58556);
#16424=VERTEX_POINT('',#58558);
#16425=VERTEX_POINT('',#58563);
#16426=VERTEX_POINT('',#58568);
#16427=VERTEX_POINT('',#58570);
#16428=VERTEX_POINT('',#58577);
#16429=VERTEX_POINT('',#58610);
#16430=VERTEX_POINT('',#58611);
#16431=VERTEX_POINT('',#58644);
#16432=VERTEX_POINT('',#58646);
#16433=VERTEX_POINT('',#58651);
#16434=VERTEX_POINT('',#58656);
#16435=VERTEX_POINT('',#58658);
#16436=VERTEX_POINT('',#58665);
#16437=VERTEX_POINT('',#58700);
#16438=VERTEX_POINT('',#58701);
#16439=VERTEX_POINT('',#58734);
#16440=VERTEX_POINT('',#58736);
#16441=VERTEX_POINT('',#58741);
#16442=VERTEX_POINT('',#58746);
#16443=VERTEX_POINT('',#58748);
#16444=VERTEX_POINT('',#58755);
#16445=VERTEX_POINT('',#58794);
#16446=VERTEX_POINT('',#58795);
#16447=VERTEX_POINT('',#58828);
#16448=VERTEX_POINT('',#58830);
#16449=VERTEX_POINT('',#58835);
#16450=VERTEX_POINT('',#58840);
#16451=VERTEX_POINT('',#58842);
#16452=VERTEX_POINT('',#58849);
#16453=VERTEX_POINT('',#58888);
#16454=VERTEX_POINT('',#58889);
#16455=VERTEX_POINT('',#58918);
#16456=VERTEX_POINT('',#58920);
#16457=VERTEX_POINT('',#58925);
#16458=VERTEX_POINT('',#58930);
#16459=VERTEX_POINT('',#58932);
#16460=VERTEX_POINT('',#58939);
#16461=VERTEX_POINT('',#58974);
#16462=VERTEX_POINT('',#58975);
#16463=VERTEX_POINT('',#58992);
#16464=VERTEX_POINT('',#58994);
#16465=VERTEX_POINT('',#58997);
#16466=VERTEX_POINT('',#59016);
#16467=VERTEX_POINT('',#59021);
#16468=VERTEX_POINT('',#59023);
#16469=VERTEX_POINT('',#59030);
#16470=VERTEX_POINT('',#59033);
#16471=VERTEX_POINT('',#59072);
#16472=VERTEX_POINT('',#59073);
#16473=VERTEX_POINT('',#59102);
#16474=VERTEX_POINT('',#59104);
#16475=VERTEX_POINT('',#59109);
#16476=VERTEX_POINT('',#59114);
#16477=VERTEX_POINT('',#59116);
#16478=VERTEX_POINT('',#59123);
#16479=VERTEX_POINT('',#59158);
#16480=VERTEX_POINT('',#59159);
#16481=VERTEX_POINT('',#59192);
#16482=VERTEX_POINT('',#59194);
#16483=VERTEX_POINT('',#59199);
#16484=VERTEX_POINT('',#59204);
#16485=VERTEX_POINT('',#59206);
#16486=VERTEX_POINT('',#59213);
#16487=VERTEX_POINT('',#59252);
#16488=VERTEX_POINT('',#59253);
#16489=VERTEX_POINT('',#59286);
#16490=VERTEX_POINT('',#59288);
#16491=VERTEX_POINT('',#59293);
#16492=VERTEX_POINT('',#59298);
#16493=VERTEX_POINT('',#59300);
#16494=VERTEX_POINT('',#59307);
#16495=VERTEX_POINT('',#59346);
#16496=VERTEX_POINT('',#59347);
#16497=VERTEX_POINT('',#59380);
#16498=VERTEX_POINT('',#59382);
#16499=VERTEX_POINT('',#59387);
#16500=VERTEX_POINT('',#59392);
#16501=VERTEX_POINT('',#59394);
#16502=VERTEX_POINT('',#59401);
#16503=VERTEX_POINT('',#59436);
#16504=VERTEX_POINT('',#59437);
#16505=VERTEX_POINT('',#59466);
#16506=VERTEX_POINT('',#59468);
#16507=VERTEX_POINT('',#59473);
#16508=VERTEX_POINT('',#59478);
#16509=VERTEX_POINT('',#59480);
#16510=VERTEX_POINT('',#59487);
#16511=VERTEX_POINT('',#59520);
#16512=VERTEX_POINT('',#59521);
#16513=VERTEX_POINT('',#59550);
#16514=VERTEX_POINT('',#59552);
#16515=VERTEX_POINT('',#59557);
#16516=VERTEX_POINT('',#59562);
#16517=VERTEX_POINT('',#59564);
#16518=VERTEX_POINT('',#59571);
#16519=VERTEX_POINT('',#59604);
#16520=VERTEX_POINT('',#59605);
#16521=VERTEX_POINT('',#59638);
#16522=VERTEX_POINT('',#59640);
#16523=VERTEX_POINT('',#59645);
#16524=VERTEX_POINT('',#59650);
#16525=VERTEX_POINT('',#59652);
#16526=VERTEX_POINT('',#59659);
#16527=VERTEX_POINT('',#59694);
#16528=VERTEX_POINT('',#59695);
#16529=VERTEX_POINT('',#59728);
#16530=VERTEX_POINT('',#59730);
#16531=VERTEX_POINT('',#59735);
#16532=VERTEX_POINT('',#59740);
#16533=VERTEX_POINT('',#59742);
#16534=VERTEX_POINT('',#59749);
#16535=VERTEX_POINT('',#59788);
#16536=VERTEX_POINT('',#59789);
#16537=VERTEX_POINT('',#59822);
#16538=VERTEX_POINT('',#59824);
#16539=VERTEX_POINT('',#59829);
#16540=VERTEX_POINT('',#59834);
#16541=VERTEX_POINT('',#59836);
#16542=VERTEX_POINT('',#59843);
#16543=VERTEX_POINT('',#59882);
#16544=VERTEX_POINT('',#59883);
#16545=VERTEX_POINT('',#59912);
#16546=VERTEX_POINT('',#59914);
#16547=VERTEX_POINT('',#59919);
#16548=VERTEX_POINT('',#59924);
#16549=VERTEX_POINT('',#59926);
#16550=VERTEX_POINT('',#59933);
#16551=VERTEX_POINT('',#59968);
#16552=VERTEX_POINT('',#59969);
#16553=VERTEX_POINT('',#59998);
#16554=VERTEX_POINT('',#60000);
#16555=VERTEX_POINT('',#60005);
#16556=VERTEX_POINT('',#60010);
#16557=VERTEX_POINT('',#60012);
#16558=VERTEX_POINT('',#60019);
#16559=VERTEX_POINT('',#60056);
#16560=VERTEX_POINT('',#60063);
#16561=VERTEX_POINT('',#60067);
#16562=VERTEX_POINT('',#60070);
#16563=VERTEX_POINT('',#60074);
#16564=VERTEX_POINT('',#60078);
#16565=VERTEX_POINT('',#60084);
#16566=VERTEX_POINT('',#60086);
#16567=VERTEX_POINT('',#60090);
#16568=VERTEX_POINT('',#60094);
#16569=VERTEX_POINT('',#60098);
#16570=VERTEX_POINT('',#60101);
#16571=VERTEX_POINT('',#60105);
#16572=VERTEX_POINT('',#60109);
#16573=VERTEX_POINT('',#60115);
#16574=VERTEX_POINT('',#60116);
#16575=VERTEX_POINT('',#60119);
#16576=VERTEX_POINT('',#60123);
#16577=VERTEX_POINT('',#60126);
#16578=VERTEX_POINT('',#60130);
#16579=VERTEX_POINT('',#60132);
#16580=VERTEX_POINT('',#60134);
#16581=VERTEX_POINT('',#60138);
#16582=VERTEX_POINT('',#60142);
#16583=VERTEX_POINT('',#60145);
#16584=VERTEX_POINT('',#60146);
#16585=VERTEX_POINT('',#60175);
#16586=VERTEX_POINT('',#60177);
#16587=VERTEX_POINT('',#60182);
#16588=VERTEX_POINT('',#60187);
#16589=VERTEX_POINT('',#60189);
#16590=VERTEX_POINT('',#60196);
#16591=VERTEX_POINT('',#60229);
#16592=VERTEX_POINT('',#60230);
#16593=VERTEX_POINT('',#60261);
#16594=VERTEX_POINT('',#60263);
#16595=VERTEX_POINT('',#60268);
#16596=VERTEX_POINT('',#60273);
#16597=VERTEX_POINT('',#60275);
#16598=VERTEX_POINT('',#60282);
#16599=VERTEX_POINT('',#60319);
#16600=VERTEX_POINT('',#60320);
#16601=VERTEX_POINT('',#60351);
#16602=VERTEX_POINT('',#60353);
#16603=VERTEX_POINT('',#60358);
#16604=VERTEX_POINT('',#60363);
#16605=VERTEX_POINT('',#60365);
#16606=VERTEX_POINT('',#60372);
#16607=VERTEX_POINT('',#60409);
#16608=VERTEX_POINT('',#60410);
#16609=VERTEX_POINT('',#60439);
#16610=VERTEX_POINT('',#60441);
#16611=VERTEX_POINT('',#60446);
#16612=VERTEX_POINT('',#60451);
#16613=VERTEX_POINT('',#60453);
#16614=VERTEX_POINT('',#60460);
#16615=VERTEX_POINT('',#60493);
#16616=VERTEX_POINT('',#60494);
#16617=VERTEX_POINT('',#60523);
#16618=VERTEX_POINT('',#60525);
#16619=VERTEX_POINT('',#60530);
#16620=VERTEX_POINT('',#60535);
#16621=VERTEX_POINT('',#60537);
#16622=VERTEX_POINT('',#60544);
#16623=VERTEX_POINT('',#60581);
#16624=VERTEX_POINT('',#60582);
#16625=VERTEX_POINT('',#60611);
#16626=VERTEX_POINT('',#60613);
#16627=VERTEX_POINT('',#60618);
#16628=VERTEX_POINT('',#60623);
#16629=VERTEX_POINT('',#60625);
#16630=VERTEX_POINT('',#60632);
#16631=VERTEX_POINT('',#60665);
#16632=VERTEX_POINT('',#60666);
#16633=VERTEX_POINT('',#60697);
#16634=VERTEX_POINT('',#60699);
#16635=VERTEX_POINT('',#60704);
#16636=VERTEX_POINT('',#60709);
#16637=VERTEX_POINT('',#60711);
#16638=VERTEX_POINT('',#60718);
#16639=VERTEX_POINT('',#60755);
#16640=VERTEX_POINT('',#60756);
#16641=VERTEX_POINT('',#60787);
#16642=VERTEX_POINT('',#60789);
#16643=VERTEX_POINT('',#60794);
#16644=VERTEX_POINT('',#60799);
#16645=VERTEX_POINT('',#60801);
#16646=VERTEX_POINT('',#60808);
#16647=VERTEX_POINT('',#60845);
#16648=VERTEX_POINT('',#60846);
#16649=VERTEX_POINT('',#60875);
#16650=VERTEX_POINT('',#60877);
#16651=VERTEX_POINT('',#60882);
#16652=VERTEX_POINT('',#60887);
#16653=VERTEX_POINT('',#60889);
#16654=VERTEX_POINT('',#60896);
#16655=VERTEX_POINT('',#60929);
#16656=VERTEX_POINT('',#60930);
#16657=VERTEX_POINT('',#60947);
#16658=VERTEX_POINT('',#60949);
#16659=VERTEX_POINT('',#60952);
#16660=VERTEX_POINT('',#60971);
#16661=VERTEX_POINT('',#60976);
#16662=VERTEX_POINT('',#60978);
#16663=VERTEX_POINT('',#60985);
#16664=VERTEX_POINT('',#60988);
#16665=VERTEX_POINT('',#61027);
#16666=VERTEX_POINT('',#61028);
#16667=VERTEX_POINT('',#61057);
#16668=VERTEX_POINT('',#61059);
#16669=VERTEX_POINT('',#61064);
#16670=VERTEX_POINT('',#61069);
#16671=VERTEX_POINT('',#61071);
#16672=VERTEX_POINT('',#61078);
#16673=VERTEX_POINT('',#61111);
#16674=VERTEX_POINT('',#61112);
#16675=VERTEX_POINT('',#61143);
#16676=VERTEX_POINT('',#61145);
#16677=VERTEX_POINT('',#61150);
#16678=VERTEX_POINT('',#61155);
#16679=VERTEX_POINT('',#61157);
#16680=VERTEX_POINT('',#61164);
#16681=VERTEX_POINT('',#61201);
#16682=VERTEX_POINT('',#61202);
#16683=VERTEX_POINT('',#61233);
#16684=VERTEX_POINT('',#61235);
#16685=VERTEX_POINT('',#61240);
#16686=VERTEX_POINT('',#61245);
#16687=VERTEX_POINT('',#61247);
#16688=VERTEX_POINT('',#61254);
#16689=VERTEX_POINT('',#61291);
#16690=VERTEX_POINT('',#61292);
#16691=VERTEX_POINT('',#61321);
#16692=VERTEX_POINT('',#61323);
#16693=VERTEX_POINT('',#61328);
#16694=VERTEX_POINT('',#61333);
#16695=VERTEX_POINT('',#61335);
#16696=VERTEX_POINT('',#61342);
#16697=VERTEX_POINT('',#61375);
#16698=VERTEX_POINT('',#61376);
#16699=VERTEX_POINT('',#61405);
#16700=VERTEX_POINT('',#61407);
#16701=VERTEX_POINT('',#61412);
#16702=VERTEX_POINT('',#61417);
#16703=VERTEX_POINT('',#61419);
#16704=VERTEX_POINT('',#61426);
#16705=VERTEX_POINT('',#61463);
#16706=VERTEX_POINT('',#61464);
#16707=VERTEX_POINT('',#61493);
#16708=VERTEX_POINT('',#61495);
#16709=VERTEX_POINT('',#61500);
#16710=VERTEX_POINT('',#61505);
#16711=VERTEX_POINT('',#61507);
#16712=VERTEX_POINT('',#61514);
#16713=VERTEX_POINT('',#61547);
#16714=VERTEX_POINT('',#61548);
#16715=VERTEX_POINT('',#61579);
#16716=VERTEX_POINT('',#61581);
#16717=VERTEX_POINT('',#61586);
#16718=VERTEX_POINT('',#61591);
#16719=VERTEX_POINT('',#61593);
#16720=VERTEX_POINT('',#61600);
#16721=VERTEX_POINT('',#61637);
#16722=VERTEX_POINT('',#61638);
#16723=VERTEX_POINT('',#61669);
#16724=VERTEX_POINT('',#61671);
#16725=VERTEX_POINT('',#61676);
#16726=VERTEX_POINT('',#61681);
#16727=VERTEX_POINT('',#61683);
#16728=VERTEX_POINT('',#61690);
#16729=VERTEX_POINT('',#61727);
#16730=VERTEX_POINT('',#61728);
#16731=VERTEX_POINT('',#61757);
#16732=VERTEX_POINT('',#61759);
#16733=VERTEX_POINT('',#61764);
#16734=VERTEX_POINT('',#61769);
#16735=VERTEX_POINT('',#61771);
#16736=VERTEX_POINT('',#61778);
#16737=VERTEX_POINT('',#61811);
#16738=VERTEX_POINT('',#61812);
#16739=VERTEX_POINT('',#61841);
#16740=VERTEX_POINT('',#61843);
#16741=VERTEX_POINT('',#61848);
#16742=VERTEX_POINT('',#61853);
#16743=VERTEX_POINT('',#61855);
#16744=VERTEX_POINT('',#61862);
#16745=VERTEX_POINT('',#61899);
#16746=VERTEX_POINT('',#61906);
#16747=VERTEX_POINT('',#61910);
#16748=VERTEX_POINT('',#61913);
#16749=VERTEX_POINT('',#61917);
#16750=VERTEX_POINT('',#61921);
#16751=VERTEX_POINT('',#61927);
#16752=VERTEX_POINT('',#61928);
#16753=VERTEX_POINT('',#61930);
#16754=VERTEX_POINT('',#61932);
#16755=VERTEX_POINT('',#61936);
#16756=VERTEX_POINT('',#61938);
#16757=VERTEX_POINT('',#61940);
#16758=VERTEX_POINT('',#61942);
#16759=VERTEX_POINT('',#61946);
#16760=VERTEX_POINT('',#61950);
#16761=VERTEX_POINT('',#61954);
#16762=VERTEX_POINT('',#61956);
#16763=VERTEX_POINT('',#61960);
#16764=VERTEX_POINT('',#61966);
#16765=VERTEX_POINT('',#61969);
#16766=VERTEX_POINT('',#61973);
#16767=VERTEX_POINT('',#61980);
#16768=VERTEX_POINT('',#61981);
#16769=VERTEX_POINT('',#61985);
#16770=VERTEX_POINT('',#61987);
#16771=VERTEX_POINT('',#61991);
#16772=VERTEX_POINT('',#61995);
#16773=VERTEX_POINT('',#61997);
#16774=VERTEX_POINT('',#62001);
#16775=VERTEX_POINT('',#62005);
#16776=VERTEX_POINT('',#62009);
#16777=VERTEX_POINT('',#62013);
#16778=VERTEX_POINT('',#62017);
#16779=VERTEX_POINT('',#62025);
#16780=VERTEX_POINT('',#62027);
#16781=VERTEX_POINT('',#62031);
#16782=VERTEX_POINT('',#62033);
#16783=VERTEX_POINT('',#62037);
#16784=VERTEX_POINT('',#62041);
#16785=VERTEX_POINT('',#62043);
#16786=VERTEX_POINT('',#62047);
#16787=VERTEX_POINT('',#62049);
#16788=VERTEX_POINT('',#62051);
#16789=VERTEX_POINT('',#62053);
#16790=VERTEX_POINT('',#62057);
#16791=VERTEX_POINT('',#62059);
#16792=VERTEX_POINT('',#62063);
#16793=VERTEX_POINT('',#62067);
#16794=VERTEX_POINT('',#62069);
#16795=VERTEX_POINT('',#62073);
#16796=VERTEX_POINT('',#62075);
#16797=VERTEX_POINT('',#62077);
#16798=VERTEX_POINT('',#62081);
#16799=VERTEX_POINT('',#62087);
#16800=VERTEX_POINT('',#62092);
#16801=VERTEX_POINT('',#62099);
#16802=VERTEX_POINT('',#62100);
#16803=VERTEX_POINT('',#62102);
#16804=VERTEX_POINT('',#62104);
#16805=VERTEX_POINT('',#62108);
#16806=VERTEX_POINT('',#62112);
#16807=VERTEX_POINT('',#62114);
#16808=VERTEX_POINT('',#62116);
#16809=VERTEX_POINT('',#62120);
#16810=VERTEX_POINT('',#62122);
#16811=VERTEX_POINT('',#62124);
#16812=VERTEX_POINT('',#62130);
#16813=VERTEX_POINT('',#62132);
#16814=VERTEX_POINT('',#62134);
#16815=VERTEX_POINT('',#62141);
#16816=VERTEX_POINT('',#62142);
#16817=VERTEX_POINT('',#62146);
#16818=VERTEX_POINT('',#62148);
#16819=VERTEX_POINT('',#62152);
#16820=VERTEX_POINT('',#62156);
#16821=VERTEX_POINT('',#62158);
#16822=VERTEX_POINT('',#62162);
#16823=VERTEX_POINT('',#62167);
#16824=VERTEX_POINT('',#62174);
#16825=VERTEX_POINT('',#62178);
#16826=VERTEX_POINT('',#62182);
#16827=VERTEX_POINT('',#62186);
#16828=VERTEX_POINT('',#62190);
#16829=VERTEX_POINT('',#62194);
#16830=VERTEX_POINT('',#62205);
#16831=VERTEX_POINT('',#62207);
#16832=VERTEX_POINT('',#62213);
#16833=VERTEX_POINT('',#62217);
#16834=VERTEX_POINT('',#62219);
#16835=VERTEX_POINT('',#62223);
#16836=VERTEX_POINT('',#62225);
#16837=VERTEX_POINT('',#62230);
#16838=VERTEX_POINT('',#62234);
#16839=VERTEX_POINT('',#62238);
#16840=VERTEX_POINT('',#62242);
#16841=VERTEX_POINT('',#62246);
#16842=VERTEX_POINT('',#62250);
#16843=VERTEX_POINT('',#62261);
#16844=VERTEX_POINT('',#62262);
#16845=VERTEX_POINT('',#62266);
#16846=VERTEX_POINT('',#62268);
#16847=VERTEX_POINT('',#62272);
#16848=VERTEX_POINT('',#62276);
#16849=VERTEX_POINT('',#62278);
#16850=VERTEX_POINT('',#62282);
#16851=VERTEX_POINT('',#62286);
#16852=VERTEX_POINT('',#62290);
#16853=VERTEX_POINT('',#62294);
#16854=VERTEX_POINT('',#62298);
#16855=VERTEX_POINT('',#62306);
#16856=VERTEX_POINT('',#62308);
#16857=VERTEX_POINT('',#62312);
#16858=VERTEX_POINT('',#62314);
#16859=VERTEX_POINT('',#62318);
#16860=VERTEX_POINT('',#62322);
#16861=VERTEX_POINT('',#62324);
#16862=VERTEX_POINT('',#62331);
#16863=VERTEX_POINT('',#62335);
#16864=VERTEX_POINT('',#62341);
#16865=VERTEX_POINT('',#62343);
#16866=VERTEX_POINT('',#62347);
#16867=VERTEX_POINT('',#62351);
#16868=VERTEX_POINT('',#62355);
#16869=VERTEX_POINT('',#62357);
#16870=VERTEX_POINT('',#62359);
#16871=VERTEX_POINT('',#62363);
#16872=VERTEX_POINT('',#62365);
#16873=VERTEX_POINT('',#62369);
#16874=VERTEX_POINT('',#62373);
#16875=VERTEX_POINT('',#62375);
#16876=VERTEX_POINT('',#62379);
#16877=VERTEX_POINT('',#62381);
#16878=VERTEX_POINT('',#62383);
#16879=VERTEX_POINT('',#62387);
#16880=VERTEX_POINT('',#62393);
#16881=VERTEX_POINT('',#62398);
#16882=VERTEX_POINT('',#62405);
#16883=VERTEX_POINT('',#62407);
#16884=VERTEX_POINT('',#62409);
#16885=VERTEX_POINT('',#62411);
#16886=VERTEX_POINT('',#62415);
#16887=VERTEX_POINT('',#62419);
#16888=VERTEX_POINT('',#62425);
#16889=VERTEX_POINT('',#62429);
#16890=VERTEX_POINT('',#62433);
#16891=VERTEX_POINT('',#62435);
#16892=VERTEX_POINT('',#62439);
#16893=VERTEX_POINT('',#62447);
#16894=VERTEX_POINT('',#62449);
#16895=VERTEX_POINT('',#62453);
#16896=VERTEX_POINT('',#62459);
#16897=VERTEX_POINT('',#62461);
#16898=VERTEX_POINT('',#62463);
#16899=VERTEX_POINT('',#62467);
#16900=VERTEX_POINT('',#62469);
#16901=VERTEX_POINT('',#62473);
#16902=VERTEX_POINT('',#62475);
#16903=VERTEX_POINT('',#62479);
#16904=VERTEX_POINT('',#62485);
#16905=VERTEX_POINT('',#62487);
#16906=VERTEX_POINT('',#62491);
#16907=VERTEX_POINT('',#62493);
#16908=VERTEX_POINT('',#62501);
#16909=VERTEX_POINT('',#62503);
#16910=VERTEX_POINT('',#62505);
#16911=VERTEX_POINT('',#62511);
#16912=VERTEX_POINT('',#62513);
#16913=VERTEX_POINT('',#62519);
#16914=VERTEX_POINT('',#62521);
#16915=VERTEX_POINT('',#62525);
#16916=VERTEX_POINT('',#62537);
#16917=VERTEX_POINT('',#62544);
#16918=VERTEX_POINT('',#62551);
#16919=VERTEX_POINT('',#62558);
#16920=VERTEX_POINT('',#62560);
#16921=VERTEX_POINT('',#62567);
#16922=VERTEX_POINT('',#62574);
#16923=VERTEX_POINT('',#62581);
#16924=VERTEX_POINT('',#62582);
#16925=VERTEX_POINT('',#62584);
#16926=VERTEX_POINT('',#62586);
#16927=VERTEX_POINT('',#62590);
#16928=VERTEX_POINT('',#62602);
#16929=VERTEX_POINT('',#62609);
#16930=VERTEX_POINT('',#62611);
#16931=VERTEX_POINT('',#62625);
#16932=VERTEX_POINT('',#62632);
#16933=VERTEX_POINT('',#62634);
#16934=VERTEX_POINT('',#62636);
#16935=VERTEX_POINT('',#62638);
#16936=VERTEX_POINT('',#62640);
#16937=VERTEX_POINT('',#62642);
#16938=VERTEX_POINT('',#62644);
#16939=VERTEX_POINT('',#62646);
#16940=VERTEX_POINT('',#62648);
#16941=VERTEX_POINT('',#62653);
#16942=VERTEX_POINT('',#62658);
#16943=VERTEX_POINT('',#62664);
#16944=VERTEX_POINT('',#62666);
#16945=VERTEX_POINT('',#62672);
#16946=VERTEX_POINT('',#62674);
#16947=VERTEX_POINT('',#62682);
#16948=VERTEX_POINT('',#62686);
#16949=VERTEX_POINT('',#62690);
#16950=VERTEX_POINT('',#62694);
#16951=VERTEX_POINT('',#62703);
#16952=VERTEX_POINT('',#62705);
#16953=VERTEX_POINT('',#62710);
#16954=VERTEX_POINT('',#62716);
#16955=VERTEX_POINT('',#62720);
#16956=VERTEX_POINT('',#62724);
#16957=VERTEX_POINT('',#62731);
#16958=VERTEX_POINT('',#62738);
#16959=VERTEX_POINT('',#62745);
#16960=VERTEX_POINT('',#62749);
#16961=VERTEX_POINT('',#62755);
#16962=VERTEX_POINT('',#62756);
#16963=VERTEX_POINT('',#62765);
#16964=VERTEX_POINT('',#62780);
#16965=VERTEX_POINT('',#62784);
#16966=VERTEX_POINT('',#62789);
#16967=VERTEX_POINT('',#62793);
#16968=VERTEX_POINT('',#62797);
#16969=VERTEX_POINT('',#62801);
#16970=VERTEX_POINT('',#62811);
#16971=VERTEX_POINT('',#62829);
#16972=VERTEX_POINT('',#62830);
#16973=VERTEX_POINT('',#62837);
#16974=VERTEX_POINT('',#62839);
#16975=VERTEX_POINT('',#62841);
#16976=VERTEX_POINT('',#62866);
#16977=VERTEX_POINT('',#62868);
#16978=VERTEX_POINT('',#62870);
#16979=VERTEX_POINT('',#62872);
#16980=VERTEX_POINT('',#62874);
#16981=VERTEX_POINT('',#62876);
#16982=VERTEX_POINT('',#62878);
#16983=VERTEX_POINT('',#62880);
#16984=VERTEX_POINT('',#62882);
#16985=VERTEX_POINT('',#62886);
#16986=VERTEX_POINT('',#62890);
#16987=VERTEX_POINT('',#62892);
#16988=VERTEX_POINT('',#62896);
#16989=VERTEX_POINT('',#62901);
#16990=VERTEX_POINT('',#62903);
#16991=VERTEX_POINT('',#62912);
#16992=VERTEX_POINT('',#62917);
#16993=VERTEX_POINT('',#62921);
#16994=VERTEX_POINT('',#62922);
#16995=VERTEX_POINT('',#62924);
#16996=VERTEX_POINT('',#62931);
#16997=VERTEX_POINT('',#62933);
#16998=VERTEX_POINT('',#62937);
#16999=VERTEX_POINT('',#62942);
#17000=VERTEX_POINT('',#62944);
#17001=VERTEX_POINT('',#62963);
#17002=VERTEX_POINT('',#62992);
#17003=VERTEX_POINT('',#62993);
#17004=VERTEX_POINT('',#62996);
#17005=VERTEX_POINT('',#62998);
#17006=VERTEX_POINT('',#63002);
#17007=VERTEX_POINT('',#63004);
#17008=VERTEX_POINT('',#63008);
#17009=VERTEX_POINT('',#63012);
#17010=VERTEX_POINT('',#63014);
#17011=VERTEX_POINT('',#63018);
#17012=VERTEX_POINT('',#63020);
#17013=VERTEX_POINT('',#63024);
#17014=VERTEX_POINT('',#63026);
#17015=VERTEX_POINT('',#63030);
#17016=VERTEX_POINT('',#63032);
#17017=VERTEX_POINT('',#63036);
#17018=VERTEX_POINT('',#63038);
#17019=VERTEX_POINT('',#63042);
#17020=VERTEX_POINT('',#63046);
#17021=VERTEX_POINT('',#63048);
#17022=VERTEX_POINT('',#63051);
#17023=VERTEX_POINT('',#63055);
#17024=VERTEX_POINT('',#63059);
#17025=VERTEX_POINT('',#63062);
#17026=VERTEX_POINT('',#63069);
#17027=VERTEX_POINT('',#63072);
#17028=VERTEX_POINT('',#63076);
#17029=VERTEX_POINT('',#63080);
#17030=VERTEX_POINT('',#63084);
#17031=VERTEX_POINT('',#63088);
#17032=VERTEX_POINT('',#63095);
#17033=VERTEX_POINT('',#63096);
#17034=VERTEX_POINT('',#63098);
#17035=VERTEX_POINT('',#63115);
#17036=VERTEX_POINT('',#63128);
#17037=VERTEX_POINT('',#63129);
#17038=VERTEX_POINT('',#63212);
#17039=VERTEX_POINT('',#63213);
#17040=VERTEX_POINT('',#63302);
#17041=VERTEX_POINT('',#63303);
#17042=VERTEX_POINT('',#63392);
#17043=VERTEX_POINT('',#63393);
#17044=VERTEX_POINT('',#63476);
#17045=VERTEX_POINT('',#63477);
#17046=VERTEX_POINT('',#63566);
#17047=VERTEX_POINT('',#63567);
#17048=VERTEX_POINT('',#63650);
#17049=VERTEX_POINT('',#63651);
#17050=VERTEX_POINT('',#63737);
#17051=VERTEX_POINT('',#63738);
#17052=VERTEX_POINT('',#63827);
#17053=VERTEX_POINT('',#63828);
#17054=VERTEX_POINT('',#63911);
#17055=VERTEX_POINT('',#63912);
#17056=VERTEX_POINT('',#64001);
#17057=VERTEX_POINT('',#64002);
#17058=VERTEX_POINT('',#64091);
#17059=VERTEX_POINT('',#64092);
#17060=VERTEX_POINT('',#64175);
#17061=VERTEX_POINT('',#64176);
#17062=VERTEX_POINT('',#64265);
#17063=VERTEX_POINT('',#64266);
#17064=VERTEX_POINT('',#64352);
#17065=VERTEX_POINT('',#64353);
#17066=VERTEX_POINT('',#64439);
#17067=VERTEX_POINT('',#64440);
#17068=VERTEX_POINT('',#64529);
#17069=VERTEX_POINT('',#64530);
#17070=VERTEX_POINT('',#64613);
#17071=VERTEX_POINT('',#64614);
#17072=VERTEX_POINT('',#64703);
#17073=VERTEX_POINT('',#64704);
#17074=VERTEX_POINT('',#64793);
#17075=VERTEX_POINT('',#64794);
#17076=VERTEX_POINT('',#64877);
#17077=VERTEX_POINT('',#64878);
#17078=VERTEX_POINT('',#64967);
#17079=VERTEX_POINT('',#64968);
#17080=VERTEX_POINT('',#65054);
#17081=VERTEX_POINT('',#65055);
#17082=VERTEX_POINT('',#65141);
#17083=VERTEX_POINT('',#65142);
#17084=VERTEX_POINT('',#65231);
#17085=VERTEX_POINT('',#65232);
#17086=VERTEX_POINT('',#65315);
#17087=VERTEX_POINT('',#65316);
#17088=VERTEX_POINT('',#65405);
#17089=VERTEX_POINT('',#65406);
#17090=VERTEX_POINT('',#65495);
#17091=VERTEX_POINT('',#65496);
#17092=VERTEX_POINT('',#65579);
#17093=VERTEX_POINT('',#65580);
#17094=VERTEX_POINT('',#65582);
#17095=VERTEX_POINT('',#65589);
#17096=VERTEX_POINT('',#65590);
#17097=VERTEX_POINT('',#65608);
#17098=VERTEX_POINT('',#65625);
#17099=VERTEX_POINT('',#65626);
#17100=VERTEX_POINT('',#65662);
#17101=VERTEX_POINT('',#65663);
#17102=VERTEX_POINT('',#65700);
#17103=VERTEX_POINT('',#65701);
#17104=VERTEX_POINT('',#65737);
#17105=VERTEX_POINT('',#65738);
#17106=VERTEX_POINT('',#65774);
#17107=VERTEX_POINT('',#65775);
#17108=VERTEX_POINT('',#65812);
#17109=VERTEX_POINT('',#65813);
#17110=VERTEX_POINT('',#65848);
#17111=VERTEX_POINT('',#65849);
#17112=VERTEX_POINT('',#65886);
#17113=VERTEX_POINT('',#65887);
#17114=VERTEX_POINT('',#65923);
#17115=VERTEX_POINT('',#65924);
#17116=VERTEX_POINT('',#65960);
#17117=VERTEX_POINT('',#65961);
#17118=VERTEX_POINT('',#65998);
#17119=VERTEX_POINT('',#65999);
#17120=VERTEX_POINT('',#66035);
#17121=VERTEX_POINT('',#66036);
#17122=VERTEX_POINT('',#66072);
#17123=VERTEX_POINT('',#66073);
#17124=VERTEX_POINT('',#66110);
#17125=VERTEX_POINT('',#66111);
#17126=VERTEX_POINT('',#66146);
#17127=VERTEX_POINT('',#66147);
#17128=VERTEX_POINT('',#66184);
#17129=VERTEX_POINT('',#66185);
#17130=VERTEX_POINT('',#66221);
#17131=VERTEX_POINT('',#66222);
#17132=VERTEX_POINT('',#66258);
#17133=VERTEX_POINT('',#66259);
#17134=VERTEX_POINT('',#66296);
#17135=VERTEX_POINT('',#66297);
#17136=VERTEX_POINT('',#66333);
#17137=VERTEX_POINT('',#66334);
#17138=VERTEX_POINT('',#66370);
#17139=VERTEX_POINT('',#66371);
#17140=VERTEX_POINT('',#66408);
#17141=VERTEX_POINT('',#66409);
#17142=VERTEX_POINT('',#66445);
#17143=VERTEX_POINT('',#66446);
#17144=VERTEX_POINT('',#66482);
#17145=VERTEX_POINT('',#66483);
#17146=VERTEX_POINT('',#66519);
#17147=VERTEX_POINT('',#66520);
#17148=VERTEX_POINT('',#66556);
#17149=VERTEX_POINT('',#66557);
#17150=VERTEX_POINT('',#66594);
#17151=VERTEX_POINT('',#66595);
#17152=VERTEX_POINT('',#66631);
#17153=VERTEX_POINT('',#66633);
#17154=VERTEX_POINT('',#66635);
#17155=VERTEX_POINT('',#66639);
#17156=VERTEX_POINT('',#66641);
#17157=VERTEX_POINT('',#66643);
#17158=VERTEX_POINT('',#66648);
#17159=VERTEX_POINT('',#66649);
#17160=VERTEX_POINT('',#66653);
#17161=VERTEX_POINT('',#66655);
#17162=VERTEX_POINT('',#66659);
#17163=VERTEX_POINT('',#66661);
#17164=VERTEX_POINT('',#66666);
#17165=VERTEX_POINT('',#66669);
#17166=VERTEX_POINT('',#66671);
#17167=VERTEX_POINT('',#66673);
#17168=VERTEX_POINT('',#66677);
#17169=VERTEX_POINT('',#66683);
#17170=VERTEX_POINT('',#66685);
#17171=VERTEX_POINT('',#66689);
#17172=VERTEX_POINT('',#66693);
#17173=VERTEX_POINT('',#66695);
#17174=VERTEX_POINT('',#66703);
#17175=VERTEX_POINT('',#68435);
#17176=VERTEX_POINT('',#68560);
#17177=VERTEX_POINT('',#68563);
#17178=VERTEX_POINT('',#70184);
#17179=VERTEX_POINT('',#70185);
#17180=VERTEX_POINT('',#70187);
#17181=VERTEX_POINT('',#70189);
#17182=VERTEX_POINT('',#70193);
#17183=VERTEX_POINT('',#70197);
#17184=VERTEX_POINT('',#70203);
#17185=VERTEX_POINT('',#70204);
#17186=VERTEX_POINT('',#70206);
#17187=VERTEX_POINT('',#70208);
#17188=VERTEX_POINT('',#70212);
#17189=VERTEX_POINT('',#70216);
#17190=VERTEX_POINT('',#70222);
#17191=VERTEX_POINT('',#70223);
#17192=VERTEX_POINT('',#70225);
#17193=VERTEX_POINT('',#70227);
#17194=VERTEX_POINT('',#70231);
#17195=VERTEX_POINT('',#70235);
#17196=VERTEX_POINT('',#70241);
#17197=VERTEX_POINT('',#70242);
#17198=VERTEX_POINT('',#70244);
#17199=VERTEX_POINT('',#70246);
#17200=VERTEX_POINT('',#70250);
#17201=VERTEX_POINT('',#70254);
#17202=VERTEX_POINT('',#70260);
#17203=VERTEX_POINT('',#70261);
#17204=VERTEX_POINT('',#70263);
#17205=VERTEX_POINT('',#70265);
#17206=VERTEX_POINT('',#70269);
#17207=VERTEX_POINT('',#70273);
#17208=VERTEX_POINT('',#70279);
#17209=VERTEX_POINT('',#70280);
#17210=VERTEX_POINT('',#70282);
#17211=VERTEX_POINT('',#70284);
#17212=VERTEX_POINT('',#70288);
#17213=VERTEX_POINT('',#70292);
#17214=VERTEX_POINT('',#70298);
#17215=VERTEX_POINT('',#70299);
#17216=VERTEX_POINT('',#70301);
#17217=VERTEX_POINT('',#70303);
#17218=VERTEX_POINT('',#70307);
#17219=VERTEX_POINT('',#70311);
#17220=VERTEX_POINT('',#70317);
#17221=VERTEX_POINT('',#70318);
#17222=VERTEX_POINT('',#70320);
#17223=VERTEX_POINT('',#70322);
#17224=VERTEX_POINT('',#70326);
#17225=VERTEX_POINT('',#70330);
#17226=VERTEX_POINT('',#70336);
#17227=VERTEX_POINT('',#70337);
#17228=VERTEX_POINT('',#70339);
#17229=VERTEX_POINT('',#70341);
#17230=VERTEX_POINT('',#70345);
#17231=VERTEX_POINT('',#70349);
#17232=VERTEX_POINT('',#70355);
#17233=VERTEX_POINT('',#70356);
#17234=VERTEX_POINT('',#70358);
#17235=VERTEX_POINT('',#70360);
#17236=VERTEX_POINT('',#70364);
#17237=VERTEX_POINT('',#70368);
#17238=VERTEX_POINT('',#70374);
#17239=VERTEX_POINT('',#70375);
#17240=VERTEX_POINT('',#70377);
#17241=VERTEX_POINT('',#70379);
#17242=VERTEX_POINT('',#70383);
#17243=VERTEX_POINT('',#70387);
#17244=VERTEX_POINT('',#70393);
#17245=VERTEX_POINT('',#70394);
#17246=VERTEX_POINT('',#70396);
#17247=VERTEX_POINT('',#70398);
#17248=VERTEX_POINT('',#70402);
#17249=VERTEX_POINT('',#70406);
#17250=VERTEX_POINT('',#70412);
#17251=VERTEX_POINT('',#70413);
#17252=VERTEX_POINT('',#70415);
#17253=VERTEX_POINT('',#70417);
#17254=VERTEX_POINT('',#70421);
#17255=VERTEX_POINT('',#70425);
#17256=VERTEX_POINT('',#70431);
#17257=VERTEX_POINT('',#70432);
#17258=VERTEX_POINT('',#70434);
#17259=VERTEX_POINT('',#70436);
#17260=VERTEX_POINT('',#70440);
#17261=VERTEX_POINT('',#70444);
#17262=VERTEX_POINT('',#70450);
#17263=VERTEX_POINT('',#70451);
#17264=VERTEX_POINT('',#70453);
#17265=VERTEX_POINT('',#70455);
#17266=VERTEX_POINT('',#70459);
#17267=VERTEX_POINT('',#70463);
#17268=VERTEX_POINT('',#70469);
#17269=VERTEX_POINT('',#70470);
#17270=VERTEX_POINT('',#70472);
#17271=VERTEX_POINT('',#70474);
#17272=VERTEX_POINT('',#70478);
#17273=VERTEX_POINT('',#70482);
#17274=VERTEX_POINT('',#70488);
#17275=VERTEX_POINT('',#70489);
#17276=VERTEX_POINT('',#70491);
#17277=VERTEX_POINT('',#70493);
#17278=VERTEX_POINT('',#70497);
#17279=VERTEX_POINT('',#70501);
#17280=VERTEX_POINT('',#70507);
#17281=VERTEX_POINT('',#70508);
#17282=VERTEX_POINT('',#70510);
#17283=VERTEX_POINT('',#70512);
#17284=VERTEX_POINT('',#70516);
#17285=VERTEX_POINT('',#70518);
#17286=VERTEX_POINT('',#70522);
#17287=VERTEX_POINT('',#70526);
#17288=VERTEX_POINT('',#70530);
#17289=VERTEX_POINT('',#70531);
#17290=VERTEX_POINT('',#70533);
#17291=VERTEX_POINT('',#70535);
#17292=VERTEX_POINT('',#70539);
#17293=VERTEX_POINT('',#70543);
#17294=VERTEX_POINT('',#70549);
#17295=VERTEX_POINT('',#70550);
#17296=VERTEX_POINT('',#70552);
#17297=VERTEX_POINT('',#70554);
#17298=VERTEX_POINT('',#70558);
#17299=VERTEX_POINT('',#70562);
#17300=VERTEX_POINT('',#70568);
#17301=VERTEX_POINT('',#70569);
#17302=VERTEX_POINT('',#70571);
#17303=VERTEX_POINT('',#70573);
#17304=VERTEX_POINT('',#70577);
#17305=VERTEX_POINT('',#70581);
#17306=VERTEX_POINT('',#70587);
#17307=VERTEX_POINT('',#70588);
#17308=VERTEX_POINT('',#70590);
#17309=VERTEX_POINT('',#70592);
#17310=VERTEX_POINT('',#70596);
#17311=VERTEX_POINT('',#70600);
#17312=VERTEX_POINT('',#70606);
#17313=VERTEX_POINT('',#70607);
#17314=VERTEX_POINT('',#70609);
#17315=VERTEX_POINT('',#70611);
#17316=VERTEX_POINT('',#70615);
#17317=VERTEX_POINT('',#70619);
#17318=VERTEX_POINT('',#70625);
#17319=VERTEX_POINT('',#70626);
#17320=VERTEX_POINT('',#70628);
#17321=VERTEX_POINT('',#70630);
#17322=VERTEX_POINT('',#70634);
#17323=VERTEX_POINT('',#70638);
#17324=VERTEX_POINT('',#70644);
#17325=VERTEX_POINT('',#70645);
#17326=VERTEX_POINT('',#70647);
#17327=VERTEX_POINT('',#70649);
#17328=VERTEX_POINT('',#70653);
#17329=VERTEX_POINT('',#70657);
#17330=VERTEX_POINT('',#70663);
#17331=VERTEX_POINT('',#70664);
#17332=VERTEX_POINT('',#70666);
#17333=VERTEX_POINT('',#70668);
#17334=VERTEX_POINT('',#70672);
#17335=VERTEX_POINT('',#70676);
#17336=VERTEX_POINT('',#70682);
#17337=VERTEX_POINT('',#70683);
#17338=VERTEX_POINT('',#70685);
#17339=VERTEX_POINT('',#70687);
#17340=VERTEX_POINT('',#70691);
#17341=VERTEX_POINT('',#70695);
#17342=VERTEX_POINT('',#70701);
#17343=VERTEX_POINT('',#70702);
#17344=VERTEX_POINT('',#70704);
#17345=VERTEX_POINT('',#70706);
#17346=VERTEX_POINT('',#70710);
#17347=VERTEX_POINT('',#70714);
#17348=VERTEX_POINT('',#70720);
#17349=VERTEX_POINT('',#70721);
#17350=VERTEX_POINT('',#70723);
#17351=VERTEX_POINT('',#70725);
#17352=VERTEX_POINT('',#70729);
#17353=VERTEX_POINT('',#70733);
#17354=VERTEX_POINT('',#70739);
#17355=VERTEX_POINT('',#70740);
#17356=VERTEX_POINT('',#70742);
#17357=VERTEX_POINT('',#70744);
#17358=VERTEX_POINT('',#70748);
#17359=VERTEX_POINT('',#70752);
#17360=VERTEX_POINT('',#70758);
#17361=VERTEX_POINT('',#70759);
#17362=VERTEX_POINT('',#70761);
#17363=VERTEX_POINT('',#70763);
#17364=VERTEX_POINT('',#70767);
#17365=VERTEX_POINT('',#70771);
#17366=VERTEX_POINT('',#70777);
#17367=VERTEX_POINT('',#70778);
#17368=VERTEX_POINT('',#70780);
#17369=VERTEX_POINT('',#70782);
#17370=VERTEX_POINT('',#70786);
#17371=VERTEX_POINT('',#70790);
#17372=VERTEX_POINT('',#70796);
#17373=VERTEX_POINT('',#70797);
#17374=VERTEX_POINT('',#70799);
#17375=VERTEX_POINT('',#70801);
#17376=VERTEX_POINT('',#70805);
#17377=VERTEX_POINT('',#70809);
#17378=VERTEX_POINT('',#70815);
#17379=VERTEX_POINT('',#70816);
#17380=VERTEX_POINT('',#70818);
#17381=VERTEX_POINT('',#70820);
#17382=VERTEX_POINT('',#70824);
#17383=VERTEX_POINT('',#70828);
#17384=VERTEX_POINT('',#70834);
#17385=VERTEX_POINT('',#70835);
#17386=VERTEX_POINT('',#70837);
#17387=VERTEX_POINT('',#70839);
#17388=VERTEX_POINT('',#70843);
#17389=VERTEX_POINT('',#70847);
#17390=VERTEX_POINT('',#70853);
#17391=VERTEX_POINT('',#70854);
#17392=VERTEX_POINT('',#70856);
#17393=VERTEX_POINT('',#70858);
#17394=VERTEX_POINT('',#70862);
#17395=VERTEX_POINT('',#70866);
#17396=VERTEX_POINT('',#70872);
#17397=VERTEX_POINT('',#70880);
#17398=VERTEX_POINT('',#70882);
#17399=VERTEX_POINT('',#70884);
#17400=VERTEX_POINT('',#70904);
#17401=VERTEX_POINT('',#70906);
#17402=VERTEX_POINT('',#70944);
#17403=VERTEX_POINT('',#70946);
#17404=VERTEX_POINT('',#70990);
#17405=VERTEX_POINT('',#70992);
#17406=VERTEX_POINT('',#71030);
#17407=VERTEX_POINT('',#71032);
#17408=VERTEX_POINT('',#71070);
#17409=VERTEX_POINT('',#71072);
#17410=VERTEX_POINT('',#71116);
#17411=VERTEX_POINT('',#71161);
#17412=VERTEX_POINT('',#71166);
#17413=VERTEX_POINT('',#71173);
#17414=VERTEX_POINT('',#71180);
#17415=VERTEX_POINT('',#71215);
#17416=VERTEX_POINT('',#71220);
#17417=VERTEX_POINT('',#71227);
#17418=VERTEX_POINT('',#71251);
#17419=VERTEX_POINT('',#71261);
#17420=VERTEX_POINT('',#71271);
#17421=VERTEX_POINT('',#71309);
#17422=VERTEX_POINT('',#71316);
#17423=VERTEX_POINT('',#71330);
#17424=VERTEX_POINT('',#71333);
#17425=VERTEX_POINT('',#71334);
#17426=VERTEX_POINT('',#71336);
#17427=VERTEX_POINT('',#71340);
#17428=VERTEX_POINT('',#71341);
#17429=VERTEX_POINT('',#71343);
#17430=VERTEX_POINT('',#71347);
#17431=VERTEX_POINT('',#71348);
#17432=VERTEX_POINT('',#71350);
#17433=VERTEX_POINT('',#71359);
#17434=VERTEX_POINT('',#71360);
#17435=VERTEX_POINT('',#71362);
#17436=VERTEX_POINT('',#71366);
#17437=VERTEX_POINT('',#71375);
#17438=VERTEX_POINT('',#71376);
#17439=VERTEX_POINT('',#71378);
#17440=VERTEX_POINT('',#71387);
#17441=VERTEX_POINT('',#71388);
#17442=VERTEX_POINT('',#71390);
#17443=VERTEX_POINT('',#71397);
#17444=VERTEX_POINT('',#71404);
#17445=VERTEX_POINT('',#71413);
#17446=VERTEX_POINT('',#71422);
#17447=VERTEX_POINT('',#71429);
#17448=VERTEX_POINT('',#71556);
#17449=VERTEX_POINT('',#71564);
#17450=VERTEX_POINT('',#71565);
#17451=VERTEX_POINT('',#71570);
#17452=VERTEX_POINT('',#71574);
#17453=EDGE_CURVE('',#14532,#14533,#13634,.T.);
#17454=EDGE_CURVE('',#14533,#14532,#13635,.T.);
#17455=EDGE_CURVE('',#14532,#14534,#7534,.T.);
#17456=EDGE_CURVE('',#14534,#14535,#13636,.T.);
#17457=EDGE_CURVE('',#14535,#14534,#13637,.T.);
#17458=EDGE_CURVE('',#14535,#14536,#7535,.T.);
#17459=EDGE_CURVE('',#14537,#14536,#13638,.T.);
#17460=EDGE_CURVE('',#14536,#14537,#13639,.T.);
#17461=EDGE_CURVE('',#14538,#14538,#13640,.T.);
#17462=EDGE_CURVE('',#14538,#14533,#7536,.T.);
#17463=EDGE_CURVE('',#14537,#14539,#7537,.T.);
#17464=EDGE_CURVE('',#14539,#14539,#13641,.T.);
#17465=EDGE_CURVE('',#14540,#14540,#13642,.T.);
#17466=EDGE_CURVE('',#14541,#14541,#13643,.T.);
#17467=EDGE_CURVE('',#14541,#14542,#7538,.T.);
#17468=EDGE_CURVE('',#14542,#14543,#13644,.T.);
#17469=EDGE_CURVE('',#14543,#14542,#13645,.T.);
#17470=EDGE_CURVE('',#14544,#14544,#13646,.T.);
#17471=EDGE_CURVE('',#14544,#14543,#7539,.T.);
#17472=EDGE_CURVE('',#14545,#14545,#13647,.T.);
#17473=EDGE_CURVE('',#14546,#14546,#13648,.T.);
#17474=EDGE_CURVE('',#14546,#14547,#7540,.T.);
#17475=EDGE_CURVE('',#14547,#14548,#13649,.T.);
#17476=EDGE_CURVE('',#14548,#14547,#13650,.T.);
#17477=EDGE_CURVE('',#14548,#14549,#7541,.T.);
#17478=EDGE_CURVE('',#14550,#14549,#13651,.T.);
#17479=EDGE_CURVE('',#14549,#14550,#13652,.T.);
#17480=EDGE_CURVE('',#14551,#14551,#13653,.T.);
#17481=EDGE_CURVE('',#14550,#14552,#7542,.T.);
#17482=EDGE_CURVE('',#14552,#14553,#13654,.T.);
#17483=EDGE_CURVE('',#14553,#14552,#13655,.T.);
#17484=EDGE_CURVE('',#14553,#14554,#7543,.T.);
#17485=EDGE_CURVE('',#14554,#14554,#13656,.T.);
#17486=EDGE_CURVE('',#14555,#14556,#13657,.T.);
#17487=EDGE_CURVE('',#14556,#14555,#13658,.T.);
#17488=EDGE_CURVE('',#14555,#14557,#7544,.T.);
#17489=EDGE_CURVE('',#14557,#14558,#13659,.T.);
#17490=EDGE_CURVE('',#14558,#14557,#13660,.T.);
#17491=EDGE_CURVE('',#14558,#14559,#7545,.T.);
#17492=EDGE_CURVE('',#14560,#14559,#13661,.T.);
#17493=EDGE_CURVE('',#14559,#14560,#13662,.T.);
#17494=EDGE_CURVE('',#14561,#14561,#13663,.T.);
#17495=EDGE_CURVE('',#14561,#14556,#7546,.T.);
#17496=EDGE_CURVE('',#14560,#14562,#7547,.T.);
#17497=EDGE_CURVE('',#14562,#14563,#13664,.T.);
#17498=EDGE_CURVE('',#14563,#14562,#13665,.T.);
#17499=EDGE_CURVE('',#14563,#14564,#7548,.T.);
#17500=EDGE_CURVE('',#14565,#14564,#13666,.T.);
#17501=EDGE_CURVE('',#14564,#14565,#13667,.T.);
#17502=EDGE_CURVE('',#14565,#14566,#7549,.T.);
#17503=EDGE_CURVE('',#14566,#14567,#13668,.T.);
#17504=EDGE_CURVE('',#14567,#14566,#13669,.T.);
#17505=EDGE_CURVE('',#14567,#14568,#7550,.T.);
#17506=EDGE_CURVE('',#14569,#14568,#13670,.T.);
#17507=EDGE_CURVE('',#14568,#14569,#13671,.T.);
#17508=EDGE_CURVE('',#14569,#14570,#7551,.T.);
#17509=EDGE_CURVE('',#14570,#14571,#13672,.T.);
#17510=EDGE_CURVE('',#14571,#14570,#13673,.T.);
#17511=EDGE_CURVE('',#14571,#14572,#7552,.T.);
#17512=EDGE_CURVE('',#14572,#14573,#13674,.T.);
#17513=EDGE_CURVE('',#14574,#14573,#842,.F.);
#17514=EDGE_CURVE('',#14574,#14575,#7553,.T.);
#17515=EDGE_CURVE('',#14576,#14575,#843,.F.);
#17516=EDGE_CURVE('',#14576,#14577,#13675,.T.);
#17517=EDGE_CURVE('',#14577,#14578,#7554,.T.);
#17518=EDGE_CURVE('',#14578,#14578,#13676,.T.);
#17519=EDGE_CURVE('',#14577,#14579,#13677,.T.);
#17520=EDGE_CURVE('',#14580,#14579,#844,.F.);
#17521=EDGE_CURVE('',#14580,#14581,#7555,.T.);
#17522=EDGE_CURVE('',#14582,#14581,#845,.F.);
#17523=EDGE_CURVE('',#14582,#14572,#13678,.T.);
#17524=EDGE_CURVE('',#14583,#14584,#7556,.T.);
#17525=EDGE_CURVE('',#14585,#14584,#846,.F.);
#17526=EDGE_CURVE('',#14585,#14586,#13679,.T.);
#17527=EDGE_CURVE('',#14587,#14586,#847,.F.);
#17528=EDGE_CURVE('',#14587,#14588,#7557,.T.);
#17529=EDGE_CURVE('',#14589,#14588,#848,.F.);
#17530=EDGE_CURVE('',#14589,#14590,#13680,.T.);
#17531=EDGE_CURVE('',#14583,#14590,#849,.F.);
#17532=EDGE_CURVE('',#14591,#14592,#7558,.T.);
#17533=EDGE_CURVE('',#14593,#14592,#850,.F.);
#17534=EDGE_CURVE('',#14593,#14594,#13681,.T.);
#17535=EDGE_CURVE('',#14595,#14594,#851,.F.);
#17536=EDGE_CURVE('',#14595,#14596,#7559,.T.);
#17537=EDGE_CURVE('',#14597,#14596,#852,.F.);
#17538=EDGE_CURVE('',#14597,#14598,#13682,.T.);
#17539=EDGE_CURVE('',#14591,#14598,#853,.F.);
#17540=EDGE_CURVE('',#14599,#14600,#7560,.T.);
#17541=EDGE_CURVE('',#14601,#14600,#854,.F.);
#17542=EDGE_CURVE('',#14601,#14602,#13683,.T.);
#17543=EDGE_CURVE('',#14603,#14602,#855,.F.);
#17544=EDGE_CURVE('',#14603,#14604,#7561,.T.);
#17545=EDGE_CURVE('',#14605,#14604,#856,.F.);
#17546=EDGE_CURVE('',#14605,#14606,#13684,.T.);
#17547=EDGE_CURVE('',#14599,#14606,#857,.F.);
#17548=EDGE_CURVE('',#14607,#14608,#7562,.T.);
#17549=EDGE_CURVE('',#14609,#14608,#858,.F.);
#17550=EDGE_CURVE('',#14609,#14610,#13685,.T.);
#17551=EDGE_CURVE('',#14611,#14610,#859,.F.);
#17552=EDGE_CURVE('',#14611,#14612,#7563,.T.);
#17553=EDGE_CURVE('',#14613,#14612,#860,.F.);
#17554=EDGE_CURVE('',#14613,#14614,#13686,.T.);
#17555=EDGE_CURVE('',#14607,#14614,#861,.F.);
#17556=EDGE_CURVE('',#14615,#14616,#7564,.T.);
#17557=EDGE_CURVE('',#14617,#14616,#862,.F.);
#17558=EDGE_CURVE('',#14617,#14618,#13687,.T.);
#17559=EDGE_CURVE('',#14619,#14618,#863,.F.);
#17560=EDGE_CURVE('',#14619,#14620,#7565,.T.);
#17561=EDGE_CURVE('',#14621,#14620,#864,.F.);
#17562=EDGE_CURVE('',#14621,#14622,#13688,.T.);
#17563=EDGE_CURVE('',#14615,#14622,#865,.F.);
#17564=EDGE_CURVE('',#14623,#14624,#7566,.T.);
#17565=EDGE_CURVE('',#14625,#14624,#866,.F.);
#17566=EDGE_CURVE('',#14625,#14626,#13689,.T.);
#17567=EDGE_CURVE('',#14627,#14626,#867,.F.);
#17568=EDGE_CURVE('',#14627,#14628,#7567,.T.);
#17569=EDGE_CURVE('',#14629,#14628,#868,.F.);
#17570=EDGE_CURVE('',#14629,#14630,#13690,.T.);
#17571=EDGE_CURVE('',#14623,#14630,#869,.F.);
#17572=EDGE_CURVE('',#14631,#14632,#7568,.T.);
#17573=EDGE_CURVE('',#14633,#14632,#870,.F.);
#17574=EDGE_CURVE('',#14633,#14634,#13691,.T.);
#17575=EDGE_CURVE('',#14635,#14634,#871,.F.);
#17576=EDGE_CURVE('',#14635,#14636,#7569,.T.);
#17577=EDGE_CURVE('',#14637,#14636,#872,.F.);
#17578=EDGE_CURVE('',#14637,#14638,#13692,.T.);
#17579=EDGE_CURVE('',#14631,#14638,#873,.F.);
#17580=EDGE_CURVE('',#14639,#14640,#7570,.T.);
#17581=EDGE_CURVE('',#14641,#14640,#874,.F.);
#17582=EDGE_CURVE('',#14641,#14642,#13693,.T.);
#17583=EDGE_CURVE('',#14643,#14642,#875,.F.);
#17584=EDGE_CURVE('',#14643,#14644,#7571,.T.);
#17585=EDGE_CURVE('',#14645,#14644,#876,.F.);
#17586=EDGE_CURVE('',#14645,#14646,#13694,.T.);
#17587=EDGE_CURVE('',#14639,#14646,#877,.F.);
#17588=EDGE_CURVE('',#14647,#14648,#7572,.T.);
#17589=EDGE_CURVE('',#14649,#14648,#878,.F.);
#17590=EDGE_CURVE('',#14649,#14650,#13695,.T.);
#17591=EDGE_CURVE('',#14651,#14650,#879,.F.);
#17592=EDGE_CURVE('',#14651,#14652,#7573,.T.);
#17593=EDGE_CURVE('',#14653,#14652,#880,.F.);
#17594=EDGE_CURVE('',#14653,#14654,#13696,.T.);
#17595=EDGE_CURVE('',#14647,#14654,#881,.F.);
#17596=EDGE_CURVE('',#14655,#14656,#7574,.T.);
#17597=EDGE_CURVE('',#14657,#14656,#882,.F.);
#17598=EDGE_CURVE('',#14657,#14658,#13697,.T.);
#17599=EDGE_CURVE('',#14659,#14658,#883,.F.);
#17600=EDGE_CURVE('',#14659,#14660,#7575,.T.);
#17601=EDGE_CURVE('',#14661,#14660,#884,.F.);
#17602=EDGE_CURVE('',#14661,#14662,#13698,.T.);
#17603=EDGE_CURVE('',#14655,#14662,#885,.F.);
#17604=EDGE_CURVE('',#14663,#14664,#7576,.T.);
#17605=EDGE_CURVE('',#14665,#14664,#886,.F.);
#17606=EDGE_CURVE('',#14665,#14666,#13699,.T.);
#17607=EDGE_CURVE('',#14667,#14666,#887,.F.);
#17608=EDGE_CURVE('',#14667,#14668,#7577,.T.);
#17609=EDGE_CURVE('',#14669,#14668,#888,.F.);
#17610=EDGE_CURVE('',#14669,#14670,#13700,.T.);
#17611=EDGE_CURVE('',#14663,#14670,#889,.F.);
#17612=EDGE_CURVE('',#14671,#14672,#7578,.T.);
#17613=EDGE_CURVE('',#14673,#14672,#890,.F.);
#17614=EDGE_CURVE('',#14673,#14674,#13701,.T.);
#17615=EDGE_CURVE('',#14675,#14674,#891,.F.);
#17616=EDGE_CURVE('',#14675,#14676,#7579,.T.);
#17617=EDGE_CURVE('',#14677,#14676,#892,.F.);
#17618=EDGE_CURVE('',#14677,#14678,#13702,.T.);
#17619=EDGE_CURVE('',#14671,#14678,#893,.F.);
#17620=EDGE_CURVE('',#14679,#14680,#7580,.T.);
#17621=EDGE_CURVE('',#14681,#14680,#894,.F.);
#17622=EDGE_CURVE('',#14681,#14682,#13703,.T.);
#17623=EDGE_CURVE('',#14683,#14682,#895,.F.);
#17624=EDGE_CURVE('',#14683,#14684,#7581,.T.);
#17625=EDGE_CURVE('',#14685,#14684,#896,.F.);
#17626=EDGE_CURVE('',#14685,#14686,#13704,.T.);
#17627=EDGE_CURVE('',#14679,#14686,#897,.F.);
#17628=EDGE_CURVE('',#14687,#14688,#7582,.T.);
#17629=EDGE_CURVE('',#14689,#14688,#898,.F.);
#17630=EDGE_CURVE('',#14689,#14690,#13705,.T.);
#17631=EDGE_CURVE('',#14691,#14690,#899,.F.);
#17632=EDGE_CURVE('',#14691,#14692,#7583,.T.);
#17633=EDGE_CURVE('',#14693,#14692,#900,.F.);
#17634=EDGE_CURVE('',#14693,#14694,#13706,.T.);
#17635=EDGE_CURVE('',#14687,#14694,#901,.F.);
#17636=EDGE_CURVE('',#14695,#14696,#7584,.T.);
#17637=EDGE_CURVE('',#14697,#14696,#902,.F.);
#17638=EDGE_CURVE('',#14697,#14698,#13707,.T.);
#17639=EDGE_CURVE('',#14699,#14698,#903,.F.);
#17640=EDGE_CURVE('',#14699,#14700,#7585,.T.);
#17641=EDGE_CURVE('',#14701,#14700,#904,.F.);
#17642=EDGE_CURVE('',#14701,#14702,#13708,.T.);
#17643=EDGE_CURVE('',#14695,#14702,#905,.F.);
#17644=EDGE_CURVE('',#14703,#14704,#7586,.T.);
#17645=EDGE_CURVE('',#14705,#14704,#906,.F.);
#17646=EDGE_CURVE('',#14705,#14706,#13709,.T.);
#17647=EDGE_CURVE('',#14707,#14706,#907,.F.);
#17648=EDGE_CURVE('',#14707,#14708,#7587,.T.);
#17649=EDGE_CURVE('',#14709,#14708,#908,.F.);
#17650=EDGE_CURVE('',#14709,#14710,#13710,.T.);
#17651=EDGE_CURVE('',#14703,#14710,#909,.F.);
#17652=EDGE_CURVE('',#14711,#14712,#7588,.T.);
#17653=EDGE_CURVE('',#14713,#14712,#910,.F.);
#17654=EDGE_CURVE('',#14713,#14714,#13711,.T.);
#17655=EDGE_CURVE('',#14715,#14714,#911,.F.);
#17656=EDGE_CURVE('',#14715,#14716,#7589,.T.);
#17657=EDGE_CURVE('',#14717,#14716,#912,.F.);
#17658=EDGE_CURVE('',#14717,#14718,#13712,.T.);
#17659=EDGE_CURVE('',#14711,#14718,#913,.F.);
#17660=EDGE_CURVE('',#14719,#14720,#7590,.T.);
#17661=EDGE_CURVE('',#14721,#14720,#914,.F.);
#17662=EDGE_CURVE('',#14721,#14722,#13713,.T.);
#17663=EDGE_CURVE('',#14723,#14722,#915,.F.);
#17664=EDGE_CURVE('',#14723,#14724,#7591,.T.);
#17665=EDGE_CURVE('',#14725,#14724,#916,.F.);
#17666=EDGE_CURVE('',#14725,#14726,#13714,.T.);
#17667=EDGE_CURVE('',#14719,#14726,#917,.F.);
#17668=EDGE_CURVE('',#14727,#14728,#7592,.T.);
#17669=EDGE_CURVE('',#14729,#14728,#918,.F.);
#17670=EDGE_CURVE('',#14729,#14730,#13715,.T.);
#17671=EDGE_CURVE('',#14731,#14730,#919,.F.);
#17672=EDGE_CURVE('',#14731,#14732,#7593,.T.);
#17673=EDGE_CURVE('',#14733,#14732,#920,.F.);
#17674=EDGE_CURVE('',#14733,#14734,#13716,.T.);
#17675=EDGE_CURVE('',#14727,#14734,#921,.F.);
#17676=EDGE_CURVE('',#14735,#14736,#7594,.T.);
#17677=EDGE_CURVE('',#14737,#14736,#922,.F.);
#17678=EDGE_CURVE('',#14737,#14738,#13717,.T.);
#17679=EDGE_CURVE('',#14739,#14738,#923,.F.);
#17680=EDGE_CURVE('',#14739,#14740,#7595,.T.);
#17681=EDGE_CURVE('',#14741,#14740,#924,.F.);
#17682=EDGE_CURVE('',#14741,#14742,#13718,.T.);
#17683=EDGE_CURVE('',#14735,#14742,#925,.F.);
#17684=EDGE_CURVE('',#14743,#14744,#7596,.T.);
#17685=EDGE_CURVE('',#14745,#14744,#926,.F.);
#17686=EDGE_CURVE('',#14745,#14746,#13719,.T.);
#17687=EDGE_CURVE('',#14747,#14746,#927,.F.);
#17688=EDGE_CURVE('',#14747,#14748,#7597,.T.);
#17689=EDGE_CURVE('',#14749,#14748,#928,.F.);
#17690=EDGE_CURVE('',#14749,#14750,#13720,.T.);
#17691=EDGE_CURVE('',#14743,#14750,#929,.F.);
#17692=EDGE_CURVE('',#14751,#14752,#7598,.T.);
#17693=EDGE_CURVE('',#14753,#14752,#930,.F.);
#17694=EDGE_CURVE('',#14753,#14754,#13721,.T.);
#17695=EDGE_CURVE('',#14755,#14754,#931,.F.);
#17696=EDGE_CURVE('',#14755,#14756,#7599,.T.);
#17697=EDGE_CURVE('',#14757,#14756,#932,.F.);
#17698=EDGE_CURVE('',#14757,#14758,#13722,.T.);
#17699=EDGE_CURVE('',#14751,#14758,#933,.F.);
#17700=EDGE_CURVE('',#14759,#14760,#7600,.T.);
#17701=EDGE_CURVE('',#14761,#14760,#934,.F.);
#17702=EDGE_CURVE('',#14761,#14762,#13723,.T.);
#17703=EDGE_CURVE('',#14763,#14762,#935,.F.);
#17704=EDGE_CURVE('',#14763,#14764,#7601,.T.);
#17705=EDGE_CURVE('',#14765,#14764,#936,.F.);
#17706=EDGE_CURVE('',#14765,#14766,#13724,.T.);
#17707=EDGE_CURVE('',#14759,#14766,#937,.F.);
#17708=EDGE_CURVE('',#14767,#14768,#7602,.T.);
#17709=EDGE_CURVE('',#14769,#14768,#938,.F.);
#17710=EDGE_CURVE('',#14769,#14770,#13725,.T.);
#17711=EDGE_CURVE('',#14771,#14770,#939,.F.);
#17712=EDGE_CURVE('',#14771,#14772,#7603,.T.);
#17713=EDGE_CURVE('',#14773,#14772,#940,.F.);
#17714=EDGE_CURVE('',#14773,#14774,#13726,.T.);
#17715=EDGE_CURVE('',#14767,#14774,#941,.F.);
#17716=EDGE_CURVE('',#14775,#14776,#7604,.T.);
#17717=EDGE_CURVE('',#14777,#14776,#942,.F.);
#17718=EDGE_CURVE('',#14777,#14778,#13727,.T.);
#17719=EDGE_CURVE('',#14779,#14778,#943,.F.);
#17720=EDGE_CURVE('',#14779,#14780,#7605,.T.);
#17721=EDGE_CURVE('',#14781,#14780,#944,.F.);
#17722=EDGE_CURVE('',#14781,#14782,#13728,.T.);
#17723=EDGE_CURVE('',#14775,#14782,#945,.F.);
#17724=EDGE_CURVE('',#14783,#14784,#7606,.T.);
#17725=EDGE_CURVE('',#14785,#14784,#946,.F.);
#17726=EDGE_CURVE('',#14785,#14786,#13729,.T.);
#17727=EDGE_CURVE('',#14787,#14786,#947,.F.);
#17728=EDGE_CURVE('',#14787,#14788,#7607,.T.);
#17729=EDGE_CURVE('',#14789,#14788,#948,.F.);
#17730=EDGE_CURVE('',#14789,#14790,#13730,.T.);
#17731=EDGE_CURVE('',#14783,#14790,#949,.F.);
#17732=EDGE_CURVE('',#14791,#14792,#7608,.T.);
#17733=EDGE_CURVE('',#14793,#14792,#950,.F.);
#17734=EDGE_CURVE('',#14793,#14794,#13731,.T.);
#17735=EDGE_CURVE('',#14795,#14794,#951,.F.);
#17736=EDGE_CURVE('',#14795,#14796,#7609,.T.);
#17737=EDGE_CURVE('',#14797,#14796,#952,.F.);
#17738=EDGE_CURVE('',#14797,#14798,#13732,.T.);
#17739=EDGE_CURVE('',#14791,#14798,#953,.F.);
#17740=EDGE_CURVE('',#14799,#14800,#7610,.T.);
#17741=EDGE_CURVE('',#14801,#14800,#954,.F.);
#17742=EDGE_CURVE('',#14801,#14802,#13733,.T.);
#17743=EDGE_CURVE('',#14803,#14802,#955,.F.);
#17744=EDGE_CURVE('',#14803,#14804,#7611,.T.);
#17745=EDGE_CURVE('',#14805,#14804,#956,.F.);
#17746=EDGE_CURVE('',#14805,#14806,#13734,.T.);
#17747=EDGE_CURVE('',#14799,#14806,#957,.F.);
#17748=EDGE_CURVE('',#14807,#14808,#7612,.T.);
#17749=EDGE_CURVE('',#14809,#14808,#958,.F.);
#17750=EDGE_CURVE('',#14809,#14810,#13735,.T.);
#17751=EDGE_CURVE('',#14811,#14810,#959,.F.);
#17752=EDGE_CURVE('',#14811,#14812,#7613,.T.);
#17753=EDGE_CURVE('',#14813,#14812,#960,.F.);
#17754=EDGE_CURVE('',#14813,#14814,#13736,.T.);
#17755=EDGE_CURVE('',#14807,#14814,#961,.F.);
#17756=EDGE_CURVE('',#14815,#14816,#7614,.T.);
#17757=EDGE_CURVE('',#14817,#14816,#962,.F.);
#17758=EDGE_CURVE('',#14817,#14818,#13737,.T.);
#17759=EDGE_CURVE('',#14819,#14818,#963,.F.);
#17760=EDGE_CURVE('',#14819,#14820,#7615,.T.);
#17761=EDGE_CURVE('',#14821,#14820,#964,.F.);
#17762=EDGE_CURVE('',#14821,#14822,#13738,.T.);
#17763=EDGE_CURVE('',#14815,#14822,#965,.F.);
#17764=EDGE_CURVE('',#14823,#14824,#7616,.T.);
#17765=EDGE_CURVE('',#14825,#14824,#966,.F.);
#17766=EDGE_CURVE('',#14825,#14826,#13739,.T.);
#17767=EDGE_CURVE('',#14827,#14826,#967,.F.);
#17768=EDGE_CURVE('',#14827,#14828,#7617,.T.);
#17769=EDGE_CURVE('',#14829,#14828,#968,.F.);
#17770=EDGE_CURVE('',#14829,#14830,#13740,.T.);
#17771=EDGE_CURVE('',#14823,#14830,#969,.F.);
#17772=EDGE_CURVE('',#14831,#14832,#7618,.T.);
#17773=EDGE_CURVE('',#14833,#14832,#970,.F.);
#17774=EDGE_CURVE('',#14833,#14834,#13741,.T.);
#17775=EDGE_CURVE('',#14835,#14834,#971,.F.);
#17776=EDGE_CURVE('',#14835,#14836,#7619,.T.);
#17777=EDGE_CURVE('',#14837,#14836,#972,.F.);
#17778=EDGE_CURVE('',#14837,#14838,#13742,.T.);
#17779=EDGE_CURVE('',#14831,#14838,#973,.F.);
#17780=EDGE_CURVE('',#14839,#14840,#7620,.T.);
#17781=EDGE_CURVE('',#14841,#14840,#974,.F.);
#17782=EDGE_CURVE('',#14841,#14842,#13743,.T.);
#17783=EDGE_CURVE('',#14843,#14842,#975,.F.);
#17784=EDGE_CURVE('',#14843,#14844,#7621,.T.);
#17785=EDGE_CURVE('',#14845,#14844,#976,.F.);
#17786=EDGE_CURVE('',#14845,#14846,#13744,.T.);
#17787=EDGE_CURVE('',#14839,#14846,#977,.F.);
#17788=EDGE_CURVE('',#14847,#14848,#7622,.T.);
#17789=EDGE_CURVE('',#14849,#14848,#978,.F.);
#17790=EDGE_CURVE('',#14849,#14850,#13745,.T.);
#17791=EDGE_CURVE('',#14851,#14850,#979,.F.);
#17792=EDGE_CURVE('',#14851,#14852,#7623,.T.);
#17793=EDGE_CURVE('',#14853,#14852,#980,.F.);
#17794=EDGE_CURVE('',#14853,#14854,#13746,.T.);
#17795=EDGE_CURVE('',#14847,#14854,#981,.F.);
#17796=EDGE_CURVE('',#14855,#14856,#7624,.T.);
#17797=EDGE_CURVE('',#14857,#14856,#982,.F.);
#17798=EDGE_CURVE('',#14857,#14858,#13747,.T.);
#17799=EDGE_CURVE('',#14859,#14858,#983,.F.);
#17800=EDGE_CURVE('',#14859,#14860,#7625,.T.);
#17801=EDGE_CURVE('',#14861,#14860,#984,.F.);
#17802=EDGE_CURVE('',#14861,#14862,#13748,.T.);
#17803=EDGE_CURVE('',#14855,#14862,#985,.F.);
#17804=EDGE_CURVE('',#14863,#14864,#7626,.T.);
#17805=EDGE_CURVE('',#14865,#14864,#986,.F.);
#17806=EDGE_CURVE('',#14865,#14866,#13749,.T.);
#17807=EDGE_CURVE('',#14867,#14866,#987,.F.);
#17808=EDGE_CURVE('',#14867,#14868,#7627,.T.);
#17809=EDGE_CURVE('',#14869,#14868,#988,.F.);
#17810=EDGE_CURVE('',#14869,#14870,#13750,.T.);
#17811=EDGE_CURVE('',#14863,#14870,#989,.F.);
#17812=EDGE_CURVE('',#14871,#14872,#7628,.T.);
#17813=EDGE_CURVE('',#14873,#14872,#990,.F.);
#17814=EDGE_CURVE('',#14873,#14874,#13751,.T.);
#17815=EDGE_CURVE('',#14875,#14874,#991,.F.);
#17816=EDGE_CURVE('',#14875,#14876,#7629,.T.);
#17817=EDGE_CURVE('',#14877,#14876,#992,.F.);
#17818=EDGE_CURVE('',#14877,#14878,#13752,.T.);
#17819=EDGE_CURVE('',#14871,#14878,#993,.F.);
#17820=EDGE_CURVE('',#14879,#14880,#7630,.T.);
#17821=EDGE_CURVE('',#14881,#14880,#994,.F.);
#17822=EDGE_CURVE('',#14881,#14882,#13753,.T.);
#17823=EDGE_CURVE('',#14883,#14882,#995,.F.);
#17824=EDGE_CURVE('',#14883,#14884,#7631,.T.);
#17825=EDGE_CURVE('',#14885,#14884,#996,.F.);
#17826=EDGE_CURVE('',#14885,#14886,#13754,.T.);
#17827=EDGE_CURVE('',#14879,#14886,#997,.F.);
#17828=EDGE_CURVE('',#14887,#14888,#7632,.T.);
#17829=EDGE_CURVE('',#14889,#14888,#998,.F.);
#17830=EDGE_CURVE('',#14889,#14890,#13755,.T.);
#17831=EDGE_CURVE('',#14891,#14890,#999,.F.);
#17832=EDGE_CURVE('',#14891,#14892,#7633,.T.);
#17833=EDGE_CURVE('',#14893,#14892,#1000,.F.);
#17834=EDGE_CURVE('',#14893,#14894,#13756,.T.);
#17835=EDGE_CURVE('',#14887,#14894,#1001,.F.);
#17836=EDGE_CURVE('',#14895,#14896,#7634,.T.);
#17837=EDGE_CURVE('',#14897,#14896,#1002,.F.);
#17838=EDGE_CURVE('',#14897,#14898,#13757,.T.);
#17839=EDGE_CURVE('',#14899,#14898,#1003,.F.);
#17840=EDGE_CURVE('',#14899,#14900,#7635,.T.);
#17841=EDGE_CURVE('',#14901,#14900,#1004,.F.);
#17842=EDGE_CURVE('',#14901,#14902,#13758,.T.);
#17843=EDGE_CURVE('',#14895,#14902,#1005,.F.);
#17844=EDGE_CURVE('',#14903,#14904,#7636,.T.);
#17845=EDGE_CURVE('',#14905,#14904,#1006,.F.);
#17846=EDGE_CURVE('',#14905,#14906,#13759,.T.);
#17847=EDGE_CURVE('',#14907,#14906,#1007,.F.);
#17848=EDGE_CURVE('',#14907,#14908,#7637,.T.);
#17849=EDGE_CURVE('',#14909,#14908,#1008,.F.);
#17850=EDGE_CURVE('',#14909,#14910,#13760,.T.);
#17851=EDGE_CURVE('',#14903,#14910,#1009,.F.);
#17852=EDGE_CURVE('',#14911,#14912,#7638,.T.);
#17853=EDGE_CURVE('',#14913,#14912,#1010,.F.);
#17854=EDGE_CURVE('',#14913,#14914,#13761,.T.);
#17855=EDGE_CURVE('',#14915,#14914,#1011,.F.);
#17856=EDGE_CURVE('',#14915,#14916,#7639,.T.);
#17857=EDGE_CURVE('',#14917,#14916,#1012,.F.);
#17858=EDGE_CURVE('',#14917,#14918,#13762,.T.);
#17859=EDGE_CURVE('',#14911,#14918,#1013,.F.);
#17860=EDGE_CURVE('',#14919,#14920,#7640,.T.);
#17861=EDGE_CURVE('',#14921,#14920,#1014,.F.);
#17862=EDGE_CURVE('',#14921,#14922,#13763,.T.);
#17863=EDGE_CURVE('',#14923,#14922,#1015,.F.);
#17864=EDGE_CURVE('',#14923,#14924,#7641,.T.);
#17865=EDGE_CURVE('',#14925,#14924,#1016,.F.);
#17866=EDGE_CURVE('',#14925,#14926,#13764,.T.);
#17867=EDGE_CURVE('',#14919,#14926,#1017,.F.);
#17868=EDGE_CURVE('',#14927,#14928,#7642,.T.);
#17869=EDGE_CURVE('',#14929,#14928,#1018,.F.);
#17870=EDGE_CURVE('',#14929,#14930,#13765,.T.);
#17871=EDGE_CURVE('',#14931,#14930,#1019,.F.);
#17872=EDGE_CURVE('',#14931,#14932,#7643,.T.);
#17873=EDGE_CURVE('',#14933,#14932,#1020,.F.);
#17874=EDGE_CURVE('',#14933,#14934,#13766,.T.);
#17875=EDGE_CURVE('',#14927,#14934,#1021,.F.);
#17876=EDGE_CURVE('',#14935,#14936,#7644,.T.);
#17877=EDGE_CURVE('',#14937,#14936,#1022,.F.);
#17878=EDGE_CURVE('',#14937,#14938,#13767,.T.);
#17879=EDGE_CURVE('',#14939,#14938,#1023,.F.);
#17880=EDGE_CURVE('',#14939,#14940,#7645,.T.);
#17881=EDGE_CURVE('',#14941,#14940,#1024,.F.);
#17882=EDGE_CURVE('',#14941,#14942,#13768,.T.);
#17883=EDGE_CURVE('',#14935,#14942,#1025,.F.);
#17884=EDGE_CURVE('',#14943,#14944,#7646,.T.);
#17885=EDGE_CURVE('',#14945,#14944,#1026,.F.);
#17886=EDGE_CURVE('',#14945,#14946,#13769,.T.);
#17887=EDGE_CURVE('',#14947,#14946,#1027,.F.);
#17888=EDGE_CURVE('',#14947,#14948,#7647,.T.);
#17889=EDGE_CURVE('',#14949,#14948,#1028,.F.);
#17890=EDGE_CURVE('',#14949,#14950,#13770,.T.);
#17891=EDGE_CURVE('',#14943,#14950,#1029,.F.);
#17892=EDGE_CURVE('',#14951,#14952,#7648,.T.);
#17893=EDGE_CURVE('',#14953,#14952,#1030,.F.);
#17894=EDGE_CURVE('',#14953,#14954,#13771,.T.);
#17895=EDGE_CURVE('',#14955,#14954,#1031,.F.);
#17896=EDGE_CURVE('',#14955,#14956,#7649,.T.);
#17897=EDGE_CURVE('',#14957,#14956,#1032,.F.);
#17898=EDGE_CURVE('',#14957,#14958,#13772,.T.);
#17899=EDGE_CURVE('',#14951,#14958,#1033,.F.);
#17900=EDGE_CURVE('',#14959,#14960,#7650,.T.);
#17901=EDGE_CURVE('',#14961,#14960,#1034,.F.);
#17902=EDGE_CURVE('',#14961,#14962,#13773,.T.);
#17903=EDGE_CURVE('',#14963,#14962,#1035,.F.);
#17904=EDGE_CURVE('',#14963,#14964,#7651,.T.);
#17905=EDGE_CURVE('',#14965,#14964,#1036,.F.);
#17906=EDGE_CURVE('',#14965,#14966,#13774,.T.);
#17907=EDGE_CURVE('',#14959,#14966,#1037,.F.);
#17908=EDGE_CURVE('',#14967,#14968,#7652,.T.);
#17909=EDGE_CURVE('',#14969,#14968,#1038,.F.);
#17910=EDGE_CURVE('',#14969,#14970,#13775,.T.);
#17911=EDGE_CURVE('',#14971,#14970,#1039,.F.);
#17912=EDGE_CURVE('',#14971,#14972,#7653,.T.);
#17913=EDGE_CURVE('',#14973,#14972,#1040,.F.);
#17914=EDGE_CURVE('',#14973,#14974,#13776,.T.);
#17915=EDGE_CURVE('',#14967,#14974,#1041,.F.);
#17916=EDGE_CURVE('',#14975,#14976,#7654,.T.);
#17917=EDGE_CURVE('',#14977,#14976,#1042,.F.);
#17918=EDGE_CURVE('',#14977,#14978,#13777,.T.);
#17919=EDGE_CURVE('',#14979,#14978,#1043,.F.);
#17920=EDGE_CURVE('',#14979,#14980,#7655,.T.);
#17921=EDGE_CURVE('',#14981,#14980,#1044,.F.);
#17922=EDGE_CURVE('',#14981,#14982,#13778,.T.);
#17923=EDGE_CURVE('',#14975,#14982,#1045,.F.);
#17924=EDGE_CURVE('',#14983,#14984,#7656,.T.);
#17925=EDGE_CURVE('',#14985,#14984,#1046,.F.);
#17926=EDGE_CURVE('',#14985,#14986,#13779,.T.);
#17927=EDGE_CURVE('',#14987,#14986,#1047,.F.);
#17928=EDGE_CURVE('',#14987,#14988,#7657,.T.);
#17929=EDGE_CURVE('',#14989,#14988,#1048,.F.);
#17930=EDGE_CURVE('',#14989,#14990,#13780,.T.);
#17931=EDGE_CURVE('',#14983,#14990,#1049,.F.);
#17932=EDGE_CURVE('',#14991,#14992,#7658,.T.);
#17933=EDGE_CURVE('',#14993,#14992,#1050,.F.);
#17934=EDGE_CURVE('',#14993,#14994,#13781,.T.);
#17935=EDGE_CURVE('',#14995,#14994,#1051,.F.);
#17936=EDGE_CURVE('',#14995,#14996,#7659,.T.);
#17937=EDGE_CURVE('',#14997,#14996,#1052,.F.);
#17938=EDGE_CURVE('',#14997,#14998,#13782,.T.);
#17939=EDGE_CURVE('',#14991,#14998,#1053,.F.);
#17940=EDGE_CURVE('',#14999,#15000,#7660,.T.);
#17941=EDGE_CURVE('',#15001,#15000,#1054,.F.);
#17942=EDGE_CURVE('',#15001,#15002,#13783,.T.);
#17943=EDGE_CURVE('',#15003,#15002,#1055,.F.);
#17944=EDGE_CURVE('',#15003,#15004,#7661,.T.);
#17945=EDGE_CURVE('',#15005,#15004,#1056,.F.);
#17946=EDGE_CURVE('',#15005,#15006,#13784,.T.);
#17947=EDGE_CURVE('',#14999,#15006,#1057,.F.);
#17948=EDGE_CURVE('',#15007,#15008,#7662,.T.);
#17949=EDGE_CURVE('',#15009,#15008,#1058,.F.);
#17950=EDGE_CURVE('',#15009,#15010,#13785,.T.);
#17951=EDGE_CURVE('',#15011,#15010,#1059,.F.);
#17952=EDGE_CURVE('',#15011,#15012,#7663,.T.);
#17953=EDGE_CURVE('',#15013,#15012,#1060,.F.);
#17954=EDGE_CURVE('',#15013,#15014,#13786,.T.);
#17955=EDGE_CURVE('',#15007,#15014,#1061,.F.);
#17956=EDGE_CURVE('',#15015,#15016,#7664,.T.);
#17957=EDGE_CURVE('',#15017,#15016,#1062,.F.);
#17958=EDGE_CURVE('',#15017,#15018,#13787,.T.);
#17959=EDGE_CURVE('',#15019,#15018,#1063,.F.);
#17960=EDGE_CURVE('',#15019,#15020,#7665,.T.);
#17961=EDGE_CURVE('',#15021,#15020,#1064,.F.);
#17962=EDGE_CURVE('',#15021,#15022,#13788,.T.);
#17963=EDGE_CURVE('',#15015,#15022,#1065,.F.);
#17964=EDGE_CURVE('',#15023,#15024,#7666,.T.);
#17965=EDGE_CURVE('',#15025,#15024,#1066,.F.);
#17966=EDGE_CURVE('',#15025,#15026,#13789,.T.);
#17967=EDGE_CURVE('',#15027,#15026,#1067,.F.);
#17968=EDGE_CURVE('',#15027,#15028,#7667,.T.);
#17969=EDGE_CURVE('',#15029,#15028,#1068,.F.);
#17970=EDGE_CURVE('',#15029,#15030,#13790,.T.);
#17971=EDGE_CURVE('',#15023,#15030,#1069,.F.);
#17972=EDGE_CURVE('',#15031,#15032,#7668,.T.);
#17973=EDGE_CURVE('',#15033,#15032,#1070,.F.);
#17974=EDGE_CURVE('',#15033,#15034,#13791,.T.);
#17975=EDGE_CURVE('',#15035,#15034,#1071,.F.);
#17976=EDGE_CURVE('',#15035,#15036,#7669,.T.);
#17977=EDGE_CURVE('',#15037,#15036,#1072,.F.);
#17978=EDGE_CURVE('',#15037,#15038,#13792,.T.);
#17979=EDGE_CURVE('',#15031,#15038,#1073,.F.);
#17980=EDGE_CURVE('',#15039,#15040,#7670,.T.);
#17981=EDGE_CURVE('',#15041,#15040,#1074,.F.);
#17982=EDGE_CURVE('',#15041,#15042,#13793,.T.);
#17983=EDGE_CURVE('',#15043,#15042,#1075,.F.);
#17984=EDGE_CURVE('',#15043,#15044,#7671,.T.);
#17985=EDGE_CURVE('',#15045,#15044,#1076,.F.);
#17986=EDGE_CURVE('',#15045,#15046,#13794,.T.);
#17987=EDGE_CURVE('',#15039,#15046,#1077,.F.);
#17988=EDGE_CURVE('',#15047,#15048,#7672,.T.);
#17989=EDGE_CURVE('',#15049,#15048,#1078,.F.);
#17990=EDGE_CURVE('',#15049,#15050,#13795,.T.);
#17991=EDGE_CURVE('',#15051,#15050,#1079,.F.);
#17992=EDGE_CURVE('',#15051,#15052,#7673,.T.);
#17993=EDGE_CURVE('',#15053,#15052,#1080,.F.);
#17994=EDGE_CURVE('',#15053,#15054,#13796,.T.);
#17995=EDGE_CURVE('',#15047,#15054,#1081,.F.);
#17996=EDGE_CURVE('',#15055,#15056,#7674,.T.);
#17997=EDGE_CURVE('',#15057,#15056,#1082,.F.);
#17998=EDGE_CURVE('',#15057,#15058,#13797,.T.);
#17999=EDGE_CURVE('',#15059,#15058,#1083,.F.);
#18000=EDGE_CURVE('',#15059,#15060,#7675,.T.);
#18001=EDGE_CURVE('',#15061,#15060,#1084,.F.);
#18002=EDGE_CURVE('',#15061,#15062,#13798,.T.);
#18003=EDGE_CURVE('',#15055,#15062,#1085,.F.);
#18004=EDGE_CURVE('',#15063,#15064,#7676,.T.);
#18005=EDGE_CURVE('',#15065,#15064,#1086,.F.);
#18006=EDGE_CURVE('',#15065,#15066,#13799,.T.);
#18007=EDGE_CURVE('',#15067,#15066,#1087,.F.);
#18008=EDGE_CURVE('',#15067,#15068,#7677,.T.);
#18009=EDGE_CURVE('',#15069,#15068,#1088,.F.);
#18010=EDGE_CURVE('',#15069,#15070,#13800,.T.);
#18011=EDGE_CURVE('',#15063,#15070,#1089,.F.);
#18012=EDGE_CURVE('',#15071,#15072,#7678,.T.);
#18013=EDGE_CURVE('',#15073,#15072,#1090,.F.);
#18014=EDGE_CURVE('',#15073,#15074,#13801,.T.);
#18015=EDGE_CURVE('',#15075,#15074,#1091,.F.);
#18016=EDGE_CURVE('',#15075,#15076,#7679,.T.);
#18017=EDGE_CURVE('',#15077,#15076,#1092,.F.);
#18018=EDGE_CURVE('',#15077,#15078,#13802,.T.);
#18019=EDGE_CURVE('',#15071,#15078,#1093,.F.);
#18020=EDGE_CURVE('',#15079,#15080,#7680,.T.);
#18021=EDGE_CURVE('',#15081,#15080,#1094,.F.);
#18022=EDGE_CURVE('',#15081,#15082,#13803,.T.);
#18023=EDGE_CURVE('',#15083,#15082,#1095,.F.);
#18024=EDGE_CURVE('',#15083,#15084,#7681,.T.);
#18025=EDGE_CURVE('',#15085,#15084,#1096,.F.);
#18026=EDGE_CURVE('',#15085,#15086,#13804,.T.);
#18027=EDGE_CURVE('',#15079,#15086,#1097,.F.);
#18028=EDGE_CURVE('',#15087,#15088,#7682,.T.);
#18029=EDGE_CURVE('',#15089,#15088,#1098,.F.);
#18030=EDGE_CURVE('',#15089,#15090,#13805,.T.);
#18031=EDGE_CURVE('',#15091,#15090,#1099,.F.);
#18032=EDGE_CURVE('',#15091,#15092,#7683,.T.);
#18033=EDGE_CURVE('',#15093,#15092,#1100,.F.);
#18034=EDGE_CURVE('',#15093,#15094,#13806,.T.);
#18035=EDGE_CURVE('',#15087,#15094,#1101,.F.);
#18036=EDGE_CURVE('',#15095,#15096,#7684,.T.);
#18037=EDGE_CURVE('',#15097,#15096,#1102,.F.);
#18038=EDGE_CURVE('',#15097,#15098,#13807,.T.);
#18039=EDGE_CURVE('',#15099,#15098,#1103,.F.);
#18040=EDGE_CURVE('',#15099,#15100,#7685,.T.);
#18041=EDGE_CURVE('',#15101,#15100,#1104,.F.);
#18042=EDGE_CURVE('',#15101,#15102,#13808,.T.);
#18043=EDGE_CURVE('',#15095,#15102,#1105,.F.);
#18044=EDGE_CURVE('',#15103,#15104,#7686,.T.);
#18045=EDGE_CURVE('',#15105,#15104,#1106,.F.);
#18046=EDGE_CURVE('',#15105,#15106,#13809,.T.);
#18047=EDGE_CURVE('',#15107,#15106,#1107,.F.);
#18048=EDGE_CURVE('',#15107,#15108,#7687,.T.);
#18049=EDGE_CURVE('',#15109,#15108,#1108,.F.);
#18050=EDGE_CURVE('',#15109,#15110,#13810,.T.);
#18051=EDGE_CURVE('',#15103,#15110,#1109,.F.);
#18052=EDGE_CURVE('',#15111,#15112,#7688,.T.);
#18053=EDGE_CURVE('',#15113,#15112,#1110,.F.);
#18054=EDGE_CURVE('',#15113,#15114,#13811,.T.);
#18055=EDGE_CURVE('',#15115,#15114,#1111,.F.);
#18056=EDGE_CURVE('',#15115,#15116,#7689,.T.);
#18057=EDGE_CURVE('',#15117,#15116,#1112,.F.);
#18058=EDGE_CURVE('',#15117,#15118,#13812,.T.);
#18059=EDGE_CURVE('',#15111,#15118,#1113,.F.);
#18060=EDGE_CURVE('',#15119,#15120,#7690,.T.);
#18061=EDGE_CURVE('',#15121,#15120,#1114,.F.);
#18062=EDGE_CURVE('',#15121,#15122,#13813,.T.);
#18063=EDGE_CURVE('',#15123,#15122,#1115,.F.);
#18064=EDGE_CURVE('',#15123,#15124,#7691,.T.);
#18065=EDGE_CURVE('',#15125,#15124,#1116,.F.);
#18066=EDGE_CURVE('',#15125,#15126,#13814,.T.);
#18067=EDGE_CURVE('',#15119,#15126,#1117,.F.);
#18068=EDGE_CURVE('',#15127,#15128,#7692,.T.);
#18069=EDGE_CURVE('',#15129,#15128,#1118,.F.);
#18070=EDGE_CURVE('',#15129,#15130,#13815,.T.);
#18071=EDGE_CURVE('',#15131,#15130,#1119,.F.);
#18072=EDGE_CURVE('',#15131,#15132,#7693,.T.);
#18073=EDGE_CURVE('',#15133,#15132,#1120,.F.);
#18074=EDGE_CURVE('',#15133,#15134,#13816,.T.);
#18075=EDGE_CURVE('',#15127,#15134,#1121,.F.);
#18076=EDGE_CURVE('',#15135,#15136,#7694,.T.);
#18077=EDGE_CURVE('',#15137,#15136,#1122,.F.);
#18078=EDGE_CURVE('',#15137,#15138,#13817,.T.);
#18079=EDGE_CURVE('',#15139,#15138,#1123,.F.);
#18080=EDGE_CURVE('',#15139,#15140,#7695,.T.);
#18081=EDGE_CURVE('',#15141,#15140,#1124,.F.);
#18082=EDGE_CURVE('',#15141,#15142,#13818,.T.);
#18083=EDGE_CURVE('',#15135,#15142,#1125,.F.);
#18084=EDGE_CURVE('',#15143,#15144,#7696,.T.);
#18085=EDGE_CURVE('',#15145,#15144,#1126,.F.);
#18086=EDGE_CURVE('',#15145,#15146,#13819,.T.);
#18087=EDGE_CURVE('',#15147,#15146,#1127,.F.);
#18088=EDGE_CURVE('',#15147,#15148,#7697,.T.);
#18089=EDGE_CURVE('',#15149,#15148,#1128,.F.);
#18090=EDGE_CURVE('',#15149,#15150,#13820,.T.);
#18091=EDGE_CURVE('',#15143,#15150,#1129,.F.);
#18092=EDGE_CURVE('',#15151,#15152,#13821,.T.);
#18093=EDGE_CURVE('',#15152,#15153,#347,.T.);
#18094=EDGE_CURVE('',#15153,#15154,#13822,.T.);
#18095=EDGE_CURVE('',#15151,#15154,#348,.T.);
#18096=EDGE_CURVE('',#15152,#15155,#13823,.T.);
#18097=EDGE_CURVE('',#15155,#15156,#349,.T.);
#18098=EDGE_CURVE('',#15156,#15153,#13824,.T.);
#18099=EDGE_CURVE('',#15155,#15157,#13825,.T.);
#18100=EDGE_CURVE('',#15157,#15158,#350,.T.);
#18101=EDGE_CURVE('',#15158,#15156,#13826,.T.);
#18102=EDGE_CURVE('',#15157,#15159,#13827,.T.);
#18103=EDGE_CURVE('',#15159,#15160,#351,.T.);
#18104=EDGE_CURVE('',#15160,#15158,#13828,.T.);
#18105=EDGE_CURVE('',#15159,#15161,#13829,.T.);
#18106=EDGE_CURVE('',#15161,#15162,#352,.T.);
#18107=EDGE_CURVE('',#15162,#15160,#13830,.T.);
#18108=EDGE_CURVE('',#15161,#15163,#13831,.T.);
#18109=EDGE_CURVE('',#15163,#15164,#353,.T.);
#18110=EDGE_CURVE('',#15164,#15162,#13832,.T.);
#18111=EDGE_CURVE('',#15165,#15164,#13833,.T.);
#18112=EDGE_CURVE('',#15163,#15166,#13834,.T.);
#18113=EDGE_CURVE('',#15166,#15165,#354,.T.);
#18114=EDGE_CURVE('',#15167,#15165,#13835,.T.);
#18115=EDGE_CURVE('',#15166,#15168,#13836,.T.);
#18116=EDGE_CURVE('',#15168,#15167,#355,.T.);
#18117=EDGE_CURVE('',#15169,#15167,#13837,.T.);
#18118=EDGE_CURVE('',#15168,#15170,#13838,.T.);
#18119=EDGE_CURVE('',#15170,#15169,#356,.T.);
#18120=EDGE_CURVE('',#15154,#15169,#13839,.T.);
#18121=EDGE_CURVE('',#15170,#15151,#13840,.T.);
#18122=EDGE_CURVE('',#15171,#15164,#7698,.T.);
#18123=EDGE_CURVE('',#15172,#15171,#13841,.T.);
#18124=EDGE_CURVE('',#15172,#15162,#7699,.T.);
#18125=EDGE_CURVE('',#15173,#15165,#7700,.T.);
#18126=EDGE_CURVE('',#15171,#15173,#13842,.T.);
#18127=EDGE_CURVE('',#15174,#15167,#7701,.T.);
#18128=EDGE_CURVE('',#15173,#15174,#13843,.T.);
#18129=EDGE_CURVE('',#15175,#15169,#7702,.T.);
#18130=EDGE_CURVE('',#15174,#15175,#13844,.T.);
#18131=EDGE_CURVE('',#15176,#15154,#7703,.T.);
#18132=EDGE_CURVE('',#15175,#15176,#13845,.T.);
#18133=EDGE_CURVE('',#15177,#15153,#7704,.T.);
#18134=EDGE_CURVE('',#15176,#15177,#13846,.T.);
#18135=EDGE_CURVE('',#15178,#15178,#13847,.T.);
#18136=EDGE_CURVE('',#15179,#15179,#13848,.T.);
#18137=EDGE_CURVE('',#15180,#15180,#13849,.T.);
#18138=EDGE_CURVE('',#15181,#15181,#13850,.T.);
#18139=EDGE_CURVE('',#15182,#15182,#13851,.T.);
#18140=EDGE_CURVE('',#15183,#15184,#7705,.T.);
#18141=EDGE_CURVE('',#15184,#14589,#7706,.T.);
#18142=EDGE_CURVE('',#14588,#15185,#7707,.T.);
#18143=EDGE_CURVE('',#15185,#15183,#7708,.T.);
#18144=EDGE_CURVE('',#15186,#15184,#7709,.T.);
#18145=EDGE_CURVE('',#14590,#15186,#7710,.T.);
#18146=EDGE_CURVE('',#15187,#15183,#7711,.T.);
#18147=EDGE_CURVE('',#15187,#15188,#7712,.T.);
#18148=EDGE_CURVE('',#15188,#15186,#7713,.T.);
#18149=EDGE_CURVE('',#15185,#15189,#7714,.T.);
#18150=EDGE_CURVE('',#15189,#15190,#7715,.T.);
#18151=EDGE_CURVE('',#15190,#15187,#7716,.T.);
#18152=EDGE_CURVE('',#15191,#15188,#7717,.T.);
#18153=EDGE_CURVE('',#15186,#15191,#7718,.T.);
#18154=EDGE_CURVE('',#15192,#15189,#7719,.T.);
#18155=EDGE_CURVE('',#15190,#15192,#7720,.T.);
#18156=EDGE_CURVE('',#14586,#15192,#7721,.T.);
#18157=EDGE_CURVE('',#15189,#14587,#7722,.T.);
#18158=EDGE_CURVE('',#15193,#15194,#7723,.T.);
#18159=EDGE_CURVE('',#15195,#15193,#7724,.T.);
#18160=EDGE_CURVE('',#15194,#15195,#7725,.T.);
#18161=EDGE_CURVE('',#14584,#15195,#7726,.T.);
#18162=EDGE_CURVE('',#15193,#14585,#7727,.T.);
#18163=EDGE_CURVE('',#15188,#15194,#7728,.T.);
#18164=EDGE_CURVE('',#15195,#15191,#7729,.T.);
#18165=EDGE_CURVE('',#15194,#15190,#7730,.T.);
#18166=EDGE_CURVE('',#15192,#15193,#7731,.T.);
#18167=EDGE_CURVE('',#15191,#14583,#7732,.T.);
#18168=EDGE_CURVE('',#15196,#15197,#7733,.T.);
#18169=EDGE_CURVE('',#15198,#15196,#7734,.T.);
#18170=EDGE_CURVE('',#15197,#15198,#7735,.T.);
#18171=EDGE_CURVE('',#15199,#15200,#7736,.T.);
#18172=EDGE_CURVE('',#15201,#15199,#7737,.T.);
#18173=EDGE_CURVE('',#15200,#15201,#7738,.T.);
#18174=EDGE_CURVE('',#15202,#15203,#7739,.T.);
#18175=EDGE_CURVE('',#15204,#15202,#7740,.T.);
#18176=EDGE_CURVE('',#15203,#15204,#7741,.T.);
#18177=EDGE_CURVE('',#14594,#15204,#7742,.T.);
#18178=EDGE_CURVE('',#15202,#14595,#7743,.T.);
#18179=EDGE_CURVE('',#15205,#15206,#7744,.T.);
#18180=EDGE_CURVE('',#15207,#15205,#7745,.T.);
#18181=EDGE_CURVE('',#15206,#15207,#7746,.T.);
#18182=EDGE_CURVE('',#14592,#15207,#7747,.T.);
#18183=EDGE_CURVE('',#15205,#14593,#7748,.T.);
#18184=EDGE_CURVE('',#15199,#15206,#7749,.T.);
#18185=EDGE_CURVE('',#15207,#15201,#7750,.T.);
#18186=EDGE_CURVE('',#15206,#15203,#7751,.T.);
#18187=EDGE_CURVE('',#15204,#15205,#7752,.T.);
#18188=EDGE_CURVE('',#15196,#15202,#7753,.T.);
#18189=EDGE_CURVE('',#15203,#15198,#7754,.T.);
#18190=EDGE_CURVE('',#14598,#15200,#7755,.T.);
#18191=EDGE_CURVE('',#15201,#14591,#7756,.T.);
#18192=EDGE_CURVE('',#15200,#15197,#7757,.T.);
#18193=EDGE_CURVE('',#15198,#15199,#7758,.T.);
#18194=EDGE_CURVE('',#14596,#15196,#7759,.T.);
#18195=EDGE_CURVE('',#15197,#14597,#7760,.T.);
#18196=EDGE_CURVE('',#15208,#15209,#7761,.T.);
#18197=EDGE_CURVE('',#15210,#15208,#7762,.T.);
#18198=EDGE_CURVE('',#15209,#15210,#7763,.T.);
#18199=EDGE_CURVE('',#15211,#15212,#7764,.T.);
#18200=EDGE_CURVE('',#15212,#15210,#7765,.T.);
#18201=EDGE_CURVE('',#15208,#15213,#7766,.T.);
#18202=EDGE_CURVE('',#15213,#15211,#7767,.T.);
#18203=EDGE_CURVE('',#14606,#15209,#7768,.T.);
#18204=EDGE_CURVE('',#15210,#14599,#7769,.T.);
#18205=EDGE_CURVE('',#15214,#15215,#7770,.T.);
#18206=EDGE_CURVE('',#15216,#15214,#7771,.T.);
#18207=EDGE_CURVE('',#15215,#15216,#7772,.T.);
#18208=EDGE_CURVE('',#15217,#15218,#7773,.T.);
#18209=EDGE_CURVE('',#15218,#15216,#7774,.T.);
#18210=EDGE_CURVE('',#15214,#15219,#7775,.T.);
#18211=EDGE_CURVE('',#15219,#15217,#7776,.T.);
#18212=EDGE_CURVE('',#15209,#15215,#7777,.T.);
#18213=EDGE_CURVE('',#15216,#15208,#7778,.T.);
#18214=EDGE_CURVE('',#14604,#15214,#7779,.T.);
#18215=EDGE_CURVE('',#15215,#14605,#7780,.T.);
#18216=EDGE_CURVE('',#15211,#15220,#7781,.T.);
#18217=EDGE_CURVE('',#15220,#14601,#7782,.T.);
#18218=EDGE_CURVE('',#14600,#15212,#7783,.T.);
#18219=EDGE_CURVE('',#15213,#15218,#7784,.T.);
#18220=EDGE_CURVE('',#15221,#15217,#7785,.T.);
#18221=EDGE_CURVE('',#15221,#15220,#7786,.T.);
#18222=EDGE_CURVE('',#15219,#14603,#7787,.T.);
#18223=EDGE_CURVE('',#14602,#15221,#7788,.T.);
#18224=EDGE_CURVE('',#15222,#15223,#7789,.T.);
#18225=EDGE_CURVE('',#15224,#15222,#7790,.T.);
#18226=EDGE_CURVE('',#15223,#15224,#7791,.T.);
#18227=EDGE_CURVE('',#15225,#15226,#7792,.T.);
#18228=EDGE_CURVE('',#15227,#15225,#7793,.T.);
#18229=EDGE_CURVE('',#15226,#15227,#7794,.T.);
#18230=EDGE_CURVE('',#15228,#15229,#7795,.T.);
#18231=EDGE_CURVE('',#15230,#15228,#7796,.T.);
#18232=EDGE_CURVE('',#15229,#15230,#7797,.T.);
#18233=EDGE_CURVE('',#14610,#15230,#7798,.T.);
#18234=EDGE_CURVE('',#15228,#14611,#7799,.T.);
#18235=EDGE_CURVE('',#15231,#15232,#7800,.T.);
#18236=EDGE_CURVE('',#15233,#15231,#7801,.T.);
#18237=EDGE_CURVE('',#15232,#15233,#7802,.T.);
#18238=EDGE_CURVE('',#14608,#15233,#7803,.T.);
#18239=EDGE_CURVE('',#15231,#14609,#7804,.T.);
#18240=EDGE_CURVE('',#15225,#15232,#7805,.T.);
#18241=EDGE_CURVE('',#15233,#15227,#7806,.T.);
#18242=EDGE_CURVE('',#15232,#15229,#7807,.T.);
#18243=EDGE_CURVE('',#15230,#15231,#7808,.T.);
#18244=EDGE_CURVE('',#15222,#15228,#7809,.T.);
#18245=EDGE_CURVE('',#15229,#15224,#7810,.T.);
#18246=EDGE_CURVE('',#14614,#15226,#7811,.T.);
#18247=EDGE_CURVE('',#15227,#14607,#7812,.T.);
#18248=EDGE_CURVE('',#15226,#15223,#7813,.T.);
#18249=EDGE_CURVE('',#15224,#15225,#7814,.T.);
#18250=EDGE_CURVE('',#14612,#15222,#7815,.T.);
#18251=EDGE_CURVE('',#15223,#14613,#7816,.T.);
#18252=EDGE_CURVE('',#15234,#15235,#7817,.T.);
#18253=EDGE_CURVE('',#15236,#15234,#7818,.T.);
#18254=EDGE_CURVE('',#15235,#15236,#7819,.T.);
#18255=EDGE_CURVE('',#15237,#15238,#7820,.T.);
#18256=EDGE_CURVE('',#15239,#15237,#7821,.T.);
#18257=EDGE_CURVE('',#15238,#15239,#7822,.T.);
#18258=EDGE_CURVE('',#15240,#15241,#7823,.T.);
#18259=EDGE_CURVE('',#15242,#15240,#7824,.T.);
#18260=EDGE_CURVE('',#15241,#15242,#7825,.T.);
#18261=EDGE_CURVE('',#14618,#15242,#7826,.T.);
#18262=EDGE_CURVE('',#15240,#14619,#7827,.T.);
#18263=EDGE_CURVE('',#15243,#15244,#7828,.T.);
#18264=EDGE_CURVE('',#15245,#15243,#7829,.T.);
#18265=EDGE_CURVE('',#15244,#15245,#7830,.T.);
#18266=EDGE_CURVE('',#14616,#15245,#7831,.T.);
#18267=EDGE_CURVE('',#15243,#14617,#7832,.T.);
#18268=EDGE_CURVE('',#15237,#15244,#7833,.T.);
#18269=EDGE_CURVE('',#15245,#15239,#7834,.T.);
#18270=EDGE_CURVE('',#15244,#15241,#7835,.T.);
#18271=EDGE_CURVE('',#15242,#15243,#7836,.T.);
#18272=EDGE_CURVE('',#15234,#15240,#7837,.T.);
#18273=EDGE_CURVE('',#15241,#15236,#7838,.T.);
#18274=EDGE_CURVE('',#14622,#15238,#7839,.T.);
#18275=EDGE_CURVE('',#15239,#14615,#7840,.T.);
#18276=EDGE_CURVE('',#15238,#15235,#7841,.T.);
#18277=EDGE_CURVE('',#15236,#15237,#7842,.T.);
#18278=EDGE_CURVE('',#14620,#15234,#7843,.T.);
#18279=EDGE_CURVE('',#15235,#14621,#7844,.T.);
#18280=EDGE_CURVE('',#15246,#15247,#7845,.T.);
#18281=EDGE_CURVE('',#15247,#14629,#7846,.T.);
#18282=EDGE_CURVE('',#14628,#15248,#7847,.T.);
#18283=EDGE_CURVE('',#15248,#15246,#7848,.T.);
#18284=EDGE_CURVE('',#15249,#15247,#7849,.T.);
#18285=EDGE_CURVE('',#14630,#15249,#7850,.T.);
#18286=EDGE_CURVE('',#15250,#15246,#7851,.T.);
#18287=EDGE_CURVE('',#15250,#15251,#7852,.T.);
#18288=EDGE_CURVE('',#15251,#15249,#7853,.T.);
#18289=EDGE_CURVE('',#15248,#15252,#7854,.T.);
#18290=EDGE_CURVE('',#15252,#15253,#7855,.T.);
#18291=EDGE_CURVE('',#15253,#15250,#7856,.T.);
#18292=EDGE_CURVE('',#15254,#15251,#7857,.T.);
#18293=EDGE_CURVE('',#15249,#15254,#7858,.T.);
#18294=EDGE_CURVE('',#15255,#15252,#7859,.T.);
#18295=EDGE_CURVE('',#15253,#15255,#7860,.T.);
#18296=EDGE_CURVE('',#14626,#15255,#7861,.T.);
#18297=EDGE_CURVE('',#15252,#14627,#7862,.T.);
#18298=EDGE_CURVE('',#15256,#15257,#7863,.T.);
#18299=EDGE_CURVE('',#15258,#15256,#7864,.T.);
#18300=EDGE_CURVE('',#15257,#15258,#7865,.T.);
#18301=EDGE_CURVE('',#14624,#15258,#7866,.T.);
#18302=EDGE_CURVE('',#15256,#14625,#7867,.T.);
#18303=EDGE_CURVE('',#15251,#15257,#7868,.T.);
#18304=EDGE_CURVE('',#15258,#15254,#7869,.T.);
#18305=EDGE_CURVE('',#15257,#15253,#7870,.T.);
#18306=EDGE_CURVE('',#15255,#15256,#7871,.T.);
#18307=EDGE_CURVE('',#15254,#14623,#7872,.T.);
#18308=EDGE_CURVE('',#15259,#15260,#7873,.T.);
#18309=EDGE_CURVE('',#15261,#15259,#7874,.T.);
#18310=EDGE_CURVE('',#15260,#15261,#7875,.T.);
#18311=EDGE_CURVE('',#15262,#15263,#7876,.T.);
#18312=EDGE_CURVE('',#15264,#15262,#7877,.T.);
#18313=EDGE_CURVE('',#15263,#15264,#7878,.T.);
#18314=EDGE_CURVE('',#15265,#15266,#7879,.T.);
#18315=EDGE_CURVE('',#15267,#15265,#7880,.T.);
#18316=EDGE_CURVE('',#15266,#15267,#7881,.T.);
#18317=EDGE_CURVE('',#14634,#15267,#7882,.T.);
#18318=EDGE_CURVE('',#15265,#14635,#7883,.T.);
#18319=EDGE_CURVE('',#15268,#15269,#7884,.T.);
#18320=EDGE_CURVE('',#15270,#15268,#7885,.T.);
#18321=EDGE_CURVE('',#15269,#15270,#7886,.T.);
#18322=EDGE_CURVE('',#14632,#15270,#7887,.T.);
#18323=EDGE_CURVE('',#15268,#14633,#7888,.T.);
#18324=EDGE_CURVE('',#15262,#15269,#7889,.T.);
#18325=EDGE_CURVE('',#15270,#15264,#7890,.T.);
#18326=EDGE_CURVE('',#15269,#15266,#7891,.T.);
#18327=EDGE_CURVE('',#15267,#15268,#7892,.T.);
#18328=EDGE_CURVE('',#15259,#15265,#7893,.T.);
#18329=EDGE_CURVE('',#15266,#15261,#7894,.T.);
#18330=EDGE_CURVE('',#14638,#15263,#7895,.T.);
#18331=EDGE_CURVE('',#15264,#14631,#7896,.T.);
#18332=EDGE_CURVE('',#15263,#15260,#7897,.T.);
#18333=EDGE_CURVE('',#15261,#15262,#7898,.T.);
#18334=EDGE_CURVE('',#14636,#15259,#7899,.T.);
#18335=EDGE_CURVE('',#15260,#14637,#7900,.T.);
#18336=EDGE_CURVE('',#15271,#15272,#7901,.T.);
#18337=EDGE_CURVE('',#15273,#15271,#7902,.T.);
#18338=EDGE_CURVE('',#15272,#15273,#7903,.T.);
#18339=EDGE_CURVE('',#15274,#15275,#7904,.T.);
#18340=EDGE_CURVE('',#15275,#15273,#7905,.T.);
#18341=EDGE_CURVE('',#15271,#15276,#7906,.T.);
#18342=EDGE_CURVE('',#15276,#15274,#7907,.T.);
#18343=EDGE_CURVE('',#14646,#15272,#7908,.T.);
#18344=EDGE_CURVE('',#15273,#14639,#7909,.T.);
#18345=EDGE_CURVE('',#15277,#15278,#7910,.T.);
#18346=EDGE_CURVE('',#15279,#15277,#7911,.T.);
#18347=EDGE_CURVE('',#15278,#15279,#7912,.T.);
#18348=EDGE_CURVE('',#15280,#15281,#7913,.T.);
#18349=EDGE_CURVE('',#15281,#15279,#7914,.T.);
#18350=EDGE_CURVE('',#15277,#15282,#7915,.T.);
#18351=EDGE_CURVE('',#15282,#15280,#7916,.T.);
#18352=EDGE_CURVE('',#15272,#15278,#7917,.T.);
#18353=EDGE_CURVE('',#15279,#15271,#7918,.T.);
#18354=EDGE_CURVE('',#14644,#15277,#7919,.T.);
#18355=EDGE_CURVE('',#15278,#14645,#7920,.T.);
#18356=EDGE_CURVE('',#15274,#15283,#7921,.T.);
#18357=EDGE_CURVE('',#15283,#14641,#7922,.T.);
#18358=EDGE_CURVE('',#14640,#15275,#7923,.T.);
#18359=EDGE_CURVE('',#15276,#15281,#7924,.T.);
#18360=EDGE_CURVE('',#15284,#15280,#7925,.T.);
#18361=EDGE_CURVE('',#15284,#15283,#7926,.T.);
#18362=EDGE_CURVE('',#15282,#14643,#7927,.T.);
#18363=EDGE_CURVE('',#14642,#15284,#7928,.T.);
#18364=EDGE_CURVE('',#15285,#15286,#7929,.T.);
#18365=EDGE_CURVE('',#15287,#15285,#7930,.T.);
#18366=EDGE_CURVE('',#15286,#15287,#7931,.T.);
#18367=EDGE_CURVE('',#15288,#15289,#7932,.T.);
#18368=EDGE_CURVE('',#15290,#15288,#7933,.T.);
#18369=EDGE_CURVE('',#15289,#15290,#7934,.T.);
#18370=EDGE_CURVE('',#15291,#15292,#7935,.T.);
#18371=EDGE_CURVE('',#15293,#15291,#7936,.T.);
#18372=EDGE_CURVE('',#15292,#15293,#7937,.T.);
#18373=EDGE_CURVE('',#14650,#15293,#7938,.T.);
#18374=EDGE_CURVE('',#15291,#14651,#7939,.T.);
#18375=EDGE_CURVE('',#15294,#15295,#7940,.T.);
#18376=EDGE_CURVE('',#15296,#15294,#7941,.T.);
#18377=EDGE_CURVE('',#15295,#15296,#7942,.T.);
#18378=EDGE_CURVE('',#14648,#15296,#7943,.T.);
#18379=EDGE_CURVE('',#15294,#14649,#7944,.T.);
#18380=EDGE_CURVE('',#15288,#15295,#7945,.T.);
#18381=EDGE_CURVE('',#15296,#15290,#7946,.T.);
#18382=EDGE_CURVE('',#15295,#15292,#7947,.T.);
#18383=EDGE_CURVE('',#15293,#15294,#7948,.T.);
#18384=EDGE_CURVE('',#15285,#15291,#7949,.T.);
#18385=EDGE_CURVE('',#15292,#15287,#7950,.T.);
#18386=EDGE_CURVE('',#14654,#15289,#7951,.T.);
#18387=EDGE_CURVE('',#15290,#14647,#7952,.T.);
#18388=EDGE_CURVE('',#15289,#15286,#7953,.T.);
#18389=EDGE_CURVE('',#15287,#15288,#7954,.T.);
#18390=EDGE_CURVE('',#14652,#15285,#7955,.T.);
#18391=EDGE_CURVE('',#15286,#14653,#7956,.T.);
#18392=EDGE_CURVE('',#15297,#15298,#7957,.T.);
#18393=EDGE_CURVE('',#15299,#15297,#7958,.T.);
#18394=EDGE_CURVE('',#15298,#15299,#7959,.T.);
#18395=EDGE_CURVE('',#15300,#15301,#7960,.T.);
#18396=EDGE_CURVE('',#15302,#15300,#7961,.T.);
#18397=EDGE_CURVE('',#15301,#15302,#7962,.T.);
#18398=EDGE_CURVE('',#15303,#15304,#7963,.T.);
#18399=EDGE_CURVE('',#15305,#15303,#7964,.T.);
#18400=EDGE_CURVE('',#15304,#15305,#7965,.T.);
#18401=EDGE_CURVE('',#14658,#15305,#7966,.T.);
#18402=EDGE_CURVE('',#15303,#14659,#7967,.T.);
#18403=EDGE_CURVE('',#15306,#15307,#7968,.T.);
#18404=EDGE_CURVE('',#15308,#15306,#7969,.T.);
#18405=EDGE_CURVE('',#15307,#15308,#7970,.T.);
#18406=EDGE_CURVE('',#14656,#15308,#7971,.T.);
#18407=EDGE_CURVE('',#15306,#14657,#7972,.T.);
#18408=EDGE_CURVE('',#15300,#15307,#7973,.T.);
#18409=EDGE_CURVE('',#15308,#15302,#7974,.T.);
#18410=EDGE_CURVE('',#15307,#15304,#7975,.T.);
#18411=EDGE_CURVE('',#15305,#15306,#7976,.T.);
#18412=EDGE_CURVE('',#15297,#15303,#7977,.T.);
#18413=EDGE_CURVE('',#15304,#15299,#7978,.T.);
#18414=EDGE_CURVE('',#14662,#15301,#7979,.T.);
#18415=EDGE_CURVE('',#15302,#14655,#7980,.T.);
#18416=EDGE_CURVE('',#15301,#15298,#7981,.T.);
#18417=EDGE_CURVE('',#15299,#15300,#7982,.T.);
#18418=EDGE_CURVE('',#14660,#15297,#7983,.T.);
#18419=EDGE_CURVE('',#15298,#14661,#7984,.T.);
#18420=EDGE_CURVE('',#15309,#15310,#7985,.T.);
#18421=EDGE_CURVE('',#15310,#14669,#7986,.T.);
#18422=EDGE_CURVE('',#14668,#15311,#7987,.T.);
#18423=EDGE_CURVE('',#15311,#15309,#7988,.T.);
#18424=EDGE_CURVE('',#15312,#15310,#7989,.T.);
#18425=EDGE_CURVE('',#14670,#15312,#7990,.T.);
#18426=EDGE_CURVE('',#15313,#15309,#7991,.T.);
#18427=EDGE_CURVE('',#15313,#15314,#7992,.T.);
#18428=EDGE_CURVE('',#15314,#15312,#7993,.T.);
#18429=EDGE_CURVE('',#15311,#15315,#7994,.T.);
#18430=EDGE_CURVE('',#15315,#15316,#7995,.T.);
#18431=EDGE_CURVE('',#15316,#15313,#7996,.T.);
#18432=EDGE_CURVE('',#15317,#15314,#7997,.T.);
#18433=EDGE_CURVE('',#15312,#15317,#7998,.T.);
#18434=EDGE_CURVE('',#15318,#15315,#7999,.T.);
#18435=EDGE_CURVE('',#15316,#15318,#8000,.T.);
#18436=EDGE_CURVE('',#14666,#15318,#8001,.T.);
#18437=EDGE_CURVE('',#15315,#14667,#8002,.T.);
#18438=EDGE_CURVE('',#15319,#15320,#8003,.T.);
#18439=EDGE_CURVE('',#15321,#15319,#8004,.T.);
#18440=EDGE_CURVE('',#15320,#15321,#8005,.T.);
#18441=EDGE_CURVE('',#14664,#15321,#8006,.T.);
#18442=EDGE_CURVE('',#15319,#14665,#8007,.T.);
#18443=EDGE_CURVE('',#15314,#15320,#8008,.T.);
#18444=EDGE_CURVE('',#15321,#15317,#8009,.T.);
#18445=EDGE_CURVE('',#15320,#15316,#8010,.T.);
#18446=EDGE_CURVE('',#15318,#15319,#8011,.T.);
#18447=EDGE_CURVE('',#15317,#14663,#8012,.T.);
#18448=EDGE_CURVE('',#15322,#15323,#8013,.T.);
#18449=EDGE_CURVE('',#15324,#15322,#8014,.T.);
#18450=EDGE_CURVE('',#15323,#15324,#8015,.T.);
#18451=EDGE_CURVE('',#15325,#15326,#8016,.T.);
#18452=EDGE_CURVE('',#15327,#15325,#8017,.T.);
#18453=EDGE_CURVE('',#15326,#15327,#8018,.T.);
#18454=EDGE_CURVE('',#15328,#15329,#8019,.T.);
#18455=EDGE_CURVE('',#15330,#15328,#8020,.T.);
#18456=EDGE_CURVE('',#15329,#15330,#8021,.T.);
#18457=EDGE_CURVE('',#14674,#15330,#8022,.T.);
#18458=EDGE_CURVE('',#15328,#14675,#8023,.T.);
#18459=EDGE_CURVE('',#15331,#15332,#8024,.T.);
#18460=EDGE_CURVE('',#15333,#15331,#8025,.T.);
#18461=EDGE_CURVE('',#15332,#15333,#8026,.T.);
#18462=EDGE_CURVE('',#14672,#15333,#8027,.T.);
#18463=EDGE_CURVE('',#15331,#14673,#8028,.T.);
#18464=EDGE_CURVE('',#15325,#15332,#8029,.T.);
#18465=EDGE_CURVE('',#15333,#15327,#8030,.T.);
#18466=EDGE_CURVE('',#15332,#15329,#8031,.T.);
#18467=EDGE_CURVE('',#15330,#15331,#8032,.T.);
#18468=EDGE_CURVE('',#15322,#15328,#8033,.T.);
#18469=EDGE_CURVE('',#15329,#15324,#8034,.T.);
#18470=EDGE_CURVE('',#14678,#15326,#8035,.T.);
#18471=EDGE_CURVE('',#15327,#14671,#8036,.T.);
#18472=EDGE_CURVE('',#15326,#15323,#8037,.T.);
#18473=EDGE_CURVE('',#15324,#15325,#8038,.T.);
#18474=EDGE_CURVE('',#14676,#15322,#8039,.T.);
#18475=EDGE_CURVE('',#15323,#14677,#8040,.T.);
#18476=EDGE_CURVE('',#15334,#15335,#8041,.T.);
#18477=EDGE_CURVE('',#15336,#15334,#8042,.T.);
#18478=EDGE_CURVE('',#15335,#15336,#8043,.T.);
#18479=EDGE_CURVE('',#15337,#15338,#8044,.T.);
#18480=EDGE_CURVE('',#15338,#15336,#8045,.T.);
#18481=EDGE_CURVE('',#15334,#15339,#8046,.T.);
#18482=EDGE_CURVE('',#15339,#15337,#8047,.T.);
#18483=EDGE_CURVE('',#14686,#15335,#8048,.T.);
#18484=EDGE_CURVE('',#15336,#14679,#8049,.T.);
#18485=EDGE_CURVE('',#15340,#15341,#8050,.T.);
#18486=EDGE_CURVE('',#15342,#15340,#8051,.T.);
#18487=EDGE_CURVE('',#15341,#15342,#8052,.T.);
#18488=EDGE_CURVE('',#15343,#15344,#8053,.T.);
#18489=EDGE_CURVE('',#15344,#15342,#8054,.T.);
#18490=EDGE_CURVE('',#15340,#15345,#8055,.T.);
#18491=EDGE_CURVE('',#15345,#15343,#8056,.T.);
#18492=EDGE_CURVE('',#15335,#15341,#8057,.T.);
#18493=EDGE_CURVE('',#15342,#15334,#8058,.T.);
#18494=EDGE_CURVE('',#14684,#15340,#8059,.T.);
#18495=EDGE_CURVE('',#15341,#14685,#8060,.T.);
#18496=EDGE_CURVE('',#15337,#15346,#8061,.T.);
#18497=EDGE_CURVE('',#15346,#14681,#8062,.T.);
#18498=EDGE_CURVE('',#14680,#15338,#8063,.T.);
#18499=EDGE_CURVE('',#15339,#15344,#8064,.T.);
#18500=EDGE_CURVE('',#15347,#15343,#8065,.T.);
#18501=EDGE_CURVE('',#15347,#15346,#8066,.T.);
#18502=EDGE_CURVE('',#15345,#14683,#8067,.T.);
#18503=EDGE_CURVE('',#14682,#15347,#8068,.T.);
#18504=EDGE_CURVE('',#15348,#15349,#8069,.T.);
#18505=EDGE_CURVE('',#15350,#15348,#8070,.T.);
#18506=EDGE_CURVE('',#15349,#15350,#8071,.T.);
#18507=EDGE_CURVE('',#15351,#15352,#8072,.T.);
#18508=EDGE_CURVE('',#15353,#15351,#8073,.T.);
#18509=EDGE_CURVE('',#15352,#15353,#8074,.T.);
#18510=EDGE_CURVE('',#15354,#15355,#8075,.T.);
#18511=EDGE_CURVE('',#15356,#15354,#8076,.T.);
#18512=EDGE_CURVE('',#15355,#15356,#8077,.T.);
#18513=EDGE_CURVE('',#14690,#15356,#8078,.T.);
#18514=EDGE_CURVE('',#15354,#14691,#8079,.T.);
#18515=EDGE_CURVE('',#15357,#15358,#8080,.T.);
#18516=EDGE_CURVE('',#15359,#15357,#8081,.T.);
#18517=EDGE_CURVE('',#15358,#15359,#8082,.T.);
#18518=EDGE_CURVE('',#14688,#15359,#8083,.T.);
#18519=EDGE_CURVE('',#15357,#14689,#8084,.T.);
#18520=EDGE_CURVE('',#15351,#15358,#8085,.T.);
#18521=EDGE_CURVE('',#15359,#15353,#8086,.T.);
#18522=EDGE_CURVE('',#15358,#15355,#8087,.T.);
#18523=EDGE_CURVE('',#15356,#15357,#8088,.T.);
#18524=EDGE_CURVE('',#15348,#15354,#8089,.T.);
#18525=EDGE_CURVE('',#15355,#15350,#8090,.T.);
#18526=EDGE_CURVE('',#14694,#15352,#8091,.T.);
#18527=EDGE_CURVE('',#15353,#14687,#8092,.T.);
#18528=EDGE_CURVE('',#15352,#15349,#8093,.T.);
#18529=EDGE_CURVE('',#15350,#15351,#8094,.T.);
#18530=EDGE_CURVE('',#14692,#15348,#8095,.T.);
#18531=EDGE_CURVE('',#15349,#14693,#8096,.T.);
#18532=EDGE_CURVE('',#15360,#15361,#8097,.T.);
#18533=EDGE_CURVE('',#15362,#15360,#8098,.T.);
#18534=EDGE_CURVE('',#15361,#15362,#8099,.T.);
#18535=EDGE_CURVE('',#15363,#15364,#8100,.T.);
#18536=EDGE_CURVE('',#15365,#15363,#8101,.T.);
#18537=EDGE_CURVE('',#15364,#15365,#8102,.T.);
#18538=EDGE_CURVE('',#15366,#15367,#8103,.T.);
#18539=EDGE_CURVE('',#15368,#15366,#8104,.T.);
#18540=EDGE_CURVE('',#15367,#15368,#8105,.T.);
#18541=EDGE_CURVE('',#14698,#15368,#8106,.T.);
#18542=EDGE_CURVE('',#15366,#14699,#8107,.T.);
#18543=EDGE_CURVE('',#15369,#15370,#8108,.T.);
#18544=EDGE_CURVE('',#15371,#15369,#8109,.T.);
#18545=EDGE_CURVE('',#15370,#15371,#8110,.T.);
#18546=EDGE_CURVE('',#14696,#15371,#8111,.T.);
#18547=EDGE_CURVE('',#15369,#14697,#8112,.T.);
#18548=EDGE_CURVE('',#15363,#15370,#8113,.T.);
#18549=EDGE_CURVE('',#15371,#15365,#8114,.T.);
#18550=EDGE_CURVE('',#15370,#15367,#8115,.T.);
#18551=EDGE_CURVE('',#15368,#15369,#8116,.T.);
#18552=EDGE_CURVE('',#15360,#15366,#8117,.T.);
#18553=EDGE_CURVE('',#15367,#15362,#8118,.T.);
#18554=EDGE_CURVE('',#14702,#15364,#8119,.T.);
#18555=EDGE_CURVE('',#15365,#14695,#8120,.T.);
#18556=EDGE_CURVE('',#15364,#15361,#8121,.T.);
#18557=EDGE_CURVE('',#15362,#15363,#8122,.T.);
#18558=EDGE_CURVE('',#14700,#15360,#8123,.T.);
#18559=EDGE_CURVE('',#15361,#14701,#8124,.T.);
#18560=EDGE_CURVE('',#15372,#15373,#8125,.T.);
#18561=EDGE_CURVE('',#15373,#14709,#8126,.T.);
#18562=EDGE_CURVE('',#14708,#15374,#8127,.T.);
#18563=EDGE_CURVE('',#15374,#15372,#8128,.T.);
#18564=EDGE_CURVE('',#15375,#15373,#8129,.T.);
#18565=EDGE_CURVE('',#14710,#15375,#8130,.T.);
#18566=EDGE_CURVE('',#15376,#15372,#8131,.T.);
#18567=EDGE_CURVE('',#15376,#15377,#8132,.T.);
#18568=EDGE_CURVE('',#15377,#15375,#8133,.T.);
#18569=EDGE_CURVE('',#15374,#15378,#8134,.T.);
#18570=EDGE_CURVE('',#15378,#15379,#8135,.T.);
#18571=EDGE_CURVE('',#15379,#15376,#8136,.T.);
#18572=EDGE_CURVE('',#15380,#15377,#8137,.T.);
#18573=EDGE_CURVE('',#15375,#15380,#8138,.T.);
#18574=EDGE_CURVE('',#15381,#15378,#8139,.T.);
#18575=EDGE_CURVE('',#15379,#15381,#8140,.T.);
#18576=EDGE_CURVE('',#14706,#15381,#8141,.T.);
#18577=EDGE_CURVE('',#15378,#14707,#8142,.T.);
#18578=EDGE_CURVE('',#15382,#15383,#8143,.T.);
#18579=EDGE_CURVE('',#15384,#15382,#8144,.T.);
#18580=EDGE_CURVE('',#15383,#15384,#8145,.T.);
#18581=EDGE_CURVE('',#14704,#15384,#8146,.T.);
#18582=EDGE_CURVE('',#15382,#14705,#8147,.T.);
#18583=EDGE_CURVE('',#15377,#15383,#8148,.T.);
#18584=EDGE_CURVE('',#15384,#15380,#8149,.T.);
#18585=EDGE_CURVE('',#15383,#15379,#8150,.T.);
#18586=EDGE_CURVE('',#15381,#15382,#8151,.T.);
#18587=EDGE_CURVE('',#15380,#14703,#8152,.T.);
#18588=EDGE_CURVE('',#15385,#15386,#8153,.T.);
#18589=EDGE_CURVE('',#15387,#15385,#8154,.T.);
#18590=EDGE_CURVE('',#15386,#15387,#8155,.T.);
#18591=EDGE_CURVE('',#15388,#15389,#8156,.T.);
#18592=EDGE_CURVE('',#15390,#15388,#8157,.T.);
#18593=EDGE_CURVE('',#15389,#15390,#8158,.T.);
#18594=EDGE_CURVE('',#15391,#15392,#8159,.T.);
#18595=EDGE_CURVE('',#15393,#15391,#8160,.T.);
#18596=EDGE_CURVE('',#15392,#15393,#8161,.T.);
#18597=EDGE_CURVE('',#14714,#15393,#8162,.T.);
#18598=EDGE_CURVE('',#15391,#14715,#8163,.T.);
#18599=EDGE_CURVE('',#15394,#15395,#8164,.T.);
#18600=EDGE_CURVE('',#15396,#15394,#8165,.T.);
#18601=EDGE_CURVE('',#15395,#15396,#8166,.T.);
#18602=EDGE_CURVE('',#14712,#15396,#8167,.T.);
#18603=EDGE_CURVE('',#15394,#14713,#8168,.T.);
#18604=EDGE_CURVE('',#15388,#15395,#8169,.T.);
#18605=EDGE_CURVE('',#15396,#15390,#8170,.T.);
#18606=EDGE_CURVE('',#15395,#15392,#8171,.T.);
#18607=EDGE_CURVE('',#15393,#15394,#8172,.T.);
#18608=EDGE_CURVE('',#15385,#15391,#8173,.T.);
#18609=EDGE_CURVE('',#15392,#15387,#8174,.T.);
#18610=EDGE_CURVE('',#14718,#15389,#8175,.T.);
#18611=EDGE_CURVE('',#15390,#14711,#8176,.T.);
#18612=EDGE_CURVE('',#15389,#15386,#8177,.T.);
#18613=EDGE_CURVE('',#15387,#15388,#8178,.T.);
#18614=EDGE_CURVE('',#14716,#15385,#8179,.T.);
#18615=EDGE_CURVE('',#15386,#14717,#8180,.T.);
#18616=EDGE_CURVE('',#15397,#15398,#8181,.T.);
#18617=EDGE_CURVE('',#15399,#15397,#8182,.T.);
#18618=EDGE_CURVE('',#15398,#15399,#8183,.T.);
#18619=EDGE_CURVE('',#15400,#15401,#8184,.T.);
#18620=EDGE_CURVE('',#15401,#15399,#8185,.T.);
#18621=EDGE_CURVE('',#15397,#15402,#8186,.T.);
#18622=EDGE_CURVE('',#15402,#15400,#8187,.T.);
#18623=EDGE_CURVE('',#14726,#15398,#8188,.T.);
#18624=EDGE_CURVE('',#15399,#14719,#8189,.T.);
#18625=EDGE_CURVE('',#15403,#15404,#8190,.T.);
#18626=EDGE_CURVE('',#15405,#15403,#8191,.T.);
#18627=EDGE_CURVE('',#15404,#15405,#8192,.T.);
#18628=EDGE_CURVE('',#15406,#15407,#8193,.T.);
#18629=EDGE_CURVE('',#15407,#15405,#8194,.T.);
#18630=EDGE_CURVE('',#15403,#15408,#8195,.T.);
#18631=EDGE_CURVE('',#15408,#15406,#8196,.T.);
#18632=EDGE_CURVE('',#15398,#15404,#8197,.T.);
#18633=EDGE_CURVE('',#15405,#15397,#8198,.T.);
#18634=EDGE_CURVE('',#14724,#15403,#8199,.T.);
#18635=EDGE_CURVE('',#15404,#14725,#8200,.T.);
#18636=EDGE_CURVE('',#15400,#15409,#8201,.T.);
#18637=EDGE_CURVE('',#15409,#14721,#8202,.T.);
#18638=EDGE_CURVE('',#14720,#15401,#8203,.T.);
#18639=EDGE_CURVE('',#15402,#15407,#8204,.T.);
#18640=EDGE_CURVE('',#15410,#15406,#8205,.T.);
#18641=EDGE_CURVE('',#15410,#15409,#8206,.T.);
#18642=EDGE_CURVE('',#15408,#14723,#8207,.T.);
#18643=EDGE_CURVE('',#14722,#15410,#8208,.T.);
#18644=EDGE_CURVE('',#15411,#15412,#8209,.T.);
#18645=EDGE_CURVE('',#15413,#15411,#8210,.T.);
#18646=EDGE_CURVE('',#15412,#15413,#8211,.T.);
#18647=EDGE_CURVE('',#15414,#15415,#8212,.T.);
#18648=EDGE_CURVE('',#15416,#15414,#8213,.T.);
#18649=EDGE_CURVE('',#15415,#15416,#8214,.T.);
#18650=EDGE_CURVE('',#15417,#15418,#8215,.T.);
#18651=EDGE_CURVE('',#15419,#15417,#8216,.T.);
#18652=EDGE_CURVE('',#15418,#15419,#8217,.T.);
#18653=EDGE_CURVE('',#14579,#15419,#8218,.T.);
#18654=EDGE_CURVE('',#15417,#14580,#8219,.T.);
#18655=EDGE_CURVE('',#15420,#15421,#8220,.T.);
#18656=EDGE_CURVE('',#15422,#15420,#8221,.T.);
#18657=EDGE_CURVE('',#15421,#15422,#8222,.T.);
#18658=EDGE_CURVE('',#14575,#15422,#8223,.T.);
#18659=EDGE_CURVE('',#15420,#14576,#8224,.T.);
#18660=EDGE_CURVE('',#15414,#15421,#8225,.T.);
#18661=EDGE_CURVE('',#15422,#15416,#8226,.T.);
#18662=EDGE_CURVE('',#15421,#15418,#8227,.T.);
#18663=EDGE_CURVE('',#15419,#15420,#8228,.T.);
#18664=EDGE_CURVE('',#15411,#15417,#8229,.T.);
#18665=EDGE_CURVE('',#15418,#15413,#8230,.T.);
#18666=EDGE_CURVE('',#14573,#15415,#8231,.T.);
#18667=EDGE_CURVE('',#15416,#14574,#8232,.T.);
#18668=EDGE_CURVE('',#15415,#15412,#8233,.T.);
#18669=EDGE_CURVE('',#15413,#15414,#8234,.T.);
#18670=EDGE_CURVE('',#14581,#15411,#8235,.T.);
#18671=EDGE_CURVE('',#15412,#14582,#8236,.T.);
#18672=EDGE_CURVE('',#15423,#15424,#8237,.T.);
#18673=EDGE_CURVE('',#15425,#15423,#8238,.T.);
#18674=EDGE_CURVE('',#15424,#15425,#8239,.T.);
#18675=EDGE_CURVE('',#15426,#15427,#8240,.T.);
#18676=EDGE_CURVE('',#15428,#15426,#8241,.T.);
#18677=EDGE_CURVE('',#15427,#15428,#8242,.T.);
#18678=EDGE_CURVE('',#15429,#15430,#8243,.T.);
#18679=EDGE_CURVE('',#15431,#15429,#8244,.T.);
#18680=EDGE_CURVE('',#15430,#15431,#8245,.T.);
#18681=EDGE_CURVE('',#14730,#15431,#8246,.T.);
#18682=EDGE_CURVE('',#15429,#14731,#8247,.T.);
#18683=EDGE_CURVE('',#15432,#15433,#8248,.T.);
#18684=EDGE_CURVE('',#15434,#15432,#8249,.T.);
#18685=EDGE_CURVE('',#15433,#15434,#8250,.T.);
#18686=EDGE_CURVE('',#14728,#15434,#8251,.T.);
#18687=EDGE_CURVE('',#15432,#14729,#8252,.T.);
#18688=EDGE_CURVE('',#15426,#15433,#8253,.T.);
#18689=EDGE_CURVE('',#15434,#15428,#8254,.T.);
#18690=EDGE_CURVE('',#15433,#15430,#8255,.T.);
#18691=EDGE_CURVE('',#15431,#15432,#8256,.T.);
#18692=EDGE_CURVE('',#15423,#15429,#8257,.T.);
#18693=EDGE_CURVE('',#15430,#15425,#8258,.T.);
#18694=EDGE_CURVE('',#14734,#15427,#8259,.T.);
#18695=EDGE_CURVE('',#15428,#14727,#8260,.T.);
#18696=EDGE_CURVE('',#15427,#15424,#8261,.T.);
#18697=EDGE_CURVE('',#15425,#15426,#8262,.T.);
#18698=EDGE_CURVE('',#14732,#15423,#8263,.T.);
#18699=EDGE_CURVE('',#15424,#14733,#8264,.T.);
#18700=EDGE_CURVE('',#15435,#15436,#8265,.T.);
#18701=EDGE_CURVE('',#15436,#14741,#8266,.T.);
#18702=EDGE_CURVE('',#14740,#15437,#8267,.T.);
#18703=EDGE_CURVE('',#15437,#15435,#8268,.T.);
#18704=EDGE_CURVE('',#15438,#15436,#8269,.T.);
#18705=EDGE_CURVE('',#14742,#15438,#8270,.T.);
#18706=EDGE_CURVE('',#15439,#15435,#8271,.T.);
#18707=EDGE_CURVE('',#15439,#15440,#8272,.T.);
#18708=EDGE_CURVE('',#15440,#15438,#8273,.T.);
#18709=EDGE_CURVE('',#15437,#15441,#8274,.T.);
#18710=EDGE_CURVE('',#15441,#15442,#8275,.T.);
#18711=EDGE_CURVE('',#15442,#15439,#8276,.T.);
#18712=EDGE_CURVE('',#15443,#15440,#8277,.T.);
#18713=EDGE_CURVE('',#15438,#15443,#8278,.T.);
#18714=EDGE_CURVE('',#15444,#15441,#8279,.T.);
#18715=EDGE_CURVE('',#15442,#15444,#8280,.T.);
#18716=EDGE_CURVE('',#14738,#15444,#8281,.T.);
#18717=EDGE_CURVE('',#15441,#14739,#8282,.T.);
#18718=EDGE_CURVE('',#15445,#15446,#8283,.T.);
#18719=EDGE_CURVE('',#15447,#15445,#8284,.T.);
#18720=EDGE_CURVE('',#15446,#15447,#8285,.T.);
#18721=EDGE_CURVE('',#14736,#15447,#8286,.T.);
#18722=EDGE_CURVE('',#15445,#14737,#8287,.T.);
#18723=EDGE_CURVE('',#15440,#15446,#8288,.T.);
#18724=EDGE_CURVE('',#15447,#15443,#8289,.T.);
#18725=EDGE_CURVE('',#15446,#15442,#8290,.T.);
#18726=EDGE_CURVE('',#15444,#15445,#8291,.T.);
#18727=EDGE_CURVE('',#15443,#14735,#8292,.T.);
#18728=EDGE_CURVE('',#15448,#15449,#8293,.T.);
#18729=EDGE_CURVE('',#15450,#15448,#8294,.T.);
#18730=EDGE_CURVE('',#15449,#15450,#8295,.T.);
#18731=EDGE_CURVE('',#15451,#15452,#8296,.T.);
#18732=EDGE_CURVE('',#15453,#15451,#8297,.T.);
#18733=EDGE_CURVE('',#15452,#15453,#8298,.T.);
#18734=EDGE_CURVE('',#15454,#15455,#8299,.T.);
#18735=EDGE_CURVE('',#15456,#15454,#8300,.T.);
#18736=EDGE_CURVE('',#15455,#15456,#8301,.T.);
#18737=EDGE_CURVE('',#14746,#15456,#8302,.T.);
#18738=EDGE_CURVE('',#15454,#14747,#8303,.T.);
#18739=EDGE_CURVE('',#15457,#15458,#8304,.T.);
#18740=EDGE_CURVE('',#15459,#15457,#8305,.T.);
#18741=EDGE_CURVE('',#15458,#15459,#8306,.T.);
#18742=EDGE_CURVE('',#14744,#15459,#8307,.T.);
#18743=EDGE_CURVE('',#15457,#14745,#8308,.T.);
#18744=EDGE_CURVE('',#15451,#15458,#8309,.T.);
#18745=EDGE_CURVE('',#15459,#15453,#8310,.T.);
#18746=EDGE_CURVE('',#15458,#15455,#8311,.T.);
#18747=EDGE_CURVE('',#15456,#15457,#8312,.T.);
#18748=EDGE_CURVE('',#15448,#15454,#8313,.T.);
#18749=EDGE_CURVE('',#15455,#15450,#8314,.T.);
#18750=EDGE_CURVE('',#14750,#15452,#8315,.T.);
#18751=EDGE_CURVE('',#15453,#14743,#8316,.T.);
#18752=EDGE_CURVE('',#15452,#15449,#8317,.T.);
#18753=EDGE_CURVE('',#15450,#15451,#8318,.T.);
#18754=EDGE_CURVE('',#14748,#15448,#8319,.T.);
#18755=EDGE_CURVE('',#15449,#14749,#8320,.T.);
#18756=EDGE_CURVE('',#15460,#15461,#8321,.T.);
#18757=EDGE_CURVE('',#15462,#15460,#8322,.T.);
#18758=EDGE_CURVE('',#15461,#15462,#8323,.T.);
#18759=EDGE_CURVE('',#15463,#15464,#8324,.T.);
#18760=EDGE_CURVE('',#15464,#15462,#8325,.T.);
#18761=EDGE_CURVE('',#15460,#15465,#8326,.T.);
#18762=EDGE_CURVE('',#15465,#15463,#8327,.T.);
#18763=EDGE_CURVE('',#14758,#15461,#8328,.T.);
#18764=EDGE_CURVE('',#15462,#14751,#8329,.T.);
#18765=EDGE_CURVE('',#15466,#15467,#8330,.T.);
#18766=EDGE_CURVE('',#15468,#15466,#8331,.T.);
#18767=EDGE_CURVE('',#15467,#15468,#8332,.T.);
#18768=EDGE_CURVE('',#15469,#15470,#8333,.T.);
#18769=EDGE_CURVE('',#15470,#15468,#8334,.T.);
#18770=EDGE_CURVE('',#15466,#15471,#8335,.T.);
#18771=EDGE_CURVE('',#15471,#15469,#8336,.T.);
#18772=EDGE_CURVE('',#15461,#15467,#8337,.T.);
#18773=EDGE_CURVE('',#15468,#15460,#8338,.T.);
#18774=EDGE_CURVE('',#14756,#15466,#8339,.T.);
#18775=EDGE_CURVE('',#15467,#14757,#8340,.T.);
#18776=EDGE_CURVE('',#15463,#15472,#8341,.T.);
#18777=EDGE_CURVE('',#15472,#14753,#8342,.T.);
#18778=EDGE_CURVE('',#14752,#15464,#8343,.T.);
#18779=EDGE_CURVE('',#15465,#15470,#8344,.T.);
#18780=EDGE_CURVE('',#15473,#15469,#8345,.T.);
#18781=EDGE_CURVE('',#15473,#15472,#8346,.T.);
#18782=EDGE_CURVE('',#15471,#14755,#8347,.T.);
#18783=EDGE_CURVE('',#14754,#15473,#8348,.T.);
#18784=EDGE_CURVE('',#15474,#15475,#8349,.T.);
#18785=EDGE_CURVE('',#15476,#15474,#8350,.T.);
#18786=EDGE_CURVE('',#15475,#15476,#8351,.T.);
#18787=EDGE_CURVE('',#15477,#15478,#8352,.T.);
#18788=EDGE_CURVE('',#15479,#15477,#8353,.T.);
#18789=EDGE_CURVE('',#15478,#15479,#8354,.T.);
#18790=EDGE_CURVE('',#15480,#15481,#8355,.T.);
#18791=EDGE_CURVE('',#15482,#15480,#8356,.T.);
#18792=EDGE_CURVE('',#15481,#15482,#8357,.T.);
#18793=EDGE_CURVE('',#14762,#15482,#8358,.T.);
#18794=EDGE_CURVE('',#15480,#14763,#8359,.T.);
#18795=EDGE_CURVE('',#15483,#15484,#8360,.T.);
#18796=EDGE_CURVE('',#15485,#15483,#8361,.T.);
#18797=EDGE_CURVE('',#15484,#15485,#8362,.T.);
#18798=EDGE_CURVE('',#14760,#15485,#8363,.T.);
#18799=EDGE_CURVE('',#15483,#14761,#8364,.T.);
#18800=EDGE_CURVE('',#15477,#15484,#8365,.T.);
#18801=EDGE_CURVE('',#15485,#15479,#8366,.T.);
#18802=EDGE_CURVE('',#15484,#15481,#8367,.T.);
#18803=EDGE_CURVE('',#15482,#15483,#8368,.T.);
#18804=EDGE_CURVE('',#15474,#15480,#8369,.T.);
#18805=EDGE_CURVE('',#15481,#15476,#8370,.T.);
#18806=EDGE_CURVE('',#14766,#15478,#8371,.T.);
#18807=EDGE_CURVE('',#15479,#14759,#8372,.T.);
#18808=EDGE_CURVE('',#15478,#15475,#8373,.T.);
#18809=EDGE_CURVE('',#15476,#15477,#8374,.T.);
#18810=EDGE_CURVE('',#14764,#15474,#8375,.T.);
#18811=EDGE_CURVE('',#15475,#14765,#8376,.T.);
#18812=EDGE_CURVE('',#15486,#15487,#8377,.T.);
#18813=EDGE_CURVE('',#15488,#15486,#8378,.T.);
#18814=EDGE_CURVE('',#15487,#15488,#8379,.T.);
#18815=EDGE_CURVE('',#15489,#15490,#8380,.T.);
#18816=EDGE_CURVE('',#15491,#15489,#8381,.T.);
#18817=EDGE_CURVE('',#15490,#15491,#8382,.T.);
#18818=EDGE_CURVE('',#15492,#15493,#8383,.T.);
#18819=EDGE_CURVE('',#15494,#15492,#8384,.T.);
#18820=EDGE_CURVE('',#15493,#15494,#8385,.T.);
#18821=EDGE_CURVE('',#14770,#15494,#8386,.T.);
#18822=EDGE_CURVE('',#15492,#14771,#8387,.T.);
#18823=EDGE_CURVE('',#15495,#15496,#8388,.T.);
#18824=EDGE_CURVE('',#15497,#15495,#8389,.T.);
#18825=EDGE_CURVE('',#15496,#15497,#8390,.T.);
#18826=EDGE_CURVE('',#14768,#15497,#8391,.T.);
#18827=EDGE_CURVE('',#15495,#14769,#8392,.T.);
#18828=EDGE_CURVE('',#15489,#15496,#8393,.T.);
#18829=EDGE_CURVE('',#15497,#15491,#8394,.T.);
#18830=EDGE_CURVE('',#15496,#15493,#8395,.T.);
#18831=EDGE_CURVE('',#15494,#15495,#8396,.T.);
#18832=EDGE_CURVE('',#15486,#15492,#8397,.T.);
#18833=EDGE_CURVE('',#15493,#15488,#8398,.T.);
#18834=EDGE_CURVE('',#14774,#15490,#8399,.T.);
#18835=EDGE_CURVE('',#15491,#14767,#8400,.T.);
#18836=EDGE_CURVE('',#15490,#15487,#8401,.T.);
#18837=EDGE_CURVE('',#15488,#15489,#8402,.T.);
#18838=EDGE_CURVE('',#14772,#15486,#8403,.T.);
#18839=EDGE_CURVE('',#15487,#14773,#8404,.T.);
#18840=EDGE_CURVE('',#15498,#15499,#8405,.T.);
#18841=EDGE_CURVE('',#15499,#14781,#8406,.T.);
#18842=EDGE_CURVE('',#14780,#15500,#8407,.T.);
#18843=EDGE_CURVE('',#15500,#15498,#8408,.T.);
#18844=EDGE_CURVE('',#15501,#15499,#8409,.T.);
#18845=EDGE_CURVE('',#14782,#15501,#8410,.T.);
#18846=EDGE_CURVE('',#15502,#15498,#8411,.T.);
#18847=EDGE_CURVE('',#15502,#15503,#8412,.T.);
#18848=EDGE_CURVE('',#15503,#15501,#8413,.T.);
#18849=EDGE_CURVE('',#15500,#15504,#8414,.T.);
#18850=EDGE_CURVE('',#15504,#15505,#8415,.T.);
#18851=EDGE_CURVE('',#15505,#15502,#8416,.T.);
#18852=EDGE_CURVE('',#15506,#15503,#8417,.T.);
#18853=EDGE_CURVE('',#15501,#15506,#8418,.T.);
#18854=EDGE_CURVE('',#15507,#15504,#8419,.T.);
#18855=EDGE_CURVE('',#15505,#15507,#8420,.T.);
#18856=EDGE_CURVE('',#14778,#15507,#8421,.T.);
#18857=EDGE_CURVE('',#15504,#14779,#8422,.T.);
#18858=EDGE_CURVE('',#15508,#15509,#8423,.T.);
#18859=EDGE_CURVE('',#15510,#15508,#8424,.T.);
#18860=EDGE_CURVE('',#15509,#15510,#8425,.T.);
#18861=EDGE_CURVE('',#14776,#15510,#8426,.T.);
#18862=EDGE_CURVE('',#15508,#14777,#8427,.T.);
#18863=EDGE_CURVE('',#15503,#15509,#8428,.T.);
#18864=EDGE_CURVE('',#15510,#15506,#8429,.T.);
#18865=EDGE_CURVE('',#15509,#15505,#8430,.T.);
#18866=EDGE_CURVE('',#15507,#15508,#8431,.T.);
#18867=EDGE_CURVE('',#15506,#14775,#8432,.T.);
#18868=EDGE_CURVE('',#15511,#15512,#8433,.T.);
#18869=EDGE_CURVE('',#15513,#15511,#8434,.T.);
#18870=EDGE_CURVE('',#15512,#15513,#8435,.T.);
#18871=EDGE_CURVE('',#15514,#15515,#8436,.T.);
#18872=EDGE_CURVE('',#15516,#15514,#8437,.T.);
#18873=EDGE_CURVE('',#15515,#15516,#8438,.T.);
#18874=EDGE_CURVE('',#15517,#15518,#8439,.T.);
#18875=EDGE_CURVE('',#15519,#15517,#8440,.T.);
#18876=EDGE_CURVE('',#15518,#15519,#8441,.T.);
#18877=EDGE_CURVE('',#14786,#15519,#8442,.T.);
#18878=EDGE_CURVE('',#15517,#14787,#8443,.T.);
#18879=EDGE_CURVE('',#15520,#15521,#8444,.T.);
#18880=EDGE_CURVE('',#15522,#15520,#8445,.T.);
#18881=EDGE_CURVE('',#15521,#15522,#8446,.T.);
#18882=EDGE_CURVE('',#14784,#15522,#8447,.T.);
#18883=EDGE_CURVE('',#15520,#14785,#8448,.T.);
#18884=EDGE_CURVE('',#15514,#15521,#8449,.T.);
#18885=EDGE_CURVE('',#15522,#15516,#8450,.T.);
#18886=EDGE_CURVE('',#15521,#15518,#8451,.T.);
#18887=EDGE_CURVE('',#15519,#15520,#8452,.T.);
#18888=EDGE_CURVE('',#15511,#15517,#8453,.T.);
#18889=EDGE_CURVE('',#15518,#15513,#8454,.T.);
#18890=EDGE_CURVE('',#14790,#15515,#8455,.T.);
#18891=EDGE_CURVE('',#15516,#14783,#8456,.T.);
#18892=EDGE_CURVE('',#15515,#15512,#8457,.T.);
#18893=EDGE_CURVE('',#15513,#15514,#8458,.T.);
#18894=EDGE_CURVE('',#14788,#15511,#8459,.T.);
#18895=EDGE_CURVE('',#15512,#14789,#8460,.T.);
#18896=EDGE_CURVE('',#15523,#15524,#8461,.T.);
#18897=EDGE_CURVE('',#15525,#15523,#8462,.T.);
#18898=EDGE_CURVE('',#15524,#15525,#8463,.T.);
#18899=EDGE_CURVE('',#15526,#15527,#8464,.T.);
#18900=EDGE_CURVE('',#15527,#15525,#8465,.T.);
#18901=EDGE_CURVE('',#15523,#15528,#8466,.T.);
#18902=EDGE_CURVE('',#15528,#15526,#8467,.T.);
#18903=EDGE_CURVE('',#14798,#15524,#8468,.T.);
#18904=EDGE_CURVE('',#15525,#14791,#8469,.T.);
#18905=EDGE_CURVE('',#15529,#15530,#8470,.T.);
#18906=EDGE_CURVE('',#15531,#15529,#8471,.T.);
#18907=EDGE_CURVE('',#15530,#15531,#8472,.T.);
#18908=EDGE_CURVE('',#15532,#15533,#8473,.T.);
#18909=EDGE_CURVE('',#15533,#15531,#8474,.T.);
#18910=EDGE_CURVE('',#15529,#15534,#8475,.T.);
#18911=EDGE_CURVE('',#15534,#15532,#8476,.T.);
#18912=EDGE_CURVE('',#15524,#15530,#8477,.T.);
#18913=EDGE_CURVE('',#15531,#15523,#8478,.T.);
#18914=EDGE_CURVE('',#14796,#15529,#8479,.T.);
#18915=EDGE_CURVE('',#15530,#14797,#8480,.T.);
#18916=EDGE_CURVE('',#15526,#15535,#8481,.T.);
#18917=EDGE_CURVE('',#15535,#14793,#8482,.T.);
#18918=EDGE_CURVE('',#14792,#15527,#8483,.T.);
#18919=EDGE_CURVE('',#15528,#15533,#8484,.T.);
#18920=EDGE_CURVE('',#15536,#15532,#8485,.T.);
#18921=EDGE_CURVE('',#15536,#15535,#8486,.T.);
#18922=EDGE_CURVE('',#15534,#14795,#8487,.T.);
#18923=EDGE_CURVE('',#14794,#15536,#8488,.T.);
#18924=EDGE_CURVE('',#15537,#15538,#8489,.T.);
#18925=EDGE_CURVE('',#15539,#15537,#8490,.T.);
#18926=EDGE_CURVE('',#15538,#15539,#8491,.T.);
#18927=EDGE_CURVE('',#15540,#15541,#8492,.T.);
#18928=EDGE_CURVE('',#15542,#15540,#8493,.T.);
#18929=EDGE_CURVE('',#15541,#15542,#8494,.T.);
#18930=EDGE_CURVE('',#15543,#15544,#8495,.T.);
#18931=EDGE_CURVE('',#15545,#15543,#8496,.T.);
#18932=EDGE_CURVE('',#15544,#15545,#8497,.T.);
#18933=EDGE_CURVE('',#14802,#15545,#8498,.T.);
#18934=EDGE_CURVE('',#15543,#14803,#8499,.T.);
#18935=EDGE_CURVE('',#15546,#15547,#8500,.T.);
#18936=EDGE_CURVE('',#15548,#15546,#8501,.T.);
#18937=EDGE_CURVE('',#15547,#15548,#8502,.T.);
#18938=EDGE_CURVE('',#14800,#15548,#8503,.T.);
#18939=EDGE_CURVE('',#15546,#14801,#8504,.T.);
#18940=EDGE_CURVE('',#15540,#15547,#8505,.T.);
#18941=EDGE_CURVE('',#15548,#15542,#8506,.T.);
#18942=EDGE_CURVE('',#15547,#15544,#8507,.T.);
#18943=EDGE_CURVE('',#15545,#15546,#8508,.T.);
#18944=EDGE_CURVE('',#15537,#15543,#8509,.T.);
#18945=EDGE_CURVE('',#15544,#15539,#8510,.T.);
#18946=EDGE_CURVE('',#14806,#15541,#8511,.T.);
#18947=EDGE_CURVE('',#15542,#14799,#8512,.T.);
#18948=EDGE_CURVE('',#15541,#15538,#8513,.T.);
#18949=EDGE_CURVE('',#15539,#15540,#8514,.T.);
#18950=EDGE_CURVE('',#14804,#15537,#8515,.T.);
#18951=EDGE_CURVE('',#15538,#14805,#8516,.T.);
#18952=EDGE_CURVE('',#15549,#15550,#8517,.T.);
#18953=EDGE_CURVE('',#15551,#15549,#8518,.T.);
#18954=EDGE_CURVE('',#15550,#15551,#8519,.T.);
#18955=EDGE_CURVE('',#15552,#15553,#8520,.T.);
#18956=EDGE_CURVE('',#15554,#15552,#8521,.T.);
#18957=EDGE_CURVE('',#15553,#15554,#8522,.T.);
#18958=EDGE_CURVE('',#15555,#15556,#8523,.T.);
#18959=EDGE_CURVE('',#15557,#15555,#8524,.T.);
#18960=EDGE_CURVE('',#15556,#15557,#8525,.T.);
#18961=EDGE_CURVE('',#14810,#15557,#8526,.T.);
#18962=EDGE_CURVE('',#15555,#14811,#8527,.T.);
#18963=EDGE_CURVE('',#15558,#15559,#8528,.T.);
#18964=EDGE_CURVE('',#15560,#15558,#8529,.T.);
#18965=EDGE_CURVE('',#15559,#15560,#8530,.T.);
#18966=EDGE_CURVE('',#14808,#15560,#8531,.T.);
#18967=EDGE_CURVE('',#15558,#14809,#8532,.T.);
#18968=EDGE_CURVE('',#15552,#15559,#8533,.T.);
#18969=EDGE_CURVE('',#15560,#15554,#8534,.T.);
#18970=EDGE_CURVE('',#15559,#15556,#8535,.T.);
#18971=EDGE_CURVE('',#15557,#15558,#8536,.T.);
#18972=EDGE_CURVE('',#15549,#15555,#8537,.T.);
#18973=EDGE_CURVE('',#15556,#15551,#8538,.T.);
#18974=EDGE_CURVE('',#14814,#15553,#8539,.T.);
#18975=EDGE_CURVE('',#15554,#14807,#8540,.T.);
#18976=EDGE_CURVE('',#15553,#15550,#8541,.T.);
#18977=EDGE_CURVE('',#15551,#15552,#8542,.T.);
#18978=EDGE_CURVE('',#14812,#15549,#8543,.T.);
#18979=EDGE_CURVE('',#15550,#14813,#8544,.T.);
#18980=EDGE_CURVE('',#15561,#15562,#8545,.T.);
#18981=EDGE_CURVE('',#15562,#14821,#8546,.T.);
#18982=EDGE_CURVE('',#14820,#15563,#8547,.T.);
#18983=EDGE_CURVE('',#15563,#15561,#8548,.T.);
#18984=EDGE_CURVE('',#15564,#15562,#8549,.T.);
#18985=EDGE_CURVE('',#14822,#15564,#8550,.T.);
#18986=EDGE_CURVE('',#15565,#15561,#8551,.T.);
#18987=EDGE_CURVE('',#15565,#15566,#8552,.T.);
#18988=EDGE_CURVE('',#15566,#15564,#8553,.T.);
#18989=EDGE_CURVE('',#15563,#15567,#8554,.T.);
#18990=EDGE_CURVE('',#15567,#15568,#8555,.T.);
#18991=EDGE_CURVE('',#15568,#15565,#8556,.T.);
#18992=EDGE_CURVE('',#15569,#15566,#8557,.T.);
#18993=EDGE_CURVE('',#15564,#15569,#8558,.T.);
#18994=EDGE_CURVE('',#15570,#15567,#8559,.T.);
#18995=EDGE_CURVE('',#15568,#15570,#8560,.T.);
#18996=EDGE_CURVE('',#14818,#15570,#8561,.T.);
#18997=EDGE_CURVE('',#15567,#14819,#8562,.T.);
#18998=EDGE_CURVE('',#15571,#15572,#8563,.T.);
#18999=EDGE_CURVE('',#15573,#15571,#8564,.T.);
#19000=EDGE_CURVE('',#15572,#15573,#8565,.T.);
#19001=EDGE_CURVE('',#14816,#15573,#8566,.T.);
#19002=EDGE_CURVE('',#15571,#14817,#8567,.T.);
#19003=EDGE_CURVE('',#15566,#15572,#8568,.T.);
#19004=EDGE_CURVE('',#15573,#15569,#8569,.T.);
#19005=EDGE_CURVE('',#15572,#15568,#8570,.T.);
#19006=EDGE_CURVE('',#15570,#15571,#8571,.T.);
#19007=EDGE_CURVE('',#15569,#14815,#8572,.T.);
#19008=EDGE_CURVE('',#15574,#15575,#8573,.T.);
#19009=EDGE_CURVE('',#15576,#15574,#8574,.T.);
#19010=EDGE_CURVE('',#15575,#15576,#8575,.T.);
#19011=EDGE_CURVE('',#15577,#15578,#8576,.T.);
#19012=EDGE_CURVE('',#15579,#15577,#8577,.T.);
#19013=EDGE_CURVE('',#15578,#15579,#8578,.T.);
#19014=EDGE_CURVE('',#15580,#15581,#8579,.T.);
#19015=EDGE_CURVE('',#15582,#15580,#8580,.T.);
#19016=EDGE_CURVE('',#15581,#15582,#8581,.T.);
#19017=EDGE_CURVE('',#14826,#15582,#8582,.T.);
#19018=EDGE_CURVE('',#15580,#14827,#8583,.T.);
#19019=EDGE_CURVE('',#15583,#15584,#8584,.T.);
#19020=EDGE_CURVE('',#15585,#15583,#8585,.T.);
#19021=EDGE_CURVE('',#15584,#15585,#8586,.T.);
#19022=EDGE_CURVE('',#14824,#15585,#8587,.T.);
#19023=EDGE_CURVE('',#15583,#14825,#8588,.T.);
#19024=EDGE_CURVE('',#15577,#15584,#8589,.T.);
#19025=EDGE_CURVE('',#15585,#15579,#8590,.T.);
#19026=EDGE_CURVE('',#15584,#15581,#8591,.T.);
#19027=EDGE_CURVE('',#15582,#15583,#8592,.T.);
#19028=EDGE_CURVE('',#15574,#15580,#8593,.T.);
#19029=EDGE_CURVE('',#15581,#15576,#8594,.T.);
#19030=EDGE_CURVE('',#14830,#15578,#8595,.T.);
#19031=EDGE_CURVE('',#15579,#14823,#8596,.T.);
#19032=EDGE_CURVE('',#15578,#15575,#8597,.T.);
#19033=EDGE_CURVE('',#15576,#15577,#8598,.T.);
#19034=EDGE_CURVE('',#14828,#15574,#8599,.T.);
#19035=EDGE_CURVE('',#15575,#14829,#8600,.T.);
#19036=EDGE_CURVE('',#15586,#15587,#8601,.T.);
#19037=EDGE_CURVE('',#15588,#15586,#8602,.T.);
#19038=EDGE_CURVE('',#15587,#15588,#8603,.T.);
#19039=EDGE_CURVE('',#15589,#15590,#8604,.T.);
#19040=EDGE_CURVE('',#15590,#15588,#8605,.T.);
#19041=EDGE_CURVE('',#15586,#15591,#8606,.T.);
#19042=EDGE_CURVE('',#15591,#15589,#8607,.T.);
#19043=EDGE_CURVE('',#14838,#15587,#8608,.T.);
#19044=EDGE_CURVE('',#15588,#14831,#8609,.T.);
#19045=EDGE_CURVE('',#15592,#15593,#8610,.T.);
#19046=EDGE_CURVE('',#15594,#15592,#8611,.T.);
#19047=EDGE_CURVE('',#15593,#15594,#8612,.T.);
#19048=EDGE_CURVE('',#15595,#15596,#8613,.T.);
#19049=EDGE_CURVE('',#15596,#15594,#8614,.T.);
#19050=EDGE_CURVE('',#15592,#15597,#8615,.T.);
#19051=EDGE_CURVE('',#15597,#15595,#8616,.T.);
#19052=EDGE_CURVE('',#15587,#15593,#8617,.T.);
#19053=EDGE_CURVE('',#15594,#15586,#8618,.T.);
#19054=EDGE_CURVE('',#14836,#15592,#8619,.T.);
#19055=EDGE_CURVE('',#15593,#14837,#8620,.T.);
#19056=EDGE_CURVE('',#15589,#15598,#8621,.T.);
#19057=EDGE_CURVE('',#15598,#14833,#8622,.T.);
#19058=EDGE_CURVE('',#14832,#15590,#8623,.T.);
#19059=EDGE_CURVE('',#15591,#15596,#8624,.T.);
#19060=EDGE_CURVE('',#15599,#15595,#8625,.T.);
#19061=EDGE_CURVE('',#15599,#15598,#8626,.T.);
#19062=EDGE_CURVE('',#15597,#14835,#8627,.T.);
#19063=EDGE_CURVE('',#14834,#15599,#8628,.T.);
#19064=EDGE_CURVE('',#15600,#15601,#8629,.T.);
#19065=EDGE_CURVE('',#15602,#15600,#8630,.T.);
#19066=EDGE_CURVE('',#15601,#15602,#8631,.T.);
#19067=EDGE_CURVE('',#15603,#15604,#8632,.T.);
#19068=EDGE_CURVE('',#15605,#15603,#8633,.T.);
#19069=EDGE_CURVE('',#15604,#15605,#8634,.T.);
#19070=EDGE_CURVE('',#15606,#15607,#8635,.T.);
#19071=EDGE_CURVE('',#15608,#15606,#8636,.T.);
#19072=EDGE_CURVE('',#15607,#15608,#8637,.T.);
#19073=EDGE_CURVE('',#14842,#15608,#8638,.T.);
#19074=EDGE_CURVE('',#15606,#14843,#8639,.T.);
#19075=EDGE_CURVE('',#15609,#15610,#8640,.T.);
#19076=EDGE_CURVE('',#15611,#15609,#8641,.T.);
#19077=EDGE_CURVE('',#15610,#15611,#8642,.T.);
#19078=EDGE_CURVE('',#14840,#15611,#8643,.T.);
#19079=EDGE_CURVE('',#15609,#14841,#8644,.T.);
#19080=EDGE_CURVE('',#15603,#15610,#8645,.T.);
#19081=EDGE_CURVE('',#15611,#15605,#8646,.T.);
#19082=EDGE_CURVE('',#15610,#15607,#8647,.T.);
#19083=EDGE_CURVE('',#15608,#15609,#8648,.T.);
#19084=EDGE_CURVE('',#15600,#15606,#8649,.T.);
#19085=EDGE_CURVE('',#15607,#15602,#8650,.T.);
#19086=EDGE_CURVE('',#14846,#15604,#8651,.T.);
#19087=EDGE_CURVE('',#15605,#14839,#8652,.T.);
#19088=EDGE_CURVE('',#15604,#15601,#8653,.T.);
#19089=EDGE_CURVE('',#15602,#15603,#8654,.T.);
#19090=EDGE_CURVE('',#14844,#15600,#8655,.T.);
#19091=EDGE_CURVE('',#15601,#14845,#8656,.T.);
#19092=EDGE_CURVE('',#15612,#15613,#8657,.T.);
#19093=EDGE_CURVE('',#15614,#15612,#8658,.T.);
#19094=EDGE_CURVE('',#15613,#15614,#8659,.T.);
#19095=EDGE_CURVE('',#15615,#15616,#8660,.T.);
#19096=EDGE_CURVE('',#15617,#15615,#8661,.T.);
#19097=EDGE_CURVE('',#15616,#15617,#8662,.T.);
#19098=EDGE_CURVE('',#15618,#15619,#8663,.T.);
#19099=EDGE_CURVE('',#15620,#15618,#8664,.T.);
#19100=EDGE_CURVE('',#15619,#15620,#8665,.T.);
#19101=EDGE_CURVE('',#14850,#15620,#8666,.T.);
#19102=EDGE_CURVE('',#15618,#14851,#8667,.T.);
#19103=EDGE_CURVE('',#15621,#15622,#8668,.T.);
#19104=EDGE_CURVE('',#15623,#15621,#8669,.T.);
#19105=EDGE_CURVE('',#15622,#15623,#8670,.T.);
#19106=EDGE_CURVE('',#14848,#15623,#8671,.T.);
#19107=EDGE_CURVE('',#15621,#14849,#8672,.T.);
#19108=EDGE_CURVE('',#15615,#15622,#8673,.T.);
#19109=EDGE_CURVE('',#15623,#15617,#8674,.T.);
#19110=EDGE_CURVE('',#15622,#15619,#8675,.T.);
#19111=EDGE_CURVE('',#15620,#15621,#8676,.T.);
#19112=EDGE_CURVE('',#15612,#15618,#8677,.T.);
#19113=EDGE_CURVE('',#15619,#15614,#8678,.T.);
#19114=EDGE_CURVE('',#14854,#15616,#8679,.T.);
#19115=EDGE_CURVE('',#15617,#14847,#8680,.T.);
#19116=EDGE_CURVE('',#15616,#15613,#8681,.T.);
#19117=EDGE_CURVE('',#15614,#15615,#8682,.T.);
#19118=EDGE_CURVE('',#14852,#15612,#8683,.T.);
#19119=EDGE_CURVE('',#15613,#14853,#8684,.T.);
#19120=EDGE_CURVE('',#15624,#15625,#8685,.T.);
#19121=EDGE_CURVE('',#15625,#14861,#8686,.T.);
#19122=EDGE_CURVE('',#14860,#15626,#8687,.T.);
#19123=EDGE_CURVE('',#15626,#15624,#8688,.T.);
#19124=EDGE_CURVE('',#15627,#15625,#8689,.T.);
#19125=EDGE_CURVE('',#14862,#15627,#8690,.T.);
#19126=EDGE_CURVE('',#15628,#15624,#8691,.T.);
#19127=EDGE_CURVE('',#15628,#15629,#8692,.T.);
#19128=EDGE_CURVE('',#15629,#15627,#8693,.T.);
#19129=EDGE_CURVE('',#15626,#15630,#8694,.T.);
#19130=EDGE_CURVE('',#15630,#15631,#8695,.T.);
#19131=EDGE_CURVE('',#15631,#15628,#8696,.T.);
#19132=EDGE_CURVE('',#15632,#15629,#8697,.T.);
#19133=EDGE_CURVE('',#15627,#15632,#8698,.T.);
#19134=EDGE_CURVE('',#15633,#15630,#8699,.T.);
#19135=EDGE_CURVE('',#15631,#15633,#8700,.T.);
#19136=EDGE_CURVE('',#14858,#15633,#8701,.T.);
#19137=EDGE_CURVE('',#15630,#14859,#8702,.T.);
#19138=EDGE_CURVE('',#15634,#15635,#8703,.T.);
#19139=EDGE_CURVE('',#15636,#15634,#8704,.T.);
#19140=EDGE_CURVE('',#15635,#15636,#8705,.T.);
#19141=EDGE_CURVE('',#14856,#15636,#8706,.T.);
#19142=EDGE_CURVE('',#15634,#14857,#8707,.T.);
#19143=EDGE_CURVE('',#15629,#15635,#8708,.T.);
#19144=EDGE_CURVE('',#15636,#15632,#8709,.T.);
#19145=EDGE_CURVE('',#15635,#15631,#8710,.T.);
#19146=EDGE_CURVE('',#15633,#15634,#8711,.T.);
#19147=EDGE_CURVE('',#15632,#14855,#8712,.T.);
#19148=EDGE_CURVE('',#15637,#15638,#8713,.T.);
#19149=EDGE_CURVE('',#15639,#15637,#8714,.T.);
#19150=EDGE_CURVE('',#15638,#15639,#8715,.T.);
#19151=EDGE_CURVE('',#15640,#15641,#8716,.T.);
#19152=EDGE_CURVE('',#15642,#15640,#8717,.T.);
#19153=EDGE_CURVE('',#15641,#15642,#8718,.T.);
#19154=EDGE_CURVE('',#15643,#15644,#8719,.T.);
#19155=EDGE_CURVE('',#15645,#15643,#8720,.T.);
#19156=EDGE_CURVE('',#15644,#15645,#8721,.T.);
#19157=EDGE_CURVE('',#14866,#15645,#8722,.T.);
#19158=EDGE_CURVE('',#15643,#14867,#8723,.T.);
#19159=EDGE_CURVE('',#15646,#15647,#8724,.T.);
#19160=EDGE_CURVE('',#15648,#15646,#8725,.T.);
#19161=EDGE_CURVE('',#15647,#15648,#8726,.T.);
#19162=EDGE_CURVE('',#14864,#15648,#8727,.T.);
#19163=EDGE_CURVE('',#15646,#14865,#8728,.T.);
#19164=EDGE_CURVE('',#15640,#15647,#8729,.T.);
#19165=EDGE_CURVE('',#15648,#15642,#8730,.T.);
#19166=EDGE_CURVE('',#15647,#15644,#8731,.T.);
#19167=EDGE_CURVE('',#15645,#15646,#8732,.T.);
#19168=EDGE_CURVE('',#15637,#15643,#8733,.T.);
#19169=EDGE_CURVE('',#15644,#15639,#8734,.T.);
#19170=EDGE_CURVE('',#14870,#15641,#8735,.T.);
#19171=EDGE_CURVE('',#15642,#14863,#8736,.T.);
#19172=EDGE_CURVE('',#15641,#15638,#8737,.T.);
#19173=EDGE_CURVE('',#15639,#15640,#8738,.T.);
#19174=EDGE_CURVE('',#14868,#15637,#8739,.T.);
#19175=EDGE_CURVE('',#15638,#14869,#8740,.T.);
#19176=EDGE_CURVE('',#15649,#15650,#8741,.T.);
#19177=EDGE_CURVE('',#15651,#15649,#8742,.T.);
#19178=EDGE_CURVE('',#15650,#15651,#8743,.T.);
#19179=EDGE_CURVE('',#15652,#15653,#8744,.T.);
#19180=EDGE_CURVE('',#15653,#15651,#8745,.T.);
#19181=EDGE_CURVE('',#15649,#15654,#8746,.T.);
#19182=EDGE_CURVE('',#15654,#15652,#8747,.T.);
#19183=EDGE_CURVE('',#14878,#15650,#8748,.T.);
#19184=EDGE_CURVE('',#15651,#14871,#8749,.T.);
#19185=EDGE_CURVE('',#15655,#15656,#8750,.T.);
#19186=EDGE_CURVE('',#15657,#15655,#8751,.T.);
#19187=EDGE_CURVE('',#15656,#15657,#8752,.T.);
#19188=EDGE_CURVE('',#15658,#15659,#8753,.T.);
#19189=EDGE_CURVE('',#15659,#15657,#8754,.T.);
#19190=EDGE_CURVE('',#15655,#15660,#8755,.T.);
#19191=EDGE_CURVE('',#15660,#15658,#8756,.T.);
#19192=EDGE_CURVE('',#15650,#15656,#8757,.T.);
#19193=EDGE_CURVE('',#15657,#15649,#8758,.T.);
#19194=EDGE_CURVE('',#14876,#15655,#8759,.T.);
#19195=EDGE_CURVE('',#15656,#14877,#8760,.T.);
#19196=EDGE_CURVE('',#15652,#15661,#8761,.T.);
#19197=EDGE_CURVE('',#15661,#14873,#8762,.T.);
#19198=EDGE_CURVE('',#14872,#15653,#8763,.T.);
#19199=EDGE_CURVE('',#15654,#15659,#8764,.T.);
#19200=EDGE_CURVE('',#15662,#15658,#8765,.T.);
#19201=EDGE_CURVE('',#15662,#15661,#8766,.T.);
#19202=EDGE_CURVE('',#15660,#14875,#8767,.T.);
#19203=EDGE_CURVE('',#14874,#15662,#8768,.T.);
#19204=EDGE_CURVE('',#15663,#15664,#8769,.T.);
#19205=EDGE_CURVE('',#15665,#15663,#8770,.T.);
#19206=EDGE_CURVE('',#15664,#15665,#8771,.T.);
#19207=EDGE_CURVE('',#15666,#15667,#8772,.T.);
#19208=EDGE_CURVE('',#15668,#15666,#8773,.T.);
#19209=EDGE_CURVE('',#15667,#15668,#8774,.T.);
#19210=EDGE_CURVE('',#15669,#15670,#8775,.T.);
#19211=EDGE_CURVE('',#15671,#15669,#8776,.T.);
#19212=EDGE_CURVE('',#15670,#15671,#8777,.T.);
#19213=EDGE_CURVE('',#14882,#15671,#8778,.T.);
#19214=EDGE_CURVE('',#15669,#14883,#8779,.T.);
#19215=EDGE_CURVE('',#15672,#15673,#8780,.T.);
#19216=EDGE_CURVE('',#15674,#15672,#8781,.T.);
#19217=EDGE_CURVE('',#15673,#15674,#8782,.T.);
#19218=EDGE_CURVE('',#14880,#15674,#8783,.T.);
#19219=EDGE_CURVE('',#15672,#14881,#8784,.T.);
#19220=EDGE_CURVE('',#15666,#15673,#8785,.T.);
#19221=EDGE_CURVE('',#15674,#15668,#8786,.T.);
#19222=EDGE_CURVE('',#15673,#15670,#8787,.T.);
#19223=EDGE_CURVE('',#15671,#15672,#8788,.T.);
#19224=EDGE_CURVE('',#15663,#15669,#8789,.T.);
#19225=EDGE_CURVE('',#15670,#15665,#8790,.T.);
#19226=EDGE_CURVE('',#14886,#15667,#8791,.T.);
#19227=EDGE_CURVE('',#15668,#14879,#8792,.T.);
#19228=EDGE_CURVE('',#15667,#15664,#8793,.T.);
#19229=EDGE_CURVE('',#15665,#15666,#8794,.T.);
#19230=EDGE_CURVE('',#14884,#15663,#8795,.T.);
#19231=EDGE_CURVE('',#15664,#14885,#8796,.T.);
#19232=EDGE_CURVE('',#15675,#15676,#8797,.T.);
#19233=EDGE_CURVE('',#15677,#15675,#8798,.T.);
#19234=EDGE_CURVE('',#15676,#15677,#8799,.T.);
#19235=EDGE_CURVE('',#15678,#15679,#8800,.T.);
#19236=EDGE_CURVE('',#15680,#15678,#8801,.T.);
#19237=EDGE_CURVE('',#15679,#15680,#8802,.T.);
#19238=EDGE_CURVE('',#15681,#15682,#8803,.T.);
#19239=EDGE_CURVE('',#15683,#15681,#8804,.T.);
#19240=EDGE_CURVE('',#15682,#15683,#8805,.T.);
#19241=EDGE_CURVE('',#14890,#15683,#8806,.T.);
#19242=EDGE_CURVE('',#15681,#14891,#8807,.T.);
#19243=EDGE_CURVE('',#15684,#15685,#8808,.T.);
#19244=EDGE_CURVE('',#15686,#15684,#8809,.T.);
#19245=EDGE_CURVE('',#15685,#15686,#8810,.T.);
#19246=EDGE_CURVE('',#14888,#15686,#8811,.T.);
#19247=EDGE_CURVE('',#15684,#14889,#8812,.T.);
#19248=EDGE_CURVE('',#15678,#15685,#8813,.T.);
#19249=EDGE_CURVE('',#15686,#15680,#8814,.T.);
#19250=EDGE_CURVE('',#15685,#15682,#8815,.T.);
#19251=EDGE_CURVE('',#15683,#15684,#8816,.T.);
#19252=EDGE_CURVE('',#15675,#15681,#8817,.T.);
#19253=EDGE_CURVE('',#15682,#15677,#8818,.T.);
#19254=EDGE_CURVE('',#14894,#15679,#8819,.T.);
#19255=EDGE_CURVE('',#15680,#14887,#8820,.T.);
#19256=EDGE_CURVE('',#15679,#15676,#8821,.T.);
#19257=EDGE_CURVE('',#15677,#15678,#8822,.T.);
#19258=EDGE_CURVE('',#14892,#15675,#8823,.T.);
#19259=EDGE_CURVE('',#15676,#14893,#8824,.T.);
#19260=EDGE_CURVE('',#15687,#15688,#8825,.T.);
#19261=EDGE_CURVE('',#15688,#14901,#8826,.T.);
#19262=EDGE_CURVE('',#14900,#15689,#8827,.T.);
#19263=EDGE_CURVE('',#15689,#15687,#8828,.T.);
#19264=EDGE_CURVE('',#15690,#15688,#8829,.T.);
#19265=EDGE_CURVE('',#14902,#15690,#8830,.T.);
#19266=EDGE_CURVE('',#15691,#15687,#8831,.T.);
#19267=EDGE_CURVE('',#15691,#15692,#8832,.T.);
#19268=EDGE_CURVE('',#15692,#15690,#8833,.T.);
#19269=EDGE_CURVE('',#15689,#15693,#8834,.T.);
#19270=EDGE_CURVE('',#15693,#15694,#8835,.T.);
#19271=EDGE_CURVE('',#15694,#15691,#8836,.T.);
#19272=EDGE_CURVE('',#15695,#15692,#8837,.T.);
#19273=EDGE_CURVE('',#15690,#15695,#8838,.T.);
#19274=EDGE_CURVE('',#15696,#15693,#8839,.T.);
#19275=EDGE_CURVE('',#15694,#15696,#8840,.T.);
#19276=EDGE_CURVE('',#14898,#15696,#8841,.T.);
#19277=EDGE_CURVE('',#15693,#14899,#8842,.T.);
#19278=EDGE_CURVE('',#15697,#15698,#8843,.T.);
#19279=EDGE_CURVE('',#15699,#15697,#8844,.T.);
#19280=EDGE_CURVE('',#15698,#15699,#8845,.T.);
#19281=EDGE_CURVE('',#14896,#15699,#8846,.T.);
#19282=EDGE_CURVE('',#15697,#14897,#8847,.T.);
#19283=EDGE_CURVE('',#15692,#15698,#8848,.T.);
#19284=EDGE_CURVE('',#15699,#15695,#8849,.T.);
#19285=EDGE_CURVE('',#15698,#15694,#8850,.T.);
#19286=EDGE_CURVE('',#15696,#15697,#8851,.T.);
#19287=EDGE_CURVE('',#15695,#14895,#8852,.T.);
#19288=EDGE_CURVE('',#15700,#15701,#8853,.T.);
#19289=EDGE_CURVE('',#15702,#15700,#8854,.T.);
#19290=EDGE_CURVE('',#15701,#15702,#8855,.T.);
#19291=EDGE_CURVE('',#15703,#15704,#8856,.T.);
#19292=EDGE_CURVE('',#15705,#15703,#8857,.T.);
#19293=EDGE_CURVE('',#15704,#15705,#8858,.T.);
#19294=EDGE_CURVE('',#15706,#15707,#8859,.T.);
#19295=EDGE_CURVE('',#15708,#15706,#8860,.T.);
#19296=EDGE_CURVE('',#15707,#15708,#8861,.T.);
#19297=EDGE_CURVE('',#14906,#15708,#8862,.T.);
#19298=EDGE_CURVE('',#15706,#14907,#8863,.T.);
#19299=EDGE_CURVE('',#15709,#15710,#8864,.T.);
#19300=EDGE_CURVE('',#15711,#15709,#8865,.T.);
#19301=EDGE_CURVE('',#15710,#15711,#8866,.T.);
#19302=EDGE_CURVE('',#14904,#15711,#8867,.T.);
#19303=EDGE_CURVE('',#15709,#14905,#8868,.T.);
#19304=EDGE_CURVE('',#15703,#15710,#8869,.T.);
#19305=EDGE_CURVE('',#15711,#15705,#8870,.T.);
#19306=EDGE_CURVE('',#15710,#15707,#8871,.T.);
#19307=EDGE_CURVE('',#15708,#15709,#8872,.T.);
#19308=EDGE_CURVE('',#15700,#15706,#8873,.T.);
#19309=EDGE_CURVE('',#15707,#15702,#8874,.T.);
#19310=EDGE_CURVE('',#14910,#15704,#8875,.T.);
#19311=EDGE_CURVE('',#15705,#14903,#8876,.T.);
#19312=EDGE_CURVE('',#15704,#15701,#8877,.T.);
#19313=EDGE_CURVE('',#15702,#15703,#8878,.T.);
#19314=EDGE_CURVE('',#14908,#15700,#8879,.T.);
#19315=EDGE_CURVE('',#15701,#14909,#8880,.T.);
#19316=EDGE_CURVE('',#15712,#15713,#8881,.T.);
#19317=EDGE_CURVE('',#15714,#15712,#8882,.T.);
#19318=EDGE_CURVE('',#15713,#15714,#8883,.T.);
#19319=EDGE_CURVE('',#15715,#15716,#8884,.T.);
#19320=EDGE_CURVE('',#15716,#15714,#8885,.T.);
#19321=EDGE_CURVE('',#15712,#15717,#8886,.T.);
#19322=EDGE_CURVE('',#15717,#15715,#8887,.T.);
#19323=EDGE_CURVE('',#14918,#15713,#8888,.T.);
#19324=EDGE_CURVE('',#15714,#14911,#8889,.T.);
#19325=EDGE_CURVE('',#15718,#15719,#8890,.T.);
#19326=EDGE_CURVE('',#15720,#15718,#8891,.T.);
#19327=EDGE_CURVE('',#15719,#15720,#8892,.T.);
#19328=EDGE_CURVE('',#15721,#15722,#8893,.T.);
#19329=EDGE_CURVE('',#15722,#15720,#8894,.T.);
#19330=EDGE_CURVE('',#15718,#15723,#8895,.T.);
#19331=EDGE_CURVE('',#15723,#15721,#8896,.T.);
#19332=EDGE_CURVE('',#15713,#15719,#8897,.T.);
#19333=EDGE_CURVE('',#15720,#15712,#8898,.T.);
#19334=EDGE_CURVE('',#14916,#15718,#8899,.T.);
#19335=EDGE_CURVE('',#15719,#14917,#8900,.T.);
#19336=EDGE_CURVE('',#15715,#15724,#8901,.T.);
#19337=EDGE_CURVE('',#15724,#14913,#8902,.T.);
#19338=EDGE_CURVE('',#14912,#15716,#8903,.T.);
#19339=EDGE_CURVE('',#15717,#15722,#8904,.T.);
#19340=EDGE_CURVE('',#15725,#15721,#8905,.T.);
#19341=EDGE_CURVE('',#15725,#15724,#8906,.T.);
#19342=EDGE_CURVE('',#15723,#14915,#8907,.T.);
#19343=EDGE_CURVE('',#14914,#15725,#8908,.T.);
#19344=EDGE_CURVE('',#15726,#15727,#8909,.T.);
#19345=EDGE_CURVE('',#15728,#15726,#8910,.T.);
#19346=EDGE_CURVE('',#15727,#15728,#8911,.T.);
#19347=EDGE_CURVE('',#15729,#15730,#8912,.T.);
#19348=EDGE_CURVE('',#15731,#15729,#8913,.T.);
#19349=EDGE_CURVE('',#15730,#15731,#8914,.T.);
#19350=EDGE_CURVE('',#15732,#15733,#8915,.T.);
#19351=EDGE_CURVE('',#15734,#15732,#8916,.T.);
#19352=EDGE_CURVE('',#15733,#15734,#8917,.T.);
#19353=EDGE_CURVE('',#14922,#15734,#8918,.T.);
#19354=EDGE_CURVE('',#15732,#14923,#8919,.T.);
#19355=EDGE_CURVE('',#15735,#15736,#8920,.T.);
#19356=EDGE_CURVE('',#15737,#15735,#8921,.T.);
#19357=EDGE_CURVE('',#15736,#15737,#8922,.T.);
#19358=EDGE_CURVE('',#14920,#15737,#8923,.T.);
#19359=EDGE_CURVE('',#15735,#14921,#8924,.T.);
#19360=EDGE_CURVE('',#15729,#15736,#8925,.T.);
#19361=EDGE_CURVE('',#15737,#15731,#8926,.T.);
#19362=EDGE_CURVE('',#15736,#15733,#8927,.T.);
#19363=EDGE_CURVE('',#15734,#15735,#8928,.T.);
#19364=EDGE_CURVE('',#15726,#15732,#8929,.T.);
#19365=EDGE_CURVE('',#15733,#15728,#8930,.T.);
#19366=EDGE_CURVE('',#14926,#15730,#8931,.T.);
#19367=EDGE_CURVE('',#15731,#14919,#8932,.T.);
#19368=EDGE_CURVE('',#15730,#15727,#8933,.T.);
#19369=EDGE_CURVE('',#15728,#15729,#8934,.T.);
#19370=EDGE_CURVE('',#14924,#15726,#8935,.T.);
#19371=EDGE_CURVE('',#15727,#14925,#8936,.T.);
#19372=EDGE_CURVE('',#15738,#15739,#8937,.T.);
#19373=EDGE_CURVE('',#15740,#15738,#8938,.T.);
#19374=EDGE_CURVE('',#15739,#15740,#8939,.T.);
#19375=EDGE_CURVE('',#15741,#15742,#8940,.T.);
#19376=EDGE_CURVE('',#15743,#15741,#8941,.T.);
#19377=EDGE_CURVE('',#15742,#15743,#8942,.T.);
#19378=EDGE_CURVE('',#15744,#15745,#8943,.T.);
#19379=EDGE_CURVE('',#15746,#15744,#8944,.T.);
#19380=EDGE_CURVE('',#15745,#15746,#8945,.T.);
#19381=EDGE_CURVE('',#14930,#15746,#8946,.T.);
#19382=EDGE_CURVE('',#15744,#14931,#8947,.T.);
#19383=EDGE_CURVE('',#15747,#15748,#8948,.T.);
#19384=EDGE_CURVE('',#15749,#15747,#8949,.T.);
#19385=EDGE_CURVE('',#15748,#15749,#8950,.T.);
#19386=EDGE_CURVE('',#14928,#15749,#8951,.T.);
#19387=EDGE_CURVE('',#15747,#14929,#8952,.T.);
#19388=EDGE_CURVE('',#15741,#15748,#8953,.T.);
#19389=EDGE_CURVE('',#15749,#15743,#8954,.T.);
#19390=EDGE_CURVE('',#15748,#15745,#8955,.T.);
#19391=EDGE_CURVE('',#15746,#15747,#8956,.T.);
#19392=EDGE_CURVE('',#15738,#15744,#8957,.T.);
#19393=EDGE_CURVE('',#15745,#15740,#8958,.T.);
#19394=EDGE_CURVE('',#14934,#15742,#8959,.T.);
#19395=EDGE_CURVE('',#15743,#14927,#8960,.T.);
#19396=EDGE_CURVE('',#15742,#15739,#8961,.T.);
#19397=EDGE_CURVE('',#15740,#15741,#8962,.T.);
#19398=EDGE_CURVE('',#14932,#15738,#8963,.T.);
#19399=EDGE_CURVE('',#15739,#14933,#8964,.T.);
#19400=EDGE_CURVE('',#15750,#15751,#8965,.T.);
#19401=EDGE_CURVE('',#15751,#14941,#8966,.T.);
#19402=EDGE_CURVE('',#14940,#15752,#8967,.T.);
#19403=EDGE_CURVE('',#15752,#15750,#8968,.T.);
#19404=EDGE_CURVE('',#15753,#15751,#8969,.T.);
#19405=EDGE_CURVE('',#14942,#15753,#8970,.T.);
#19406=EDGE_CURVE('',#15754,#15750,#8971,.T.);
#19407=EDGE_CURVE('',#15754,#15755,#8972,.T.);
#19408=EDGE_CURVE('',#15755,#15753,#8973,.T.);
#19409=EDGE_CURVE('',#15752,#15756,#8974,.T.);
#19410=EDGE_CURVE('',#15756,#15757,#8975,.T.);
#19411=EDGE_CURVE('',#15757,#15754,#8976,.T.);
#19412=EDGE_CURVE('',#15758,#15755,#8977,.T.);
#19413=EDGE_CURVE('',#15753,#15758,#8978,.T.);
#19414=EDGE_CURVE('',#15759,#15756,#8979,.T.);
#19415=EDGE_CURVE('',#15757,#15759,#8980,.T.);
#19416=EDGE_CURVE('',#14938,#15759,#8981,.T.);
#19417=EDGE_CURVE('',#15756,#14939,#8982,.T.);
#19418=EDGE_CURVE('',#15760,#15761,#8983,.T.);
#19419=EDGE_CURVE('',#15762,#15760,#8984,.T.);
#19420=EDGE_CURVE('',#15761,#15762,#8985,.T.);
#19421=EDGE_CURVE('',#14936,#15762,#8986,.T.);
#19422=EDGE_CURVE('',#15760,#14937,#8987,.T.);
#19423=EDGE_CURVE('',#15755,#15761,#8988,.T.);
#19424=EDGE_CURVE('',#15762,#15758,#8989,.T.);
#19425=EDGE_CURVE('',#15761,#15757,#8990,.T.);
#19426=EDGE_CURVE('',#15759,#15760,#8991,.T.);
#19427=EDGE_CURVE('',#15758,#14935,#8992,.T.);
#19428=EDGE_CURVE('',#15763,#15764,#8993,.T.);
#19429=EDGE_CURVE('',#15765,#15763,#8994,.T.);
#19430=EDGE_CURVE('',#15764,#15765,#8995,.T.);
#19431=EDGE_CURVE('',#15766,#15767,#8996,.T.);
#19432=EDGE_CURVE('',#15768,#15766,#8997,.T.);
#19433=EDGE_CURVE('',#15767,#15768,#8998,.T.);
#19434=EDGE_CURVE('',#15769,#15770,#8999,.T.);
#19435=EDGE_CURVE('',#15771,#15769,#9000,.T.);
#19436=EDGE_CURVE('',#15770,#15771,#9001,.T.);
#19437=EDGE_CURVE('',#14946,#15771,#9002,.T.);
#19438=EDGE_CURVE('',#15769,#14947,#9003,.T.);
#19439=EDGE_CURVE('',#15772,#15773,#9004,.T.);
#19440=EDGE_CURVE('',#15774,#15772,#9005,.T.);
#19441=EDGE_CURVE('',#15773,#15774,#9006,.T.);
#19442=EDGE_CURVE('',#14944,#15774,#9007,.T.);
#19443=EDGE_CURVE('',#15772,#14945,#9008,.T.);
#19444=EDGE_CURVE('',#15766,#15773,#9009,.T.);
#19445=EDGE_CURVE('',#15774,#15768,#9010,.T.);
#19446=EDGE_CURVE('',#15773,#15770,#9011,.T.);
#19447=EDGE_CURVE('',#15771,#15772,#9012,.T.);
#19448=EDGE_CURVE('',#15763,#15769,#9013,.T.);
#19449=EDGE_CURVE('',#15770,#15765,#9014,.T.);
#19450=EDGE_CURVE('',#14950,#15767,#9015,.T.);
#19451=EDGE_CURVE('',#15768,#14943,#9016,.T.);
#19452=EDGE_CURVE('',#15767,#15764,#9017,.T.);
#19453=EDGE_CURVE('',#15765,#15766,#9018,.T.);
#19454=EDGE_CURVE('',#14948,#15763,#9019,.T.);
#19455=EDGE_CURVE('',#15764,#14949,#9020,.T.);
#19456=EDGE_CURVE('',#15775,#15776,#9021,.T.);
#19457=EDGE_CURVE('',#15777,#15775,#9022,.T.);
#19458=EDGE_CURVE('',#15776,#15777,#9023,.T.);
#19459=EDGE_CURVE('',#15778,#15779,#9024,.T.);
#19460=EDGE_CURVE('',#15779,#15777,#9025,.T.);
#19461=EDGE_CURVE('',#15775,#15780,#9026,.T.);
#19462=EDGE_CURVE('',#15780,#15778,#9027,.T.);
#19463=EDGE_CURVE('',#14958,#15776,#9028,.T.);
#19464=EDGE_CURVE('',#15777,#14951,#9029,.T.);
#19465=EDGE_CURVE('',#15781,#15782,#9030,.T.);
#19466=EDGE_CURVE('',#15783,#15781,#9031,.T.);
#19467=EDGE_CURVE('',#15782,#15783,#9032,.T.);
#19468=EDGE_CURVE('',#15784,#15785,#9033,.T.);
#19469=EDGE_CURVE('',#15785,#15783,#9034,.T.);
#19470=EDGE_CURVE('',#15781,#15786,#9035,.T.);
#19471=EDGE_CURVE('',#15786,#15784,#9036,.T.);
#19472=EDGE_CURVE('',#15776,#15782,#9037,.T.);
#19473=EDGE_CURVE('',#15783,#15775,#9038,.T.);
#19474=EDGE_CURVE('',#14956,#15781,#9039,.T.);
#19475=EDGE_CURVE('',#15782,#14957,#9040,.T.);
#19476=EDGE_CURVE('',#15778,#15787,#9041,.T.);
#19477=EDGE_CURVE('',#15787,#14953,#9042,.T.);
#19478=EDGE_CURVE('',#14952,#15779,#9043,.T.);
#19479=EDGE_CURVE('',#15780,#15785,#9044,.T.);
#19480=EDGE_CURVE('',#15788,#15784,#9045,.T.);
#19481=EDGE_CURVE('',#15788,#15787,#9046,.T.);
#19482=EDGE_CURVE('',#15786,#14955,#9047,.T.);
#19483=EDGE_CURVE('',#14954,#15788,#9048,.T.);
#19484=EDGE_CURVE('',#15789,#15790,#9049,.T.);
#19485=EDGE_CURVE('',#15791,#15789,#9050,.T.);
#19486=EDGE_CURVE('',#15790,#15791,#9051,.T.);
#19487=EDGE_CURVE('',#15792,#15793,#9052,.T.);
#19488=EDGE_CURVE('',#15794,#15792,#9053,.T.);
#19489=EDGE_CURVE('',#15793,#15794,#9054,.T.);
#19490=EDGE_CURVE('',#15795,#15796,#9055,.T.);
#19491=EDGE_CURVE('',#15797,#15795,#9056,.T.);
#19492=EDGE_CURVE('',#15796,#15797,#9057,.T.);
#19493=EDGE_CURVE('',#14962,#15797,#9058,.T.);
#19494=EDGE_CURVE('',#15795,#14963,#9059,.T.);
#19495=EDGE_CURVE('',#15798,#15799,#9060,.T.);
#19496=EDGE_CURVE('',#15800,#15798,#9061,.T.);
#19497=EDGE_CURVE('',#15799,#15800,#9062,.T.);
#19498=EDGE_CURVE('',#14960,#15800,#9063,.T.);
#19499=EDGE_CURVE('',#15798,#14961,#9064,.T.);
#19500=EDGE_CURVE('',#15792,#15799,#9065,.T.);
#19501=EDGE_CURVE('',#15800,#15794,#9066,.T.);
#19502=EDGE_CURVE('',#15799,#15796,#9067,.T.);
#19503=EDGE_CURVE('',#15797,#15798,#9068,.T.);
#19504=EDGE_CURVE('',#15789,#15795,#9069,.T.);
#19505=EDGE_CURVE('',#15796,#15791,#9070,.T.);
#19506=EDGE_CURVE('',#14966,#15793,#9071,.T.);
#19507=EDGE_CURVE('',#15794,#14959,#9072,.T.);
#19508=EDGE_CURVE('',#15793,#15790,#9073,.T.);
#19509=EDGE_CURVE('',#15791,#15792,#9074,.T.);
#19510=EDGE_CURVE('',#14964,#15789,#9075,.T.);
#19511=EDGE_CURVE('',#15790,#14965,#9076,.T.);
#19512=EDGE_CURVE('',#15801,#15802,#9077,.T.);
#19513=EDGE_CURVE('',#15803,#15801,#9078,.T.);
#19514=EDGE_CURVE('',#15802,#15803,#9079,.T.);
#19515=EDGE_CURVE('',#15804,#15805,#9080,.T.);
#19516=EDGE_CURVE('',#15806,#15804,#9081,.T.);
#19517=EDGE_CURVE('',#15805,#15806,#9082,.T.);
#19518=EDGE_CURVE('',#15807,#15808,#9083,.T.);
#19519=EDGE_CURVE('',#15809,#15807,#9084,.T.);
#19520=EDGE_CURVE('',#15808,#15809,#9085,.T.);
#19521=EDGE_CURVE('',#14970,#15809,#9086,.T.);
#19522=EDGE_CURVE('',#15807,#14971,#9087,.T.);
#19523=EDGE_CURVE('',#15810,#15811,#9088,.T.);
#19524=EDGE_CURVE('',#15812,#15810,#9089,.T.);
#19525=EDGE_CURVE('',#15811,#15812,#9090,.T.);
#19526=EDGE_CURVE('',#14968,#15812,#9091,.T.);
#19527=EDGE_CURVE('',#15810,#14969,#9092,.T.);
#19528=EDGE_CURVE('',#15804,#15811,#9093,.T.);
#19529=EDGE_CURVE('',#15812,#15806,#9094,.T.);
#19530=EDGE_CURVE('',#15811,#15808,#9095,.T.);
#19531=EDGE_CURVE('',#15809,#15810,#9096,.T.);
#19532=EDGE_CURVE('',#15801,#15807,#9097,.T.);
#19533=EDGE_CURVE('',#15808,#15803,#9098,.T.);
#19534=EDGE_CURVE('',#14974,#15805,#9099,.T.);
#19535=EDGE_CURVE('',#15806,#14967,#9100,.T.);
#19536=EDGE_CURVE('',#15805,#15802,#9101,.T.);
#19537=EDGE_CURVE('',#15803,#15804,#9102,.T.);
#19538=EDGE_CURVE('',#14972,#15801,#9103,.T.);
#19539=EDGE_CURVE('',#15802,#14973,#9104,.T.);
#19540=EDGE_CURVE('',#15813,#15814,#9105,.T.);
#19541=EDGE_CURVE('',#15814,#14981,#9106,.T.);
#19542=EDGE_CURVE('',#14980,#15815,#9107,.T.);
#19543=EDGE_CURVE('',#15815,#15813,#9108,.T.);
#19544=EDGE_CURVE('',#15816,#15814,#9109,.T.);
#19545=EDGE_CURVE('',#14982,#15816,#9110,.T.);
#19546=EDGE_CURVE('',#15817,#15813,#9111,.T.);
#19547=EDGE_CURVE('',#15817,#15818,#9112,.T.);
#19548=EDGE_CURVE('',#15818,#15816,#9113,.T.);
#19549=EDGE_CURVE('',#15815,#15819,#9114,.T.);
#19550=EDGE_CURVE('',#15819,#15820,#9115,.T.);
#19551=EDGE_CURVE('',#15820,#15817,#9116,.T.);
#19552=EDGE_CURVE('',#15821,#15818,#9117,.T.);
#19553=EDGE_CURVE('',#15816,#15821,#9118,.T.);
#19554=EDGE_CURVE('',#15822,#15819,#9119,.T.);
#19555=EDGE_CURVE('',#15820,#15822,#9120,.T.);
#19556=EDGE_CURVE('',#14978,#15822,#9121,.T.);
#19557=EDGE_CURVE('',#15819,#14979,#9122,.T.);
#19558=EDGE_CURVE('',#15823,#15824,#9123,.T.);
#19559=EDGE_CURVE('',#15825,#15823,#9124,.T.);
#19560=EDGE_CURVE('',#15824,#15825,#9125,.T.);
#19561=EDGE_CURVE('',#14976,#15825,#9126,.T.);
#19562=EDGE_CURVE('',#15823,#14977,#9127,.T.);
#19563=EDGE_CURVE('',#15818,#15824,#9128,.T.);
#19564=EDGE_CURVE('',#15825,#15821,#9129,.T.);
#19565=EDGE_CURVE('',#15824,#15820,#9130,.T.);
#19566=EDGE_CURVE('',#15822,#15823,#9131,.T.);
#19567=EDGE_CURVE('',#15821,#14975,#9132,.T.);
#19568=EDGE_CURVE('',#15826,#15827,#9133,.T.);
#19569=EDGE_CURVE('',#15828,#15826,#9134,.T.);
#19570=EDGE_CURVE('',#15827,#15828,#9135,.T.);
#19571=EDGE_CURVE('',#15829,#15830,#9136,.T.);
#19572=EDGE_CURVE('',#15831,#15829,#9137,.T.);
#19573=EDGE_CURVE('',#15830,#15831,#9138,.T.);
#19574=EDGE_CURVE('',#15832,#15833,#9139,.T.);
#19575=EDGE_CURVE('',#15834,#15832,#9140,.T.);
#19576=EDGE_CURVE('',#15833,#15834,#9141,.T.);
#19577=EDGE_CURVE('',#14986,#15834,#9142,.T.);
#19578=EDGE_CURVE('',#15832,#14987,#9143,.T.);
#19579=EDGE_CURVE('',#15835,#15836,#9144,.T.);
#19580=EDGE_CURVE('',#15837,#15835,#9145,.T.);
#19581=EDGE_CURVE('',#15836,#15837,#9146,.T.);
#19582=EDGE_CURVE('',#14984,#15837,#9147,.T.);
#19583=EDGE_CURVE('',#15835,#14985,#9148,.T.);
#19584=EDGE_CURVE('',#15829,#15836,#9149,.T.);
#19585=EDGE_CURVE('',#15837,#15831,#9150,.T.);
#19586=EDGE_CURVE('',#15836,#15833,#9151,.T.);
#19587=EDGE_CURVE('',#15834,#15835,#9152,.T.);
#19588=EDGE_CURVE('',#15826,#15832,#9153,.T.);
#19589=EDGE_CURVE('',#15833,#15828,#9154,.T.);
#19590=EDGE_CURVE('',#14990,#15830,#9155,.T.);
#19591=EDGE_CURVE('',#15831,#14983,#9156,.T.);
#19592=EDGE_CURVE('',#15830,#15827,#9157,.T.);
#19593=EDGE_CURVE('',#15828,#15829,#9158,.T.);
#19594=EDGE_CURVE('',#14988,#15826,#9159,.T.);
#19595=EDGE_CURVE('',#15827,#14989,#9160,.T.);
#19596=EDGE_CURVE('',#15838,#15839,#9161,.T.);
#19597=EDGE_CURVE('',#15840,#15838,#9162,.T.);
#19598=EDGE_CURVE('',#15839,#15840,#9163,.T.);
#19599=EDGE_CURVE('',#15841,#15842,#9164,.T.);
#19600=EDGE_CURVE('',#15842,#15840,#9165,.T.);
#19601=EDGE_CURVE('',#15838,#15843,#9166,.T.);
#19602=EDGE_CURVE('',#15843,#15841,#9167,.T.);
#19603=EDGE_CURVE('',#14998,#15839,#9168,.T.);
#19604=EDGE_CURVE('',#15840,#14991,#9169,.T.);
#19605=EDGE_CURVE('',#15844,#15845,#9170,.T.);
#19606=EDGE_CURVE('',#15846,#15844,#9171,.T.);
#19607=EDGE_CURVE('',#15845,#15846,#9172,.T.);
#19608=EDGE_CURVE('',#15847,#15848,#9173,.T.);
#19609=EDGE_CURVE('',#15848,#15846,#9174,.T.);
#19610=EDGE_CURVE('',#15844,#15849,#9175,.T.);
#19611=EDGE_CURVE('',#15849,#15847,#9176,.T.);
#19612=EDGE_CURVE('',#15839,#15845,#9177,.T.);
#19613=EDGE_CURVE('',#15846,#15838,#9178,.T.);
#19614=EDGE_CURVE('',#14996,#15844,#9179,.T.);
#19615=EDGE_CURVE('',#15845,#14997,#9180,.T.);
#19616=EDGE_CURVE('',#15841,#15850,#9181,.T.);
#19617=EDGE_CURVE('',#15850,#14993,#9182,.T.);
#19618=EDGE_CURVE('',#14992,#15842,#9183,.T.);
#19619=EDGE_CURVE('',#15843,#15848,#9184,.T.);
#19620=EDGE_CURVE('',#15851,#15847,#9185,.T.);
#19621=EDGE_CURVE('',#15851,#15850,#9186,.T.);
#19622=EDGE_CURVE('',#15849,#14995,#9187,.T.);
#19623=EDGE_CURVE('',#14994,#15851,#9188,.T.);
#19624=EDGE_CURVE('',#15852,#15853,#9189,.T.);
#19625=EDGE_CURVE('',#15854,#15852,#9190,.T.);
#19626=EDGE_CURVE('',#15853,#15854,#9191,.T.);
#19627=EDGE_CURVE('',#15855,#15856,#9192,.T.);
#19628=EDGE_CURVE('',#15857,#15855,#9193,.T.);
#19629=EDGE_CURVE('',#15856,#15857,#9194,.T.);
#19630=EDGE_CURVE('',#15858,#15859,#9195,.T.);
#19631=EDGE_CURVE('',#15860,#15858,#9196,.T.);
#19632=EDGE_CURVE('',#15859,#15860,#9197,.T.);
#19633=EDGE_CURVE('',#15002,#15860,#9198,.T.);
#19634=EDGE_CURVE('',#15858,#15003,#9199,.T.);
#19635=EDGE_CURVE('',#15861,#15862,#9200,.T.);
#19636=EDGE_CURVE('',#15863,#15861,#9201,.T.);
#19637=EDGE_CURVE('',#15862,#15863,#9202,.T.);
#19638=EDGE_CURVE('',#15000,#15863,#9203,.T.);
#19639=EDGE_CURVE('',#15861,#15001,#9204,.T.);
#19640=EDGE_CURVE('',#15855,#15862,#9205,.T.);
#19641=EDGE_CURVE('',#15863,#15857,#9206,.T.);
#19642=EDGE_CURVE('',#15862,#15859,#9207,.T.);
#19643=EDGE_CURVE('',#15860,#15861,#9208,.T.);
#19644=EDGE_CURVE('',#15852,#15858,#9209,.T.);
#19645=EDGE_CURVE('',#15859,#15854,#9210,.T.);
#19646=EDGE_CURVE('',#15006,#15856,#9211,.T.);
#19647=EDGE_CURVE('',#15857,#14999,#9212,.T.);
#19648=EDGE_CURVE('',#15856,#15853,#9213,.T.);
#19649=EDGE_CURVE('',#15854,#15855,#9214,.T.);
#19650=EDGE_CURVE('',#15004,#15852,#9215,.T.);
#19651=EDGE_CURVE('',#15853,#15005,#9216,.T.);
#19652=EDGE_CURVE('',#15864,#15865,#9217,.T.);
#19653=EDGE_CURVE('',#15866,#15864,#9218,.T.);
#19654=EDGE_CURVE('',#15865,#15866,#9219,.T.);
#19655=EDGE_CURVE('',#15867,#15868,#9220,.T.);
#19656=EDGE_CURVE('',#15869,#15867,#9221,.T.);
#19657=EDGE_CURVE('',#15868,#15869,#9222,.T.);
#19658=EDGE_CURVE('',#15870,#15871,#9223,.T.);
#19659=EDGE_CURVE('',#15872,#15870,#9224,.T.);
#19660=EDGE_CURVE('',#15871,#15872,#9225,.T.);
#19661=EDGE_CURVE('',#15010,#15872,#9226,.T.);
#19662=EDGE_CURVE('',#15870,#15011,#9227,.T.);
#19663=EDGE_CURVE('',#15873,#15874,#9228,.T.);
#19664=EDGE_CURVE('',#15875,#15873,#9229,.T.);
#19665=EDGE_CURVE('',#15874,#15875,#9230,.T.);
#19666=EDGE_CURVE('',#15008,#15875,#9231,.T.);
#19667=EDGE_CURVE('',#15873,#15009,#9232,.T.);
#19668=EDGE_CURVE('',#15867,#15874,#9233,.T.);
#19669=EDGE_CURVE('',#15875,#15869,#9234,.T.);
#19670=EDGE_CURVE('',#15874,#15871,#9235,.T.);
#19671=EDGE_CURVE('',#15872,#15873,#9236,.T.);
#19672=EDGE_CURVE('',#15864,#15870,#9237,.T.);
#19673=EDGE_CURVE('',#15871,#15866,#9238,.T.);
#19674=EDGE_CURVE('',#15014,#15868,#9239,.T.);
#19675=EDGE_CURVE('',#15869,#15007,#9240,.T.);
#19676=EDGE_CURVE('',#15868,#15865,#9241,.T.);
#19677=EDGE_CURVE('',#15866,#15867,#9242,.T.);
#19678=EDGE_CURVE('',#15012,#15864,#9243,.T.);
#19679=EDGE_CURVE('',#15865,#15013,#9244,.T.);
#19680=EDGE_CURVE('',#15876,#15877,#9245,.T.);
#19681=EDGE_CURVE('',#15877,#15021,#9246,.T.);
#19682=EDGE_CURVE('',#15020,#15878,#9247,.T.);
#19683=EDGE_CURVE('',#15878,#15876,#9248,.T.);
#19684=EDGE_CURVE('',#15879,#15877,#9249,.T.);
#19685=EDGE_CURVE('',#15022,#15879,#9250,.T.);
#19686=EDGE_CURVE('',#15880,#15876,#9251,.T.);
#19687=EDGE_CURVE('',#15880,#15881,#9252,.T.);
#19688=EDGE_CURVE('',#15881,#15879,#9253,.T.);
#19689=EDGE_CURVE('',#15878,#15882,#9254,.T.);
#19690=EDGE_CURVE('',#15882,#15883,#9255,.T.);
#19691=EDGE_CURVE('',#15883,#15880,#9256,.T.);
#19692=EDGE_CURVE('',#15884,#15881,#9257,.T.);
#19693=EDGE_CURVE('',#15879,#15884,#9258,.T.);
#19694=EDGE_CURVE('',#15885,#15882,#9259,.T.);
#19695=EDGE_CURVE('',#15883,#15885,#9260,.T.);
#19696=EDGE_CURVE('',#15018,#15885,#9261,.T.);
#19697=EDGE_CURVE('',#15882,#15019,#9262,.T.);
#19698=EDGE_CURVE('',#15886,#15887,#9263,.T.);
#19699=EDGE_CURVE('',#15888,#15886,#9264,.T.);
#19700=EDGE_CURVE('',#15887,#15888,#9265,.T.);
#19701=EDGE_CURVE('',#15016,#15888,#9266,.T.);
#19702=EDGE_CURVE('',#15886,#15017,#9267,.T.);
#19703=EDGE_CURVE('',#15881,#15887,#9268,.T.);
#19704=EDGE_CURVE('',#15888,#15884,#9269,.T.);
#19705=EDGE_CURVE('',#15887,#15883,#9270,.T.);
#19706=EDGE_CURVE('',#15885,#15886,#9271,.T.);
#19707=EDGE_CURVE('',#15884,#15015,#9272,.T.);
#19708=EDGE_CURVE('',#15889,#15890,#9273,.T.);
#19709=EDGE_CURVE('',#15891,#15889,#9274,.T.);
#19710=EDGE_CURVE('',#15890,#15891,#9275,.T.);
#19711=EDGE_CURVE('',#15892,#15893,#9276,.T.);
#19712=EDGE_CURVE('',#15894,#15892,#9277,.T.);
#19713=EDGE_CURVE('',#15893,#15894,#9278,.T.);
#19714=EDGE_CURVE('',#15895,#15896,#9279,.T.);
#19715=EDGE_CURVE('',#15897,#15895,#9280,.T.);
#19716=EDGE_CURVE('',#15896,#15897,#9281,.T.);
#19717=EDGE_CURVE('',#15026,#15897,#9282,.T.);
#19718=EDGE_CURVE('',#15895,#15027,#9283,.T.);
#19719=EDGE_CURVE('',#15898,#15899,#9284,.T.);
#19720=EDGE_CURVE('',#15900,#15898,#9285,.T.);
#19721=EDGE_CURVE('',#15899,#15900,#9286,.T.);
#19722=EDGE_CURVE('',#15024,#15900,#9287,.T.);
#19723=EDGE_CURVE('',#15898,#15025,#9288,.T.);
#19724=EDGE_CURVE('',#15892,#15899,#9289,.T.);
#19725=EDGE_CURVE('',#15900,#15894,#9290,.T.);
#19726=EDGE_CURVE('',#15899,#15896,#9291,.T.);
#19727=EDGE_CURVE('',#15897,#15898,#9292,.T.);
#19728=EDGE_CURVE('',#15889,#15895,#9293,.T.);
#19729=EDGE_CURVE('',#15896,#15891,#9294,.T.);
#19730=EDGE_CURVE('',#15030,#15893,#9295,.T.);
#19731=EDGE_CURVE('',#15894,#15023,#9296,.T.);
#19732=EDGE_CURVE('',#15893,#15890,#9297,.T.);
#19733=EDGE_CURVE('',#15891,#15892,#9298,.T.);
#19734=EDGE_CURVE('',#15028,#15889,#9299,.T.);
#19735=EDGE_CURVE('',#15890,#15029,#9300,.T.);
#19736=EDGE_CURVE('',#15901,#15902,#9301,.T.);
#19737=EDGE_CURVE('',#15903,#15901,#9302,.T.);
#19738=EDGE_CURVE('',#15902,#15903,#9303,.T.);
#19739=EDGE_CURVE('',#15904,#15905,#9304,.T.);
#19740=EDGE_CURVE('',#15905,#15903,#9305,.T.);
#19741=EDGE_CURVE('',#15901,#15906,#9306,.T.);
#19742=EDGE_CURVE('',#15906,#15904,#9307,.T.);
#19743=EDGE_CURVE('',#15038,#15902,#9308,.T.);
#19744=EDGE_CURVE('',#15903,#15031,#9309,.T.);
#19745=EDGE_CURVE('',#15907,#15908,#9310,.T.);
#19746=EDGE_CURVE('',#15909,#15907,#9311,.T.);
#19747=EDGE_CURVE('',#15908,#15909,#9312,.T.);
#19748=EDGE_CURVE('',#15910,#15911,#9313,.T.);
#19749=EDGE_CURVE('',#15911,#15909,#9314,.T.);
#19750=EDGE_CURVE('',#15907,#15912,#9315,.T.);
#19751=EDGE_CURVE('',#15912,#15910,#9316,.T.);
#19752=EDGE_CURVE('',#15902,#15908,#9317,.T.);
#19753=EDGE_CURVE('',#15909,#15901,#9318,.T.);
#19754=EDGE_CURVE('',#15036,#15907,#9319,.T.);
#19755=EDGE_CURVE('',#15908,#15037,#9320,.T.);
#19756=EDGE_CURVE('',#15904,#15913,#9321,.T.);
#19757=EDGE_CURVE('',#15913,#15033,#9322,.T.);
#19758=EDGE_CURVE('',#15032,#15905,#9323,.T.);
#19759=EDGE_CURVE('',#15906,#15911,#9324,.T.);
#19760=EDGE_CURVE('',#15914,#15910,#9325,.T.);
#19761=EDGE_CURVE('',#15914,#15913,#9326,.T.);
#19762=EDGE_CURVE('',#15912,#15035,#9327,.T.);
#19763=EDGE_CURVE('',#15034,#15914,#9328,.T.);
#19764=EDGE_CURVE('',#15915,#15916,#9329,.T.);
#19765=EDGE_CURVE('',#15917,#15915,#9330,.T.);
#19766=EDGE_CURVE('',#15916,#15917,#9331,.T.);
#19767=EDGE_CURVE('',#15918,#15919,#9332,.T.);
#19768=EDGE_CURVE('',#15920,#15918,#9333,.T.);
#19769=EDGE_CURVE('',#15919,#15920,#9334,.T.);
#19770=EDGE_CURVE('',#15921,#15922,#9335,.T.);
#19771=EDGE_CURVE('',#15923,#15921,#9336,.T.);
#19772=EDGE_CURVE('',#15922,#15923,#9337,.T.);
#19773=EDGE_CURVE('',#15042,#15923,#9338,.T.);
#19774=EDGE_CURVE('',#15921,#15043,#9339,.T.);
#19775=EDGE_CURVE('',#15924,#15925,#9340,.T.);
#19776=EDGE_CURVE('',#15926,#15924,#9341,.T.);
#19777=EDGE_CURVE('',#15925,#15926,#9342,.T.);
#19778=EDGE_CURVE('',#15040,#15926,#9343,.T.);
#19779=EDGE_CURVE('',#15924,#15041,#9344,.T.);
#19780=EDGE_CURVE('',#15918,#15925,#9345,.T.);
#19781=EDGE_CURVE('',#15926,#15920,#9346,.T.);
#19782=EDGE_CURVE('',#15925,#15922,#9347,.T.);
#19783=EDGE_CURVE('',#15923,#15924,#9348,.T.);
#19784=EDGE_CURVE('',#15915,#15921,#9349,.T.);
#19785=EDGE_CURVE('',#15922,#15917,#9350,.T.);
#19786=EDGE_CURVE('',#15046,#15919,#9351,.T.);
#19787=EDGE_CURVE('',#15920,#15039,#9352,.T.);
#19788=EDGE_CURVE('',#15919,#15916,#9353,.T.);
#19789=EDGE_CURVE('',#15917,#15918,#9354,.T.);
#19790=EDGE_CURVE('',#15044,#15915,#9355,.T.);
#19791=EDGE_CURVE('',#15916,#15045,#9356,.T.);
#19792=EDGE_CURVE('',#15927,#15928,#9357,.T.);
#19793=EDGE_CURVE('',#15929,#15927,#9358,.T.);
#19794=EDGE_CURVE('',#15928,#15929,#9359,.T.);
#19795=EDGE_CURVE('',#15930,#15931,#9360,.T.);
#19796=EDGE_CURVE('',#15932,#15930,#9361,.T.);
#19797=EDGE_CURVE('',#15931,#15932,#9362,.T.);
#19798=EDGE_CURVE('',#15933,#15934,#9363,.T.);
#19799=EDGE_CURVE('',#15935,#15933,#9364,.T.);
#19800=EDGE_CURVE('',#15934,#15935,#9365,.T.);
#19801=EDGE_CURVE('',#15050,#15935,#9366,.T.);
#19802=EDGE_CURVE('',#15933,#15051,#9367,.T.);
#19803=EDGE_CURVE('',#15936,#15937,#9368,.T.);
#19804=EDGE_CURVE('',#15938,#15936,#9369,.T.);
#19805=EDGE_CURVE('',#15937,#15938,#9370,.T.);
#19806=EDGE_CURVE('',#15048,#15938,#9371,.T.);
#19807=EDGE_CURVE('',#15936,#15049,#9372,.T.);
#19808=EDGE_CURVE('',#15930,#15937,#9373,.T.);
#19809=EDGE_CURVE('',#15938,#15932,#9374,.T.);
#19810=EDGE_CURVE('',#15937,#15934,#9375,.T.);
#19811=EDGE_CURVE('',#15935,#15936,#9376,.T.);
#19812=EDGE_CURVE('',#15927,#15933,#9377,.T.);
#19813=EDGE_CURVE('',#15934,#15929,#9378,.T.);
#19814=EDGE_CURVE('',#15054,#15931,#9379,.T.);
#19815=EDGE_CURVE('',#15932,#15047,#9380,.T.);
#19816=EDGE_CURVE('',#15931,#15928,#9381,.T.);
#19817=EDGE_CURVE('',#15929,#15930,#9382,.T.);
#19818=EDGE_CURVE('',#15052,#15927,#9383,.T.);
#19819=EDGE_CURVE('',#15928,#15053,#9384,.T.);
#19820=EDGE_CURVE('',#15939,#15940,#9385,.T.);
#19821=EDGE_CURVE('',#15940,#15061,#9386,.T.);
#19822=EDGE_CURVE('',#15060,#15941,#9387,.T.);
#19823=EDGE_CURVE('',#15941,#15939,#9388,.T.);
#19824=EDGE_CURVE('',#15942,#15940,#9389,.T.);
#19825=EDGE_CURVE('',#15062,#15942,#9390,.T.);
#19826=EDGE_CURVE('',#15943,#15939,#9391,.T.);
#19827=EDGE_CURVE('',#15943,#15944,#9392,.T.);
#19828=EDGE_CURVE('',#15944,#15942,#9393,.T.);
#19829=EDGE_CURVE('',#15941,#15945,#9394,.T.);
#19830=EDGE_CURVE('',#15945,#15946,#9395,.T.);
#19831=EDGE_CURVE('',#15946,#15943,#9396,.T.);
#19832=EDGE_CURVE('',#15947,#15944,#9397,.T.);
#19833=EDGE_CURVE('',#15942,#15947,#9398,.T.);
#19834=EDGE_CURVE('',#15948,#15945,#9399,.T.);
#19835=EDGE_CURVE('',#15946,#15948,#9400,.T.);
#19836=EDGE_CURVE('',#15058,#15948,#9401,.T.);
#19837=EDGE_CURVE('',#15945,#15059,#9402,.T.);
#19838=EDGE_CURVE('',#15949,#15950,#9403,.T.);
#19839=EDGE_CURVE('',#15951,#15949,#9404,.T.);
#19840=EDGE_CURVE('',#15950,#15951,#9405,.T.);
#19841=EDGE_CURVE('',#15056,#15951,#9406,.T.);
#19842=EDGE_CURVE('',#15949,#15057,#9407,.T.);
#19843=EDGE_CURVE('',#15944,#15950,#9408,.T.);
#19844=EDGE_CURVE('',#15951,#15947,#9409,.T.);
#19845=EDGE_CURVE('',#15950,#15946,#9410,.T.);
#19846=EDGE_CURVE('',#15948,#15949,#9411,.T.);
#19847=EDGE_CURVE('',#15947,#15055,#9412,.T.);
#19848=EDGE_CURVE('',#15952,#15953,#9413,.T.);
#19849=EDGE_CURVE('',#15954,#15952,#9414,.T.);
#19850=EDGE_CURVE('',#15953,#15954,#9415,.T.);
#19851=EDGE_CURVE('',#15955,#15956,#9416,.T.);
#19852=EDGE_CURVE('',#15957,#15955,#9417,.T.);
#19853=EDGE_CURVE('',#15956,#15957,#9418,.T.);
#19854=EDGE_CURVE('',#15958,#15959,#9419,.T.);
#19855=EDGE_CURVE('',#15960,#15958,#9420,.T.);
#19856=EDGE_CURVE('',#15959,#15960,#9421,.T.);
#19857=EDGE_CURVE('',#15066,#15960,#9422,.T.);
#19858=EDGE_CURVE('',#15958,#15067,#9423,.T.);
#19859=EDGE_CURVE('',#15961,#15962,#9424,.T.);
#19860=EDGE_CURVE('',#15963,#15961,#9425,.T.);
#19861=EDGE_CURVE('',#15962,#15963,#9426,.T.);
#19862=EDGE_CURVE('',#15064,#15963,#9427,.T.);
#19863=EDGE_CURVE('',#15961,#15065,#9428,.T.);
#19864=EDGE_CURVE('',#15955,#15962,#9429,.T.);
#19865=EDGE_CURVE('',#15963,#15957,#9430,.T.);
#19866=EDGE_CURVE('',#15962,#15959,#9431,.T.);
#19867=EDGE_CURVE('',#15960,#15961,#9432,.T.);
#19868=EDGE_CURVE('',#15952,#15958,#9433,.T.);
#19869=EDGE_CURVE('',#15959,#15954,#9434,.T.);
#19870=EDGE_CURVE('',#15070,#15956,#9435,.T.);
#19871=EDGE_CURVE('',#15957,#15063,#9436,.T.);
#19872=EDGE_CURVE('',#15956,#15953,#9437,.T.);
#19873=EDGE_CURVE('',#15954,#15955,#9438,.T.);
#19874=EDGE_CURVE('',#15068,#15952,#9439,.T.);
#19875=EDGE_CURVE('',#15953,#15069,#9440,.T.);
#19876=EDGE_CURVE('',#15964,#15965,#9441,.T.);
#19877=EDGE_CURVE('',#15966,#15964,#9442,.T.);
#19878=EDGE_CURVE('',#15965,#15966,#9443,.T.);
#19879=EDGE_CURVE('',#15967,#15968,#9444,.T.);
#19880=EDGE_CURVE('',#15968,#15966,#9445,.T.);
#19881=EDGE_CURVE('',#15964,#15969,#9446,.T.);
#19882=EDGE_CURVE('',#15969,#15967,#9447,.T.);
#19883=EDGE_CURVE('',#15078,#15965,#9448,.T.);
#19884=EDGE_CURVE('',#15966,#15071,#9449,.T.);
#19885=EDGE_CURVE('',#15970,#15971,#9450,.T.);
#19886=EDGE_CURVE('',#15972,#15970,#9451,.T.);
#19887=EDGE_CURVE('',#15971,#15972,#9452,.T.);
#19888=EDGE_CURVE('',#15973,#15974,#9453,.T.);
#19889=EDGE_CURVE('',#15974,#15972,#9454,.T.);
#19890=EDGE_CURVE('',#15970,#15975,#9455,.T.);
#19891=EDGE_CURVE('',#15975,#15973,#9456,.T.);
#19892=EDGE_CURVE('',#15965,#15971,#9457,.T.);
#19893=EDGE_CURVE('',#15972,#15964,#9458,.T.);
#19894=EDGE_CURVE('',#15076,#15970,#9459,.T.);
#19895=EDGE_CURVE('',#15971,#15077,#9460,.T.);
#19896=EDGE_CURVE('',#15967,#15976,#9461,.T.);
#19897=EDGE_CURVE('',#15976,#15073,#9462,.T.);
#19898=EDGE_CURVE('',#15072,#15968,#9463,.T.);
#19899=EDGE_CURVE('',#15969,#15974,#9464,.T.);
#19900=EDGE_CURVE('',#15977,#15973,#9465,.T.);
#19901=EDGE_CURVE('',#15977,#15976,#9466,.T.);
#19902=EDGE_CURVE('',#15975,#15075,#9467,.T.);
#19903=EDGE_CURVE('',#15074,#15977,#9468,.T.);
#19904=EDGE_CURVE('',#15978,#15979,#9469,.T.);
#19905=EDGE_CURVE('',#15980,#15978,#9470,.T.);
#19906=EDGE_CURVE('',#15979,#15980,#9471,.T.);
#19907=EDGE_CURVE('',#15981,#15982,#9472,.T.);
#19908=EDGE_CURVE('',#15983,#15981,#9473,.T.);
#19909=EDGE_CURVE('',#15982,#15983,#9474,.T.);
#19910=EDGE_CURVE('',#15984,#15985,#9475,.T.);
#19911=EDGE_CURVE('',#15986,#15984,#9476,.T.);
#19912=EDGE_CURVE('',#15985,#15986,#9477,.T.);
#19913=EDGE_CURVE('',#15082,#15986,#9478,.T.);
#19914=EDGE_CURVE('',#15984,#15083,#9479,.T.);
#19915=EDGE_CURVE('',#15987,#15988,#9480,.T.);
#19916=EDGE_CURVE('',#15989,#15987,#9481,.T.);
#19917=EDGE_CURVE('',#15988,#15989,#9482,.T.);
#19918=EDGE_CURVE('',#15080,#15989,#9483,.T.);
#19919=EDGE_CURVE('',#15987,#15081,#9484,.T.);
#19920=EDGE_CURVE('',#15981,#15988,#9485,.T.);
#19921=EDGE_CURVE('',#15989,#15983,#9486,.T.);
#19922=EDGE_CURVE('',#15988,#15985,#9487,.T.);
#19923=EDGE_CURVE('',#15986,#15987,#9488,.T.);
#19924=EDGE_CURVE('',#15978,#15984,#9489,.T.);
#19925=EDGE_CURVE('',#15985,#15980,#9490,.T.);
#19926=EDGE_CURVE('',#15086,#15982,#9491,.T.);
#19927=EDGE_CURVE('',#15983,#15079,#9492,.T.);
#19928=EDGE_CURVE('',#15982,#15979,#9493,.T.);
#19929=EDGE_CURVE('',#15980,#15981,#9494,.T.);
#19930=EDGE_CURVE('',#15084,#15978,#9495,.T.);
#19931=EDGE_CURVE('',#15979,#15085,#9496,.T.);
#19932=EDGE_CURVE('',#15990,#15991,#9497,.T.);
#19933=EDGE_CURVE('',#15992,#15990,#9498,.T.);
#19934=EDGE_CURVE('',#15991,#15992,#9499,.T.);
#19935=EDGE_CURVE('',#15993,#15994,#9500,.T.);
#19936=EDGE_CURVE('',#15995,#15993,#9501,.T.);
#19937=EDGE_CURVE('',#15994,#15995,#9502,.T.);
#19938=EDGE_CURVE('',#15996,#15997,#9503,.T.);
#19939=EDGE_CURVE('',#15998,#15996,#9504,.T.);
#19940=EDGE_CURVE('',#15997,#15998,#9505,.T.);
#19941=EDGE_CURVE('',#15090,#15998,#9506,.T.);
#19942=EDGE_CURVE('',#15996,#15091,#9507,.T.);
#19943=EDGE_CURVE('',#15999,#16000,#9508,.T.);
#19944=EDGE_CURVE('',#16001,#15999,#9509,.T.);
#19945=EDGE_CURVE('',#16000,#16001,#9510,.T.);
#19946=EDGE_CURVE('',#15088,#16001,#9511,.T.);
#19947=EDGE_CURVE('',#15999,#15089,#9512,.T.);
#19948=EDGE_CURVE('',#15993,#16000,#9513,.T.);
#19949=EDGE_CURVE('',#16001,#15995,#9514,.T.);
#19950=EDGE_CURVE('',#16000,#15997,#9515,.T.);
#19951=EDGE_CURVE('',#15998,#15999,#9516,.T.);
#19952=EDGE_CURVE('',#15990,#15996,#9517,.T.);
#19953=EDGE_CURVE('',#15997,#15992,#9518,.T.);
#19954=EDGE_CURVE('',#15094,#15994,#9519,.T.);
#19955=EDGE_CURVE('',#15995,#15087,#9520,.T.);
#19956=EDGE_CURVE('',#15994,#15991,#9521,.T.);
#19957=EDGE_CURVE('',#15992,#15993,#9522,.T.);
#19958=EDGE_CURVE('',#15092,#15990,#9523,.T.);
#19959=EDGE_CURVE('',#15991,#15093,#9524,.T.);
#19960=EDGE_CURVE('',#16002,#16003,#9525,.T.);
#19961=EDGE_CURVE('',#16003,#15101,#9526,.T.);
#19962=EDGE_CURVE('',#15100,#16004,#9527,.T.);
#19963=EDGE_CURVE('',#16004,#16002,#9528,.T.);
#19964=EDGE_CURVE('',#16005,#16003,#9529,.T.);
#19965=EDGE_CURVE('',#15102,#16005,#9530,.T.);
#19966=EDGE_CURVE('',#16006,#16002,#9531,.T.);
#19967=EDGE_CURVE('',#16006,#16007,#9532,.T.);
#19968=EDGE_CURVE('',#16007,#16005,#9533,.T.);
#19969=EDGE_CURVE('',#16004,#16008,#9534,.T.);
#19970=EDGE_CURVE('',#16008,#16009,#9535,.T.);
#19971=EDGE_CURVE('',#16009,#16006,#9536,.T.);
#19972=EDGE_CURVE('',#16010,#16007,#9537,.T.);
#19973=EDGE_CURVE('',#16005,#16010,#9538,.T.);
#19974=EDGE_CURVE('',#16011,#16008,#9539,.T.);
#19975=EDGE_CURVE('',#16009,#16011,#9540,.T.);
#19976=EDGE_CURVE('',#15098,#16011,#9541,.T.);
#19977=EDGE_CURVE('',#16008,#15099,#9542,.T.);
#19978=EDGE_CURVE('',#16012,#16013,#9543,.T.);
#19979=EDGE_CURVE('',#16014,#16012,#9544,.T.);
#19980=EDGE_CURVE('',#16013,#16014,#9545,.T.);
#19981=EDGE_CURVE('',#15096,#16014,#9546,.T.);
#19982=EDGE_CURVE('',#16012,#15097,#9547,.T.);
#19983=EDGE_CURVE('',#16007,#16013,#9548,.T.);
#19984=EDGE_CURVE('',#16014,#16010,#9549,.T.);
#19985=EDGE_CURVE('',#16013,#16009,#9550,.T.);
#19986=EDGE_CURVE('',#16011,#16012,#9551,.T.);
#19987=EDGE_CURVE('',#16010,#15095,#9552,.T.);
#19988=EDGE_CURVE('',#16015,#16016,#9553,.T.);
#19989=EDGE_CURVE('',#16017,#16015,#9554,.T.);
#19990=EDGE_CURVE('',#16016,#16017,#9555,.T.);
#19991=EDGE_CURVE('',#16018,#16019,#9556,.T.);
#19992=EDGE_CURVE('',#16020,#16018,#9557,.T.);
#19993=EDGE_CURVE('',#16019,#16020,#9558,.T.);
#19994=EDGE_CURVE('',#16021,#16022,#9559,.T.);
#19995=EDGE_CURVE('',#16023,#16021,#9560,.T.);
#19996=EDGE_CURVE('',#16022,#16023,#9561,.T.);
#19997=EDGE_CURVE('',#15106,#16023,#9562,.T.);
#19998=EDGE_CURVE('',#16021,#15107,#9563,.T.);
#19999=EDGE_CURVE('',#16024,#16025,#9564,.T.);
#20000=EDGE_CURVE('',#16026,#16024,#9565,.T.);
#20001=EDGE_CURVE('',#16025,#16026,#9566,.T.);
#20002=EDGE_CURVE('',#15104,#16026,#9567,.T.);
#20003=EDGE_CURVE('',#16024,#15105,#9568,.T.);
#20004=EDGE_CURVE('',#16018,#16025,#9569,.T.);
#20005=EDGE_CURVE('',#16026,#16020,#9570,.T.);
#20006=EDGE_CURVE('',#16025,#16022,#9571,.T.);
#20007=EDGE_CURVE('',#16023,#16024,#9572,.T.);
#20008=EDGE_CURVE('',#16015,#16021,#9573,.T.);
#20009=EDGE_CURVE('',#16022,#16017,#9574,.T.);
#20010=EDGE_CURVE('',#15110,#16019,#9575,.T.);
#20011=EDGE_CURVE('',#16020,#15103,#9576,.T.);
#20012=EDGE_CURVE('',#16019,#16016,#9577,.T.);
#20013=EDGE_CURVE('',#16017,#16018,#9578,.T.);
#20014=EDGE_CURVE('',#15108,#16015,#9579,.T.);
#20015=EDGE_CURVE('',#16016,#15109,#9580,.T.);
#20016=EDGE_CURVE('',#16027,#16028,#9581,.T.);
#20017=EDGE_CURVE('',#16029,#16027,#9582,.T.);
#20018=EDGE_CURVE('',#16028,#16029,#9583,.T.);
#20019=EDGE_CURVE('',#16030,#16031,#9584,.T.);
#20020=EDGE_CURVE('',#16031,#16029,#9585,.T.);
#20021=EDGE_CURVE('',#16027,#16032,#9586,.T.);
#20022=EDGE_CURVE('',#16032,#16030,#9587,.T.);
#20023=EDGE_CURVE('',#15118,#16028,#9588,.T.);
#20024=EDGE_CURVE('',#16029,#15111,#9589,.T.);
#20025=EDGE_CURVE('',#16033,#16034,#9590,.T.);
#20026=EDGE_CURVE('',#16035,#16033,#9591,.T.);
#20027=EDGE_CURVE('',#16034,#16035,#9592,.T.);
#20028=EDGE_CURVE('',#16036,#16037,#9593,.T.);
#20029=EDGE_CURVE('',#16037,#16035,#9594,.T.);
#20030=EDGE_CURVE('',#16033,#16038,#9595,.T.);
#20031=EDGE_CURVE('',#16038,#16036,#9596,.T.);
#20032=EDGE_CURVE('',#16028,#16034,#9597,.T.);
#20033=EDGE_CURVE('',#16035,#16027,#9598,.T.);
#20034=EDGE_CURVE('',#15116,#16033,#9599,.T.);
#20035=EDGE_CURVE('',#16034,#15117,#9600,.T.);
#20036=EDGE_CURVE('',#16030,#16039,#9601,.T.);
#20037=EDGE_CURVE('',#16039,#15113,#9602,.T.);
#20038=EDGE_CURVE('',#15112,#16031,#9603,.T.);
#20039=EDGE_CURVE('',#16032,#16037,#9604,.T.);
#20040=EDGE_CURVE('',#16040,#16036,#9605,.T.);
#20041=EDGE_CURVE('',#16040,#16039,#9606,.T.);
#20042=EDGE_CURVE('',#16038,#15115,#9607,.T.);
#20043=EDGE_CURVE('',#15114,#16040,#9608,.T.);
#20044=EDGE_CURVE('',#16041,#16042,#9609,.T.);
#20045=EDGE_CURVE('',#16043,#16041,#9610,.T.);
#20046=EDGE_CURVE('',#16042,#16043,#9611,.T.);
#20047=EDGE_CURVE('',#16044,#16045,#9612,.T.);
#20048=EDGE_CURVE('',#16046,#16044,#9613,.T.);
#20049=EDGE_CURVE('',#16045,#16046,#9614,.T.);
#20050=EDGE_CURVE('',#16047,#16048,#9615,.T.);
#20051=EDGE_CURVE('',#16049,#16047,#9616,.T.);
#20052=EDGE_CURVE('',#16048,#16049,#9617,.T.);
#20053=EDGE_CURVE('',#15122,#16049,#9618,.T.);
#20054=EDGE_CURVE('',#16047,#15123,#9619,.T.);
#20055=EDGE_CURVE('',#16050,#16051,#9620,.T.);
#20056=EDGE_CURVE('',#16052,#16050,#9621,.T.);
#20057=EDGE_CURVE('',#16051,#16052,#9622,.T.);
#20058=EDGE_CURVE('',#15120,#16052,#9623,.T.);
#20059=EDGE_CURVE('',#16050,#15121,#9624,.T.);
#20060=EDGE_CURVE('',#16044,#16051,#9625,.T.);
#20061=EDGE_CURVE('',#16052,#16046,#9626,.T.);
#20062=EDGE_CURVE('',#16051,#16048,#9627,.T.);
#20063=EDGE_CURVE('',#16049,#16050,#9628,.T.);
#20064=EDGE_CURVE('',#16041,#16047,#9629,.T.);
#20065=EDGE_CURVE('',#16048,#16043,#9630,.T.);
#20066=EDGE_CURVE('',#15126,#16045,#9631,.T.);
#20067=EDGE_CURVE('',#16046,#15119,#9632,.T.);
#20068=EDGE_CURVE('',#16045,#16042,#9633,.T.);
#20069=EDGE_CURVE('',#16043,#16044,#9634,.T.);
#20070=EDGE_CURVE('',#15124,#16041,#9635,.T.);
#20071=EDGE_CURVE('',#16042,#15125,#9636,.T.);
#20072=EDGE_CURVE('',#16053,#16054,#9637,.T.);
#20073=EDGE_CURVE('',#16055,#16053,#9638,.T.);
#20074=EDGE_CURVE('',#16054,#16055,#9639,.T.);
#20075=EDGE_CURVE('',#16056,#16057,#9640,.T.);
#20076=EDGE_CURVE('',#16058,#16056,#9641,.T.);
#20077=EDGE_CURVE('',#16057,#16058,#9642,.T.);
#20078=EDGE_CURVE('',#16059,#16060,#9643,.T.);
#20079=EDGE_CURVE('',#16061,#16059,#9644,.T.);
#20080=EDGE_CURVE('',#16060,#16061,#9645,.T.);
#20081=EDGE_CURVE('',#15130,#16061,#9646,.T.);
#20082=EDGE_CURVE('',#16059,#15131,#9647,.T.);
#20083=EDGE_CURVE('',#16062,#16063,#9648,.T.);
#20084=EDGE_CURVE('',#16064,#16062,#9649,.T.);
#20085=EDGE_CURVE('',#16063,#16064,#9650,.T.);
#20086=EDGE_CURVE('',#15128,#16064,#9651,.T.);
#20087=EDGE_CURVE('',#16062,#15129,#9652,.T.);
#20088=EDGE_CURVE('',#16056,#16063,#9653,.T.);
#20089=EDGE_CURVE('',#16064,#16058,#9654,.T.);
#20090=EDGE_CURVE('',#16063,#16060,#9655,.T.);
#20091=EDGE_CURVE('',#16061,#16062,#9656,.T.);
#20092=EDGE_CURVE('',#16053,#16059,#9657,.T.);
#20093=EDGE_CURVE('',#16060,#16055,#9658,.T.);
#20094=EDGE_CURVE('',#15134,#16057,#9659,.T.);
#20095=EDGE_CURVE('',#16058,#15127,#9660,.T.);
#20096=EDGE_CURVE('',#16057,#16054,#9661,.T.);
#20097=EDGE_CURVE('',#16055,#16056,#9662,.T.);
#20098=EDGE_CURVE('',#15132,#16053,#9663,.T.);
#20099=EDGE_CURVE('',#16054,#15133,#9664,.T.);
#20100=EDGE_CURVE('',#16065,#16066,#13852,.T.);
#20101=EDGE_CURVE('',#16066,#16065,#13853,.T.);
#20102=EDGE_CURVE('',#16065,#16067,#9665,.T.);
#20103=EDGE_CURVE('',#16067,#16068,#13854,.T.);
#20104=EDGE_CURVE('',#16068,#16067,#13855,.T.);
#20105=EDGE_CURVE('',#16066,#16069,#9666,.T.);
#20106=EDGE_CURVE('',#16070,#16069,#13856,.T.);
#20107=EDGE_CURVE('',#16069,#16070,#13857,.T.);
#20108=EDGE_CURVE('',#16071,#16071,#13858,.T.);
#20109=EDGE_CURVE('',#16071,#16068,#9667,.T.);
#20110=EDGE_CURVE('',#16072,#16073,#9668,.T.);
#20111=EDGE_CURVE('',#16074,#16072,#9669,.T.);
#20112=EDGE_CURVE('',#16073,#16074,#9670,.T.);
#20113=EDGE_CURVE('',#16075,#16076,#9671,.T.);
#20114=EDGE_CURVE('',#16077,#16075,#9672,.T.);
#20115=EDGE_CURVE('',#16076,#16077,#9673,.T.);
#20116=EDGE_CURVE('',#16078,#16079,#9674,.T.);
#20117=EDGE_CURVE('',#16080,#16078,#9675,.T.);
#20118=EDGE_CURVE('',#16079,#16080,#9676,.T.);
#20119=EDGE_CURVE('',#15138,#16080,#9677,.T.);
#20120=EDGE_CURVE('',#16078,#15139,#9678,.T.);
#20121=EDGE_CURVE('',#16081,#16082,#9679,.T.);
#20122=EDGE_CURVE('',#16083,#16081,#9680,.T.);
#20123=EDGE_CURVE('',#16082,#16083,#9681,.T.);
#20124=EDGE_CURVE('',#15136,#16083,#9682,.T.);
#20125=EDGE_CURVE('',#16081,#15137,#9683,.T.);
#20126=EDGE_CURVE('',#16075,#16082,#9684,.T.);
#20127=EDGE_CURVE('',#16083,#16077,#9685,.T.);
#20128=EDGE_CURVE('',#16082,#16079,#9686,.T.);
#20129=EDGE_CURVE('',#16080,#16081,#9687,.T.);
#20130=EDGE_CURVE('',#16072,#16078,#9688,.T.);
#20131=EDGE_CURVE('',#16079,#16074,#9689,.T.);
#20132=EDGE_CURVE('',#15142,#16076,#9690,.T.);
#20133=EDGE_CURVE('',#16077,#15135,#9691,.T.);
#20134=EDGE_CURVE('',#16076,#16073,#9692,.T.);
#20135=EDGE_CURVE('',#16074,#16075,#9693,.T.);
#20136=EDGE_CURVE('',#15140,#16072,#9694,.T.);
#20137=EDGE_CURVE('',#16073,#15141,#9695,.T.);
#20138=EDGE_CURVE('',#16084,#16085,#9696,.T.);
#20139=EDGE_CURVE('',#16086,#16084,#9697,.T.);
#20140=EDGE_CURVE('',#16085,#16086,#9698,.T.);
#20141=EDGE_CURVE('',#16087,#16088,#9699,.T.);
#20142=EDGE_CURVE('',#16089,#16087,#9700,.T.);
#20143=EDGE_CURVE('',#16088,#16089,#9701,.T.);
#20144=EDGE_CURVE('',#16090,#16091,#9702,.T.);
#20145=EDGE_CURVE('',#16092,#16090,#9703,.T.);
#20146=EDGE_CURVE('',#16091,#16092,#9704,.T.);
#20147=EDGE_CURVE('',#15146,#16092,#9705,.T.);
#20148=EDGE_CURVE('',#16090,#15147,#9706,.T.);
#20149=EDGE_CURVE('',#16093,#16094,#9707,.T.);
#20150=EDGE_CURVE('',#16095,#16093,#9708,.T.);
#20151=EDGE_CURVE('',#16094,#16095,#9709,.T.);
#20152=EDGE_CURVE('',#15144,#16095,#9710,.T.);
#20153=EDGE_CURVE('',#16093,#15145,#9711,.T.);
#20154=EDGE_CURVE('',#16087,#16094,#9712,.T.);
#20155=EDGE_CURVE('',#16095,#16089,#9713,.T.);
#20156=EDGE_CURVE('',#16094,#16091,#9714,.T.);
#20157=EDGE_CURVE('',#16092,#16093,#9715,.T.);
#20158=EDGE_CURVE('',#16084,#16090,#9716,.T.);
#20159=EDGE_CURVE('',#16091,#16086,#9717,.T.);
#20160=EDGE_CURVE('',#15150,#16088,#9718,.T.);
#20161=EDGE_CURVE('',#16089,#15143,#9719,.T.);
#20162=EDGE_CURVE('',#16088,#16085,#9720,.T.);
#20163=EDGE_CURVE('',#16086,#16087,#9721,.T.);
#20164=EDGE_CURVE('',#15148,#16084,#9722,.T.);
#20165=EDGE_CURVE('',#16085,#15149,#9723,.T.);
#20166=EDGE_CURVE('',#16096,#16097,#13859,.T.);
#20167=EDGE_CURVE('',#16097,#16096,#13860,.T.);
#20168=EDGE_CURVE('',#16096,#16098,#9724,.T.);
#20169=EDGE_CURVE('',#16098,#16099,#13861,.T.);
#20170=EDGE_CURVE('',#16099,#16098,#13862,.T.);
#20171=EDGE_CURVE('',#16099,#16100,#9725,.T.);
#20172=EDGE_CURVE('',#16101,#16100,#13863,.T.);
#20173=EDGE_CURVE('',#16100,#16101,#13864,.T.);
#20174=EDGE_CURVE('',#14578,#16097,#9726,.T.);
#20175=EDGE_CURVE('',#16102,#16102,#13865,.T.);
#20176=EDGE_CURVE('',#16102,#16070,#9727,.T.);
#20177=EDGE_CURVE('',#16103,#16103,#13866,.T.);
#20178=EDGE_CURVE('',#16104,#16104,#13867,.T.);
#20179=EDGE_CURVE('',#16104,#16101,#9728,.T.);
#20180=EDGE_CURVE('',#16104,#16105,#9729,.T.);
#20181=EDGE_CURVE('',#16105,#16105,#13868,.T.);
#20182=EDGE_CURVE('',#16105,#16103,#9730,.T.);
#20183=EDGE_CURVE('',#15178,#16106,#9731,.T.);
#20184=EDGE_CURVE('',#16106,#16106,#13869,.T.);
#20185=EDGE_CURVE('',#15179,#16107,#9732,.T.);
#20186=EDGE_CURVE('',#16107,#16107,#13870,.T.);
#20187=EDGE_CURVE('',#15180,#16108,#9733,.T.);
#20188=EDGE_CURVE('',#16108,#16108,#13871,.T.);
#20189=EDGE_CURVE('',#15181,#16109,#9734,.T.);
#20190=EDGE_CURVE('',#16109,#16109,#13872,.T.);
#20191=EDGE_CURVE('',#15182,#16110,#9735,.T.);
#20192=EDGE_CURVE('',#16110,#16110,#13873,.T.);
#20193=EDGE_CURVE('',#16111,#16111,#13874,.T.);
#20194=EDGE_CURVE('',#16111,#16112,#9736,.T.);
#20195=EDGE_CURVE('',#16112,#16112,#13875,.T.);
#20196=EDGE_CURVE('',#16112,#16113,#9737,.T.);
#20197=EDGE_CURVE('',#16113,#16113,#13876,.T.);
#20198=EDGE_CURVE('',#16114,#15156,#9738,.T.);
#20199=EDGE_CURVE('',#15177,#16114,#13877,.T.);
#20200=EDGE_CURVE('',#16115,#15158,#9739,.T.);
#20201=EDGE_CURVE('',#16114,#16115,#13878,.T.);
#20202=EDGE_CURVE('',#16116,#15160,#9740,.T.);
#20203=EDGE_CURVE('',#16115,#16116,#13879,.T.);
#20204=EDGE_CURVE('',#16116,#15172,#13880,.T.);
#20205=EDGE_CURVE('',#14551,#16117,#9741,.T.);
#20206=EDGE_CURVE('',#16117,#16117,#13881,.T.);
#20207=EDGE_CURVE('',#16111,#16118,#9742,.T.);
#20208=EDGE_CURVE('',#16118,#16118,#13882,.T.);
#20209=EDGE_CURVE('',#14545,#16119,#9743,.T.);
#20210=EDGE_CURVE('',#16119,#16119,#13883,.T.);
#20211=EDGE_CURVE('',#16120,#16120,#13884,.T.);
#20212=EDGE_CURVE('',#16120,#16121,#9744,.T.);
#20213=EDGE_CURVE('',#16121,#16121,#13885,.T.);
#20214=EDGE_CURVE('',#16121,#14540,#9745,.T.);
#20215=EDGE_CURVE('',#16122,#16122,#13886,.T.);
#20216=EDGE_CURVE('',#16122,#14538,#9746,.T.);
#20217=EDGE_CURVE('',#16123,#16123,#13887,.T.);
#20218=EDGE_CURVE('',#16123,#16124,#9747,.T.);
#20219=EDGE_CURVE('',#16124,#16124,#13888,.T.);
#20220=EDGE_CURVE('',#16124,#16071,#9748,.T.);
#20221=EDGE_CURVE('',#16125,#16126,#9749,.T.);
#20222=EDGE_CURVE('',#16125,#16127,#357,.T.);
#20223=EDGE_CURVE('',#16128,#16127,#358,.T.);
#20224=EDGE_CURVE('',#16129,#16128,#359,.T.);
#20225=EDGE_CURVE('',#16130,#16129,#360,.T.);
#20226=EDGE_CURVE('',#16131,#16130,#361,.T.);
#20227=EDGE_CURVE('',#16126,#16131,#362,.T.);
#20228=EDGE_CURVE('',#16132,#16133,#9750,.T.);
#20229=EDGE_CURVE('',#16132,#16125,#363,.T.);
#20230=EDGE_CURVE('',#16133,#16126,#364,.T.);
#20231=EDGE_CURVE('',#16134,#16135,#9751,.T.);
#20232=EDGE_CURVE('',#16134,#16132,#365,.T.);
#20233=EDGE_CURVE('',#16135,#16133,#366,.T.);
#20234=EDGE_CURVE('',#16136,#16137,#9752,.T.);
#20235=EDGE_CURVE('',#16136,#16134,#367,.T.);
#20236=EDGE_CURVE('',#16137,#16135,#368,.T.);
#20237=EDGE_CURVE('',#16138,#16139,#9753,.T.);
#20238=EDGE_CURVE('',#16138,#16136,#369,.T.);
#20239=EDGE_CURVE('',#16139,#16137,#370,.T.);
#20240=EDGE_CURVE('',#16140,#16141,#9754,.T.);
#20241=EDGE_CURVE('',#16140,#16138,#371,.T.);
#20242=EDGE_CURVE('',#16141,#16139,#372,.T.);
#20243=EDGE_CURVE('',#16142,#16143,#9755,.T.);
#20244=EDGE_CURVE('',#16142,#16144,#373,.T.);
#20245=EDGE_CURVE('',#16145,#16144,#13889,.T.);
#20246=EDGE_CURVE('',#16143,#16145,#374,.T.);
#20247=EDGE_CURVE('',#16146,#16147,#9756,.T.);
#20248=EDGE_CURVE('',#16146,#16142,#375,.T.);
#20249=EDGE_CURVE('',#16147,#16143,#376,.T.);
#20250=EDGE_CURVE('',#16148,#16149,#9757,.T.);
#20251=EDGE_CURVE('',#16148,#16146,#377,.T.);
#20252=EDGE_CURVE('',#16149,#16147,#378,.T.);
#20253=EDGE_CURVE('',#16150,#16150,#13890,.T.);
#20254=EDGE_CURVE('',#16150,#16151,#9758,.T.);
#20255=EDGE_CURVE('',#16151,#16151,#13891,.T.);
#20256=EDGE_CURVE('',#16152,#16151,#9759,.T.);
#20257=EDGE_CURVE('',#16153,#16153,#13892,.T.);
#20258=EDGE_CURVE('',#16154,#16155,#9760,.F.);
#20259=EDGE_CURVE('',#16155,#16156,#9761,.T.);
#20260=EDGE_CURVE('',#16156,#16157,#9762,.F.);
#20261=EDGE_CURVE('',#16157,#16154,#9763,.T.);
#20262=EDGE_CURVE('',#16155,#16158,#9764,.T.);
#20263=EDGE_CURVE('',#16158,#16159,#9765,.T.);
#20264=EDGE_CURVE('',#16156,#16159,#9766,.T.);
#20265=EDGE_CURVE('',#16160,#16161,#9767,.T.);
#20266=EDGE_CURVE('',#16161,#16162,#9768,.T.);
#20267=EDGE_CURVE('',#16162,#16163,#9769,.T.);
#20268=EDGE_CURVE('',#16163,#16164,#9770,.T.);
#20269=EDGE_CURVE('',#16164,#16165,#9771,.T.);
#20270=EDGE_CURVE('',#16165,#16160,#9772,.T.);
#20271=EDGE_CURVE('',#16166,#16164,#9773,.T.);
#20272=EDGE_CURVE('',#16167,#16166,#9774,.T.);
#20273=EDGE_CURVE('',#16165,#16167,#9775,.T.);
#20274=EDGE_CURVE('',#16168,#16163,#9776,.T.);
#20275=EDGE_CURVE('',#16168,#16169,#9777,.T.);
#20276=EDGE_CURVE('',#16169,#16166,#9778,.T.);
#20277=EDGE_CURVE('',#16162,#16170,#9779,.T.);
#20278=EDGE_CURVE('',#16171,#16170,#9780,.T.);
#20279=EDGE_CURVE('',#16172,#16171,#9781,.T.);
#20280=EDGE_CURVE('',#16172,#16168,#9782,.T.);
#20281=EDGE_CURVE('',#16173,#16174,#9783,.T.);
#20282=EDGE_CURVE('',#16175,#16173,#9784,.T.);
#20283=EDGE_CURVE('',#16174,#16175,#9785,.T.);
#20284=EDGE_CURVE('',#16170,#16175,#9786,.T.);
#20285=EDGE_CURVE('',#16173,#16176,#9787,.T.);
#20286=EDGE_CURVE('',#16176,#16171,#9788,.T.);
#20287=EDGE_CURVE('',#16160,#16177,#9789,.T.);
#20288=EDGE_CURVE('',#16177,#16174,#9790,.T.);
#20289=EDGE_CURVE('',#16175,#16161,#9791,.T.);
#20290=EDGE_CURVE('',#16178,#16179,#9792,.T.);
#20291=EDGE_CURVE('',#16180,#16178,#9793,.T.);
#20292=EDGE_CURVE('',#16179,#16180,#9794,.T.);
#20293=EDGE_CURVE('',#16181,#16182,#9795,.T.);
#20294=EDGE_CURVE('',#16182,#16180,#9796,.T.);
#20295=EDGE_CURVE('',#16178,#16183,#9797,.T.);
#20296=EDGE_CURVE('',#16183,#16181,#9798,.T.);
#20297=EDGE_CURVE('',#16174,#16179,#9799,.T.);
#20298=EDGE_CURVE('',#16180,#16173,#9800,.T.);
#20299=EDGE_CURVE('',#16184,#16185,#9801,.T.);
#20300=EDGE_CURVE('',#16186,#16184,#9802,.T.);
#20301=EDGE_CURVE('',#16185,#16186,#9803,.T.);
#20302=EDGE_CURVE('',#16187,#16188,#9804,.T.);
#20303=EDGE_CURVE('',#16188,#16186,#9805,.T.);
#20304=EDGE_CURVE('',#16184,#16189,#9806,.T.);
#20305=EDGE_CURVE('',#16189,#16187,#9807,.T.);
#20306=EDGE_CURVE('',#16179,#16185,#9808,.T.);
#20307=EDGE_CURVE('',#16186,#16178,#9809,.T.);
#20308=EDGE_CURVE('',#16190,#16191,#9810,.T.);
#20309=EDGE_CURVE('',#16192,#16190,#9811,.T.);
#20310=EDGE_CURVE('',#16191,#16192,#9812,.T.);
#20311=EDGE_CURVE('',#16193,#16194,#9813,.T.);
#20312=EDGE_CURVE('',#16194,#16192,#9814,.T.);
#20313=EDGE_CURVE('',#16190,#16195,#9815,.T.);
#20314=EDGE_CURVE('',#16195,#16193,#9816,.T.);
#20315=EDGE_CURVE('',#16185,#16191,#9817,.T.);
#20316=EDGE_CURVE('',#16192,#16184,#9818,.T.);
#20317=EDGE_CURVE('',#16196,#16197,#9819,.T.);
#20318=EDGE_CURVE('',#16198,#16196,#9820,.T.);
#20319=EDGE_CURVE('',#16197,#16198,#9821,.T.);
#20320=EDGE_CURVE('',#16199,#16200,#9822,.T.);
#20321=EDGE_CURVE('',#16200,#16198,#9823,.T.);
#20322=EDGE_CURVE('',#16196,#16201,#9824,.T.);
#20323=EDGE_CURVE('',#16201,#16199,#9825,.T.);
#20324=EDGE_CURVE('',#16191,#16197,#9826,.T.);
#20325=EDGE_CURVE('',#16198,#16190,#9827,.T.);
#20326=EDGE_CURVE('',#16202,#16203,#9828,.T.);
#20327=EDGE_CURVE('',#16204,#16202,#9829,.T.);
#20328=EDGE_CURVE('',#16203,#16204,#9830,.T.);
#20329=EDGE_CURVE('',#16205,#16206,#9831,.T.);
#20330=EDGE_CURVE('',#16206,#16204,#9832,.T.);
#20331=EDGE_CURVE('',#16202,#16207,#9833,.T.);
#20332=EDGE_CURVE('',#16207,#16205,#9834,.T.);
#20333=EDGE_CURVE('',#16197,#16203,#9835,.T.);
#20334=EDGE_CURVE('',#16204,#16196,#9836,.T.);
#20335=EDGE_CURVE('',#16208,#16209,#9837,.T.);
#20336=EDGE_CURVE('',#16209,#16202,#9838,.T.);
#20337=EDGE_CURVE('',#16203,#16210,#9839,.T.);
#20338=EDGE_CURVE('',#16210,#16208,#9840,.T.);
#20339=EDGE_CURVE('',#16211,#16187,#9841,.T.);
#20340=EDGE_CURVE('',#16211,#16212,#9842,.T.);
#20341=EDGE_CURVE('',#16212,#16181,#9843,.T.);
#20342=EDGE_CURVE('',#16183,#16188,#9844,.T.);
#20343=EDGE_CURVE('',#16189,#16194,#9845,.T.);
#20344=EDGE_CURVE('',#16213,#16193,#9846,.T.);
#20345=EDGE_CURVE('',#16213,#16211,#9847,.T.);
#20346=EDGE_CURVE('',#16195,#16200,#9848,.T.);
#20347=EDGE_CURVE('',#16214,#16199,#9849,.T.);
#20348=EDGE_CURVE('',#16214,#16213,#9850,.T.);
#20349=EDGE_CURVE('',#16201,#16206,#9851,.T.);
#20350=EDGE_CURVE('',#16215,#16205,#9852,.T.);
#20351=EDGE_CURVE('',#16215,#16214,#9853,.T.);
#20352=EDGE_CURVE('',#16207,#16216,#9854,.T.);
#20353=EDGE_CURVE('',#16216,#16169,#9855,.T.);
#20354=EDGE_CURVE('',#16169,#16215,#9856,.T.);
#20355=EDGE_CURVE('',#16216,#16209,#9857,.T.);
#20356=EDGE_CURVE('',#16208,#16167,#9858,.T.);
#20357=EDGE_CURVE('',#16166,#16216,#9859,.T.);
#20358=EDGE_CURVE('',#16217,#16217,#13893,.T.);
#20359=EDGE_CURVE('',#16217,#16218,#9860,.T.);
#20360=EDGE_CURVE('',#16218,#16218,#13894,.T.);
#20361=EDGE_CURVE('',#16210,#16177,#9861,.T.);
#20362=EDGE_CURVE('',#16219,#16219,#13895,.T.);
#20363=EDGE_CURVE('',#16220,#16220,#13896,.T.);
#20364=EDGE_CURVE('',#16221,#16221,#13897,.T.);
#20365=EDGE_CURVE('',#16222,#16222,#13898,.T.);
#20366=EDGE_CURVE('',#16223,#16223,#13899,.T.);
#20367=EDGE_CURVE('',#16223,#16218,#9862,.T.);
#20368=EDGE_CURVE('',#16219,#16224,#9863,.T.);
#20369=EDGE_CURVE('',#16224,#16224,#13900,.T.);
#20370=EDGE_CURVE('',#16225,#16225,#13901,.T.);
#20371=EDGE_CURVE('',#16225,#16224,#9864,.T.);
#20372=EDGE_CURVE('',#16222,#16226,#9865,.T.);
#20373=EDGE_CURVE('',#16226,#16226,#13902,.T.);
#20374=EDGE_CURVE('',#16227,#16227,#13903,.T.);
#20375=EDGE_CURVE('',#16227,#16226,#9866,.T.);
#20376=EDGE_CURVE('',#16220,#16228,#9867,.T.);
#20377=EDGE_CURVE('',#16228,#16228,#13904,.T.);
#20378=EDGE_CURVE('',#16229,#16229,#13905,.T.);
#20379=EDGE_CURVE('',#16229,#16228,#9868,.T.);
#20380=EDGE_CURVE('',#16230,#16230,#13906,.T.);
#20381=EDGE_CURVE('',#16230,#16229,#9869,.T.);
#20382=EDGE_CURVE('',#16212,#16172,#9870,.T.);
#20383=EDGE_CURVE('',#16231,#16231,#13907,.T.);
#20384=EDGE_CURVE('',#16232,#16232,#13908,.T.);
#20385=EDGE_CURVE('',#16233,#16233,#13909,.T.);
#20386=EDGE_CURVE('',#16234,#16234,#13910,.T.);
#20387=EDGE_CURVE('',#16231,#16227,#9871,.T.);
#20388=EDGE_CURVE('',#16234,#16225,#9872,.T.);
#20389=EDGE_CURVE('',#16232,#16223,#9873,.T.);
#20390=EDGE_CURVE('',#16176,#16182,#9874,.T.);
#20391=EDGE_CURVE('',#16235,#16236,#13911,.T.);
#20392=EDGE_CURVE('',#16236,#16235,#13912,.T.);
#20393=EDGE_CURVE('',#16235,#16237,#9875,.T.);
#20394=EDGE_CURVE('',#16237,#16238,#13913,.T.);
#20395=EDGE_CURVE('',#16238,#16237,#13914,.T.);
#20396=EDGE_CURVE('',#16238,#16239,#9876,.T.);
#20397=EDGE_CURVE('',#16240,#16239,#13915,.T.);
#20398=EDGE_CURVE('',#16239,#16240,#13916,.T.);
#20399=EDGE_CURVE('',#16233,#16236,#9877,.T.);
#20400=EDGE_CURVE('',#16240,#16241,#9878,.T.);
#20401=EDGE_CURVE('',#16241,#16241,#13917,.T.);
#20402=EDGE_CURVE('',#16242,#16243,#379,.T.);
#20403=EDGE_CURVE('',#16242,#16244,#380,.T.);
#20404=EDGE_CURVE('',#16245,#16244,#381,.T.);
#20405=EDGE_CURVE('',#16246,#16245,#382,.T.);
#20406=EDGE_CURVE('',#16243,#16246,#383,.T.);
#20407=EDGE_CURVE('',#16247,#16248,#384,.T.);
#20408=EDGE_CURVE('',#16249,#16247,#385,.T.);
#20409=EDGE_CURVE('',#16250,#16249,#386,.T.);
#20410=EDGE_CURVE('',#16251,#16250,#387,.T.);
#20411=EDGE_CURVE('',#16252,#16251,#388,.T.);
#20412=EDGE_CURVE('',#16253,#16252,#389,.T.);
#20413=EDGE_CURVE('',#16254,#16253,#390,.T.);
#20414=EDGE_CURVE('',#16255,#16254,#391,.T.);
#20415=EDGE_CURVE('',#16255,#16149,#392,.T.);
#20416=EDGE_CURVE('',#16256,#16145,#393,.T.);
#20417=EDGE_CURVE('',#16248,#16256,#394,.T.);
#20418=EDGE_CURVE('',#16257,#16258,#395,.T.);
#20419=EDGE_CURVE('',#16259,#16257,#396,.T.);
#20420=EDGE_CURVE('',#16260,#16259,#397,.T.);
#20421=EDGE_CURVE('',#16260,#16141,#398,.T.);
#20422=EDGE_CURVE('',#16261,#16131,#399,.T.);
#20423=EDGE_CURVE('',#16262,#16261,#400,.T.);
#20424=EDGE_CURVE('',#16263,#16262,#401,.T.);
#20425=EDGE_CURVE('',#16264,#16263,#402,.T.);
#20426=EDGE_CURVE('',#16265,#16264,#403,.T.);
#20427=EDGE_CURVE('',#16266,#16265,#404,.T.);
#20428=EDGE_CURVE('',#16267,#16266,#405,.T.);
#20429=EDGE_CURVE('',#16268,#16267,#406,.T.);
#20430=EDGE_CURVE('',#16269,#16268,#407,.T.);
#20431=EDGE_CURVE('',#16270,#16269,#408,.T.);
#20432=EDGE_CURVE('',#16271,#16270,#409,.T.);
#20433=EDGE_CURVE('',#16272,#16271,#410,.T.);
#20434=EDGE_CURVE('',#16258,#16272,#411,.T.);
#20435=EDGE_CURVE('',#16273,#16128,#412,.T.);
#20436=EDGE_CURVE('',#16274,#16273,#413,.T.);
#20437=EDGE_CURVE('',#16129,#16274,#414,.T.);
#20438=EDGE_CURVE('',#16275,#16276,#415,.T.);
#20439=EDGE_CURVE('',#16277,#16275,#416,.T.);
#20440=EDGE_CURVE('',#16278,#16277,#417,.T.);
#20441=EDGE_CURVE('',#16278,#16276,#418,.T.);
#20442=EDGE_CURVE('',#16279,#16280,#419,.T.);
#20443=EDGE_CURVE('',#16279,#16281,#420,.T.);
#20444=EDGE_CURVE('',#16282,#16281,#421,.T.);
#20445=EDGE_CURVE('',#16280,#16282,#422,.T.);
#20446=EDGE_CURVE('',#16283,#16284,#423,.T.);
#20447=EDGE_CURVE('',#16285,#16283,#424,.T.);
#20448=EDGE_CURVE('',#16144,#16285,#425,.T.);
#20449=EDGE_CURVE('',#16286,#16148,#426,.T.);
#20450=EDGE_CURVE('',#16287,#16286,#427,.T.);
#20451=EDGE_CURVE('',#16288,#16287,#428,.T.);
#20452=EDGE_CURVE('',#16289,#16288,#429,.T.);
#20453=EDGE_CURVE('',#16290,#16289,#430,.T.);
#20454=EDGE_CURVE('',#16291,#16290,#431,.T.);
#20455=EDGE_CURVE('',#16284,#16291,#432,.T.);
#20456=EDGE_CURVE('',#16292,#16293,#433,.T.);
#20457=EDGE_CURVE('',#16294,#16292,#434,.T.);
#20458=EDGE_CURVE('',#16295,#16294,#435,.T.);
#20459=EDGE_CURVE('',#16293,#16295,#436,.T.);
#20460=EDGE_CURVE('',#16296,#16297,#437,.T.);
#20461=EDGE_CURVE('',#16298,#16296,#438,.T.);
#20462=EDGE_CURVE('',#16299,#16298,#439,.T.);
#20463=EDGE_CURVE('',#16297,#16299,#440,.T.);
#20464=EDGE_CURVE('',#16300,#16301,#441,.T.);
#20465=EDGE_CURVE('',#16302,#16300,#442,.T.);
#20466=EDGE_CURVE('',#16303,#16302,#443,.T.);
#20467=EDGE_CURVE('',#16304,#16303,#444,.T.);
#20468=EDGE_CURVE('',#16305,#16304,#445,.T.);
#20469=EDGE_CURVE('',#16306,#16305,#446,.T.);
#20470=EDGE_CURVE('',#16307,#16306,#447,.T.);
#20471=EDGE_CURVE('',#16308,#16307,#448,.T.);
#20472=EDGE_CURVE('',#16309,#16308,#449,.T.);
#20473=EDGE_CURVE('',#16310,#16309,#450,.T.);
#20474=EDGE_CURVE('',#16311,#16310,#451,.T.);
#20475=EDGE_CURVE('',#16312,#16311,#452,.T.);
#20476=EDGE_CURVE('',#16127,#16312,#453,.T.);
#20477=EDGE_CURVE('',#16313,#16140,#454,.T.);
#20478=EDGE_CURVE('',#16314,#16313,#455,.T.);
#20479=EDGE_CURVE('',#16301,#16314,#456,.T.);
#20480=EDGE_CURVE('',#16315,#16316,#457,.T.);
#20481=EDGE_CURVE('',#16317,#16315,#458,.T.);
#20482=EDGE_CURVE('',#16318,#16317,#459,.T.);
#20483=EDGE_CURVE('',#16316,#16318,#460,.T.);
#20484=EDGE_CURVE('',#16293,#16255,#461,.T.);
#20485=EDGE_CURVE('',#16286,#16295,#462,.T.);
#20486=EDGE_CURVE('',#16313,#16260,#13918,.T.);
#20487=EDGE_CURVE('',#16297,#16242,#463,.T.);
#20488=EDGE_CURVE('',#16244,#16299,#464,.T.);
#20489=EDGE_CURVE('',#16276,#16315,#465,.T.);
#20490=EDGE_CURVE('',#16317,#16278,#466,.T.);
#20491=EDGE_CURVE('',#16319,#16279,#467,.T.);
#20492=EDGE_CURVE('',#16319,#16320,#468,.T.);
#20493=EDGE_CURVE('',#16281,#16320,#469,.T.);
#20494=EDGE_CURVE('',#16321,#16285,#13919,.F.);
#20495=EDGE_CURVE('',#16256,#16321,#13920,.F.);
#20496=EDGE_CURVE('',#16322,#16323,#9879,.T.);
#20497=EDGE_CURVE('',#16322,#16314,#13921,.T.);
#20498=EDGE_CURVE('',#16259,#16324,#13922,.T.);
#20499=EDGE_CURVE('',#16324,#16323,#13923,.T.);
#20500=EDGE_CURVE('',#16325,#16319,#470,.T.);
#20501=EDGE_CURVE('',#16326,#16325,#471,.T.);
#20502=EDGE_CURVE('',#16320,#16326,#472,.T.);
#20503=EDGE_CURVE('',#16327,#16261,#13924,.T.);
#20504=EDGE_CURVE('',#16262,#16327,#9880,.F.);
#20505=EDGE_CURVE('',#16264,#16310,#9881,.F.);
#20506=EDGE_CURVE('',#16311,#16263,#9882,.F.);
#20507=EDGE_CURVE('',#16309,#16265,#9883,.F.);
#20508=EDGE_CURVE('',#16266,#16308,#9884,.F.);
#20509=EDGE_CURVE('',#16307,#16267,#9885,.F.);
#20510=EDGE_CURVE('',#16268,#16306,#9886,.F.);
#20511=EDGE_CURVE('',#16305,#16269,#9887,.F.);
#20512=EDGE_CURVE('',#16270,#16304,#9888,.F.);
#20513=EDGE_CURVE('',#16303,#16271,#9889,.F.);
#20514=EDGE_CURVE('',#16272,#16302,#9890,.F.);
#20515=EDGE_CURVE('',#16300,#16258,#9891,.F.);
#20516=EDGE_CURVE('',#16257,#16301,#9892,.F.);
#20517=EDGE_CURVE('',#16252,#16290,#9893,.F.);
#20518=EDGE_CURVE('',#16291,#16251,#9894,.F.);
#20519=EDGE_CURVE('',#16250,#16284,#9895,.F.);
#20520=EDGE_CURVE('',#16283,#16249,#9896,.F.);
#20521=EDGE_CURVE('',#16328,#16248,#9897,.F.);
#20522=EDGE_CURVE('',#16329,#16328,#181,.T.);
#20523=EDGE_CURVE('',#16247,#16329,#9898,.F.);
#20524=EDGE_CURVE('',#16254,#16245,#13925,.T.);
#20525=EDGE_CURVE('',#16289,#16253,#9899,.F.);
#20526=EDGE_CURVE('',#16246,#16288,#9900,.F.);
#20527=EDGE_CURVE('',#16287,#16243,#473,.F.);
#20528=EDGE_CURVE('',#16285,#16329,#13926,.F.);
#20529=EDGE_CURVE('',#16328,#16256,#13927,.F.);
#20530=EDGE_CURVE('',#16282,#16294,#474,.F.);
#20531=EDGE_CURVE('',#16292,#16280,#475,.T.);
#20532=EDGE_CURVE('',#16314,#16259,#13928,.T.);
#20533=EDGE_CURVE('',#16318,#16330,#476,.F.);
#20534=EDGE_CURVE('',#16330,#16312,#477,.F.);
#20535=EDGE_CURVE('',#16327,#16316,#478,.T.);
#20536=EDGE_CURVE('',#16275,#16298,#479,.T.);
#20537=EDGE_CURVE('',#16296,#16277,#480,.F.);
#20538=EDGE_CURVE('',#16273,#16326,#481,.F.);
#20539=EDGE_CURVE('',#16330,#16130,#9901,.T.);
#20540=EDGE_CURVE('',#16325,#16274,#482,.T.);
#20541=EDGE_CURVE('',#16331,#16331,#13929,.T.);
#20542=EDGE_CURVE('',#16331,#16221,#9902,.T.);
#20543=EDGE_CURVE('',#16332,#16332,#13930,.T.);
#20544=EDGE_CURVE('',#16332,#16331,#9903,.T.);
#20545=EDGE_CURVE('',#16333,#16333,#13931,.T.);
#20546=EDGE_CURVE('',#16334,#16334,#13932,.T.);
#20547=EDGE_CURVE('',#16334,#16333,#9904,.T.);
#20548=EDGE_CURVE('',#16335,#16335,#13933,.T.);
#20549=EDGE_CURVE('',#16335,#16334,#9905,.T.);
#20550=EDGE_CURVE('',#16336,#16336,#13934,.T.);
#20551=EDGE_CURVE('',#16336,#16335,#9906,.T.);
#20552=EDGE_CURVE('',#16337,#16337,#13935,.T.);
#20553=EDGE_CURVE('',#16337,#16336,#9907,.T.);
#20554=EDGE_CURVE('',#16338,#16339,#13936,.T.);
#20555=EDGE_CURVE('',#16159,#16338,#9908,.T.);
#20556=EDGE_CURVE('',#16339,#16158,#9909,.T.);
#20557=EDGE_CURVE('',#16340,#16154,#9910,.T.);
#20558=EDGE_CURVE('',#16339,#16340,#9911,.T.);
#20559=EDGE_CURVE('',#16341,#16338,#9912,.T.);
#20560=EDGE_CURVE('',#16342,#16340,#13937,.T.);
#20561=EDGE_CURVE('',#16342,#16337,#9913,.T.);
#20562=EDGE_CURVE('',#16341,#16342,#13938,.T.);
#20563=EDGE_CURVE('',#16157,#16341,#9914,.T.);
#20564=EDGE_CURVE('',#16343,#16343,#13939,.T.);
#20565=EDGE_CURVE('',#16344,#16344,#13940,.T.);
#20566=EDGE_CURVE('',#16344,#16343,#9915,.T.);
#20567=EDGE_CURVE('',#16322,#16323,#182,.T.);
#20568=EDGE_CURVE('',#16324,#16344,#9916,.T.);
#20569=EDGE_CURVE('',#16153,#16321,#9917,.T.);
#20570=EDGE_CURVE('',#16345,#16346,#13941,.T.);
#20571=EDGE_CURVE('',#16346,#16345,#13942,.T.);
#20572=EDGE_CURVE('',#16345,#16347,#9918,.T.);
#20573=EDGE_CURVE('',#16347,#16347,#13943,.T.);
#20574=EDGE_CURVE('',#16348,#16348,#13944,.T.);
#20575=EDGE_CURVE('',#16346,#16349,#9919,.T.);
#20576=EDGE_CURVE('',#16349,#16349,#13945,.T.);
#20577=EDGE_CURVE('',#16350,#16350,#13946,.T.);
#20578=EDGE_CURVE('',#16350,#16351,#9920,.T.);
#20579=EDGE_CURVE('',#16351,#16352,#13947,.T.);
#20580=EDGE_CURVE('',#16352,#16351,#13948,.T.);
#20581=EDGE_CURVE('',#16353,#16353,#13949,.T.);
#20582=EDGE_CURVE('',#16354,#16354,#13950,.T.);
#20583=EDGE_CURVE('',#16354,#16352,#9921,.T.);
#20584=EDGE_CURVE('',#16355,#16355,#13951,.T.);
#20585=EDGE_CURVE('',#16355,#16356,#13952,.T.);
#20586=EDGE_CURVE('',#16356,#16356,#13953,.T.);
#20587=EDGE_CURVE('',#16357,#16357,#13954,.T.);
#20588=EDGE_CURVE('',#16358,#16358,#13955,.T.);
#20589=EDGE_CURVE('',#16358,#16353,#9922,.T.);
#20590=EDGE_CURVE('',#16359,#16359,#13956,.T.);
#20591=EDGE_CURVE('',#16359,#16358,#9923,.T.);
#20592=EDGE_CURVE('',#16348,#16359,#9924,.T.);
#20593=EDGE_CURVE('',#16349,#16360,#9925,.T.);
#20594=EDGE_CURVE('',#16360,#16360,#13957,.T.);
#20595=EDGE_CURVE('',#16360,#16361,#9926,.T.);
#20596=EDGE_CURVE('',#16361,#16361,#13958,.T.);
#20597=EDGE_CURVE('',#16361,#16362,#9927,.T.);
#20598=EDGE_CURVE('',#16362,#16362,#13959,.T.);
#20599=EDGE_CURVE('',#16362,#16357,#9928,.T.);
#20600=EDGE_CURVE('',#16363,#16363,#13960,.T.);
#20601=EDGE_CURVE('',#16363,#16364,#9929,.T.);
#20602=EDGE_CURVE('',#16364,#16364,#13961,.T.);
#20603=EDGE_CURVE('',#16365,#16365,#13962,.T.);
#20604=EDGE_CURVE('',#16365,#16363,#9930,.T.);
#20605=EDGE_CURVE('',#16366,#16366,#13963,.T.);
#20606=EDGE_CURVE('',#16366,#16365,#9931,.T.);
#20607=EDGE_CURVE('',#16367,#16367,#13964,.T.);
#20608=EDGE_CURVE('',#16367,#16368,#9932,.T.);
#20609=EDGE_CURVE('',#16368,#16368,#13965,.T.);
#20610=EDGE_CURVE('',#16368,#16369,#9933,.T.);
#20611=EDGE_CURVE('',#16369,#16369,#13966,.T.);
#20612=EDGE_CURVE('',#16369,#16370,#9934,.T.);
#20613=EDGE_CURVE('',#16370,#16370,#13967,.T.);
#20614=EDGE_CURVE('',#16371,#16372,#13968,.T.);
#20615=EDGE_CURVE('',#16372,#16371,#13969,.T.);
#20616=EDGE_CURVE('',#16371,#16373,#9935,.T.);
#20617=EDGE_CURVE('',#16373,#16373,#13970,.T.);
#20618=EDGE_CURVE('',#16374,#16374,#13971,.T.);
#20619=EDGE_CURVE('',#16375,#16375,#13972,.T.);
#20620=EDGE_CURVE('',#16375,#16372,#9936,.T.);
#20621=EDGE_CURVE('',#16376,#16376,#13973,.T.);
#20622=EDGE_CURVE('',#16376,#16377,#9937,.T.);
#20623=EDGE_CURVE('',#16377,#16378,#13974,.T.);
#20624=EDGE_CURVE('',#16378,#16377,#13975,.T.);
#20625=EDGE_CURVE('',#16378,#16379,#9938,.T.);
#20626=EDGE_CURVE('',#16379,#16379,#13976,.T.);
#20627=EDGE_CURVE('',#16380,#16380,#13977,.T.);
#20628=EDGE_CURVE('',#16381,#16382,#483,.T.);
#20629=EDGE_CURVE('',#16381,#16383,#13978,.T.);
#20630=EDGE_CURVE('',#16383,#16384,#13979,.T.);
#20631=EDGE_CURVE('',#16384,#16384,#13980,.T.);
#20632=EDGE_CURVE('',#16383,#16382,#13981,.T.);
#20633=EDGE_CURVE('',#16385,#16381,#484,.T.);
#20634=EDGE_CURVE('',#16386,#16385,#13982,.T.);
#20635=EDGE_CURVE('',#16387,#16386,#13983,.T.);
#20636=EDGE_CURVE('',#16382,#16387,#485,.T.);
#20637=EDGE_CURVE('',#16388,#16388,#13984,.T.);
#20638=EDGE_CURVE('',#16388,#16386,#13985,.T.);
#20639=EDGE_CURVE('',#16387,#16385,#486,.T.);
#20640=EDGE_CURVE('',#16389,#16390,#487,.T.);
#20641=EDGE_CURVE('',#16389,#16391,#13986,.T.);
#20642=EDGE_CURVE('',#16391,#16392,#13987,.T.);
#20643=EDGE_CURVE('',#16392,#16392,#13988,.T.);
#20644=EDGE_CURVE('',#16391,#16390,#13989,.T.);
#20645=EDGE_CURVE('',#16393,#16389,#488,.T.);
#20646=EDGE_CURVE('',#16394,#16393,#13990,.T.);
#20647=EDGE_CURVE('',#16395,#16394,#13991,.T.);
#20648=EDGE_CURVE('',#16390,#16395,#489,.T.);
#20649=EDGE_CURVE('',#16396,#16396,#13992,.T.);
#20650=EDGE_CURVE('',#16396,#16394,#13993,.T.);
#20651=EDGE_CURVE('',#16395,#16393,#490,.T.);
#20652=EDGE_CURVE('',#16397,#16398,#491,.T.);
#20653=EDGE_CURVE('',#16397,#16399,#13994,.T.);
#20654=EDGE_CURVE('',#16399,#16400,#13995,.T.);
#20655=EDGE_CURVE('',#16400,#16400,#13996,.T.);
#20656=EDGE_CURVE('',#16399,#16398,#13997,.T.);
#20657=EDGE_CURVE('',#16401,#16397,#492,.T.);
#20658=EDGE_CURVE('',#16402,#16401,#13998,.T.);
#20659=EDGE_CURVE('',#16403,#16402,#13999,.T.);
#20660=EDGE_CURVE('',#16398,#16403,#493,.T.);
#20661=EDGE_CURVE('',#16404,#16404,#14000,.T.);
#20662=EDGE_CURVE('',#16404,#16402,#14001,.T.);
#20663=EDGE_CURVE('',#16403,#16401,#494,.T.);
#20664=EDGE_CURVE('',#16405,#16406,#495,.T.);
#20665=EDGE_CURVE('',#16405,#16407,#14002,.T.);
#20666=EDGE_CURVE('',#16407,#16408,#14003,.T.);
#20667=EDGE_CURVE('',#16408,#16408,#14004,.T.);
#20668=EDGE_CURVE('',#16407,#16406,#14005,.T.);
#20669=EDGE_CURVE('',#16409,#16405,#496,.T.);
#20670=EDGE_CURVE('',#16410,#16409,#14006,.T.);
#20671=EDGE_CURVE('',#16411,#16410,#14007,.T.);
#20672=EDGE_CURVE('',#16406,#16411,#497,.T.);
#20673=EDGE_CURVE('',#16412,#16412,#14008,.T.);
#20674=EDGE_CURVE('',#16412,#16410,#14009,.T.);
#20675=EDGE_CURVE('',#16411,#16409,#498,.T.);
#20676=EDGE_CURVE('',#16413,#16414,#499,.T.);
#20677=EDGE_CURVE('',#16413,#16415,#14010,.T.);
#20678=EDGE_CURVE('',#16415,#16416,#14011,.T.);
#20679=EDGE_CURVE('',#16416,#16416,#14012,.T.);
#20680=EDGE_CURVE('',#16415,#16414,#14013,.T.);
#20681=EDGE_CURVE('',#16417,#16413,#500,.T.);
#20682=EDGE_CURVE('',#16418,#16417,#14014,.T.);
#20683=EDGE_CURVE('',#16419,#16418,#14015,.T.);
#20684=EDGE_CURVE('',#16414,#16419,#501,.T.);
#20685=EDGE_CURVE('',#16420,#16420,#14016,.T.);
#20686=EDGE_CURVE('',#16420,#16418,#14017,.T.);
#20687=EDGE_CURVE('',#16419,#16417,#502,.T.);
#20688=EDGE_CURVE('',#16421,#16422,#503,.T.);
#20689=EDGE_CURVE('',#16421,#16423,#14018,.T.);
#20690=EDGE_CURVE('',#16423,#16424,#14019,.T.);
#20691=EDGE_CURVE('',#16424,#16424,#14020,.T.);
#20692=EDGE_CURVE('',#16423,#16422,#14021,.T.);
#20693=EDGE_CURVE('',#16425,#16421,#504,.T.);
#20694=EDGE_CURVE('',#16426,#16425,#14022,.T.);
#20695=EDGE_CURVE('',#16427,#16426,#14023,.T.);
#20696=EDGE_CURVE('',#16422,#16427,#505,.T.);
#20697=EDGE_CURVE('',#16428,#16428,#14024,.T.);
#20698=EDGE_CURVE('',#16428,#16426,#14025,.T.);
#20699=EDGE_CURVE('',#16427,#16425,#506,.T.);
#20700=EDGE_CURVE('',#16429,#16430,#507,.T.);
#20701=EDGE_CURVE('',#16429,#16431,#14026,.T.);
#20702=EDGE_CURVE('',#16431,#16432,#14027,.T.);
#20703=EDGE_CURVE('',#16432,#16432,#14028,.T.);
#20704=EDGE_CURVE('',#16431,#16430,#14029,.T.);
#20705=EDGE_CURVE('',#16433,#16429,#508,.T.);
#20706=EDGE_CURVE('',#16434,#16433,#14030,.T.);
#20707=EDGE_CURVE('',#16435,#16434,#14031,.T.);
#20708=EDGE_CURVE('',#16430,#16435,#509,.T.);
#20709=EDGE_CURVE('',#16436,#16436,#14032,.T.);
#20710=EDGE_CURVE('',#16436,#16434,#14033,.T.);
#20711=EDGE_CURVE('',#16435,#16433,#510,.T.);
#20712=EDGE_CURVE('',#16437,#16438,#511,.T.);
#20713=EDGE_CURVE('',#16437,#16439,#14034,.T.);
#20714=EDGE_CURVE('',#16439,#16440,#14035,.T.);
#20715=EDGE_CURVE('',#16440,#16440,#14036,.T.);
#20716=EDGE_CURVE('',#16439,#16438,#14037,.T.);
#20717=EDGE_CURVE('',#16441,#16437,#512,.T.);
#20718=EDGE_CURVE('',#16442,#16441,#14038,.T.);
#20719=EDGE_CURVE('',#16443,#16442,#14039,.T.);
#20720=EDGE_CURVE('',#16438,#16443,#513,.T.);
#20721=EDGE_CURVE('',#16444,#16444,#14040,.T.);
#20722=EDGE_CURVE('',#16444,#16442,#14041,.T.);
#20723=EDGE_CURVE('',#16443,#16441,#514,.T.);
#20724=EDGE_CURVE('',#16445,#16446,#515,.T.);
#20725=EDGE_CURVE('',#16445,#16447,#14042,.T.);
#20726=EDGE_CURVE('',#16447,#16448,#14043,.T.);
#20727=EDGE_CURVE('',#16448,#16448,#14044,.T.);
#20728=EDGE_CURVE('',#16447,#16446,#14045,.T.);
#20729=EDGE_CURVE('',#16449,#16445,#516,.T.);
#20730=EDGE_CURVE('',#16450,#16449,#14046,.T.);
#20731=EDGE_CURVE('',#16451,#16450,#14047,.T.);
#20732=EDGE_CURVE('',#16446,#16451,#517,.T.);
#20733=EDGE_CURVE('',#16452,#16452,#14048,.T.);
#20734=EDGE_CURVE('',#16452,#16450,#14049,.T.);
#20735=EDGE_CURVE('',#16451,#16449,#518,.T.);
#20736=EDGE_CURVE('',#16453,#16454,#519,.T.);
#20737=EDGE_CURVE('',#16453,#16455,#14050,.T.);
#20738=EDGE_CURVE('',#16455,#16456,#14051,.T.);
#20739=EDGE_CURVE('',#16456,#16456,#14052,.T.);
#20740=EDGE_CURVE('',#16455,#16454,#14053,.T.);
#20741=EDGE_CURVE('',#16457,#16453,#520,.T.);
#20742=EDGE_CURVE('',#16458,#16457,#14054,.T.);
#20743=EDGE_CURVE('',#16459,#16458,#14055,.T.);
#20744=EDGE_CURVE('',#16454,#16459,#521,.T.);
#20745=EDGE_CURVE('',#16460,#16460,#14056,.T.);
#20746=EDGE_CURVE('',#16460,#16458,#14057,.T.);
#20747=EDGE_CURVE('',#16459,#16457,#522,.T.);
#20748=EDGE_CURVE('',#16461,#16462,#523,.T.);
#20749=EDGE_CURVE('',#16461,#16463,#14058,.T.);
#20750=EDGE_CURVE('',#16463,#16464,#14059,.T.);
#20751=EDGE_CURVE('',#16464,#16464,#14060,.T.);
#20752=EDGE_CURVE('',#16463,#16465,#14061,.T.);
#20753=EDGE_CURVE('',#16462,#16465,#524,.T.);
#20754=EDGE_CURVE('',#16466,#16461,#525,.T.);
#20755=EDGE_CURVE('',#16467,#16466,#14062,.T.);
#20756=EDGE_CURVE('',#16468,#16467,#14063,.T.);
#20757=EDGE_CURVE('',#16465,#16468,#526,.T.);
#20758=EDGE_CURVE('',#16469,#16469,#14064,.T.);
#20759=EDGE_CURVE('',#16469,#16467,#14065,.T.);
#20760=EDGE_CURVE('',#16470,#16466,#527,.T.);
#20761=EDGE_CURVE('',#16468,#16470,#528,.T.);
#20762=EDGE_CURVE('',#16471,#16472,#529,.T.);
#20763=EDGE_CURVE('',#16471,#16473,#14066,.T.);
#20764=EDGE_CURVE('',#16473,#16474,#14067,.T.);
#20765=EDGE_CURVE('',#16474,#16474,#14068,.T.);
#20766=EDGE_CURVE('',#16473,#16472,#14069,.T.);
#20767=EDGE_CURVE('',#16475,#16471,#530,.T.);
#20768=EDGE_CURVE('',#16476,#16475,#14070,.T.);
#20769=EDGE_CURVE('',#16477,#16476,#14071,.T.);
#20770=EDGE_CURVE('',#16472,#16477,#531,.T.);
#20771=EDGE_CURVE('',#16478,#16478,#14072,.T.);
#20772=EDGE_CURVE('',#16478,#16476,#14073,.T.);
#20773=EDGE_CURVE('',#16477,#16475,#532,.T.);
#20774=EDGE_CURVE('',#16479,#16480,#533,.T.);
#20775=EDGE_CURVE('',#16479,#16481,#14074,.T.);
#20776=EDGE_CURVE('',#16481,#16482,#14075,.T.);
#20777=EDGE_CURVE('',#16482,#16482,#14076,.T.);
#20778=EDGE_CURVE('',#16481,#16480,#14077,.T.);
#20779=EDGE_CURVE('',#16483,#16479,#534,.T.);
#20780=EDGE_CURVE('',#16484,#16483,#14078,.T.);
#20781=EDGE_CURVE('',#16485,#16484,#14079,.T.);
#20782=EDGE_CURVE('',#16480,#16485,#535,.T.);
#20783=EDGE_CURVE('',#16486,#16486,#14080,.T.);
#20784=EDGE_CURVE('',#16486,#16484,#14081,.T.);
#20785=EDGE_CURVE('',#16485,#16483,#536,.T.);
#20786=EDGE_CURVE('',#16487,#16488,#537,.T.);
#20787=EDGE_CURVE('',#16487,#16489,#14082,.T.);
#20788=EDGE_CURVE('',#16489,#16490,#14083,.T.);
#20789=EDGE_CURVE('',#16490,#16490,#14084,.T.);
#20790=EDGE_CURVE('',#16489,#16488,#14085,.T.);
#20791=EDGE_CURVE('',#16491,#16487,#538,.T.);
#20792=EDGE_CURVE('',#16492,#16491,#14086,.T.);
#20793=EDGE_CURVE('',#16493,#16492,#14087,.T.);
#20794=EDGE_CURVE('',#16488,#16493,#539,.T.);
#20795=EDGE_CURVE('',#16494,#16494,#14088,.T.);
#20796=EDGE_CURVE('',#16494,#16492,#14089,.T.);
#20797=EDGE_CURVE('',#16493,#16491,#540,.T.);
#20798=EDGE_CURVE('',#16495,#16496,#541,.T.);
#20799=EDGE_CURVE('',#16495,#16497,#14090,.T.);
#20800=EDGE_CURVE('',#16497,#16498,#14091,.T.);
#20801=EDGE_CURVE('',#16498,#16498,#14092,.T.);
#20802=EDGE_CURVE('',#16497,#16496,#14093,.T.);
#20803=EDGE_CURVE('',#16499,#16495,#542,.T.);
#20804=EDGE_CURVE('',#16500,#16499,#14094,.T.);
#20805=EDGE_CURVE('',#16501,#16500,#14095,.T.);
#20806=EDGE_CURVE('',#16496,#16501,#543,.T.);
#20807=EDGE_CURVE('',#16502,#16502,#14096,.T.);
#20808=EDGE_CURVE('',#16502,#16500,#14097,.T.);
#20809=EDGE_CURVE('',#16501,#16499,#544,.T.);
#20810=EDGE_CURVE('',#16503,#16504,#545,.T.);
#20811=EDGE_CURVE('',#16503,#16505,#14098,.T.);
#20812=EDGE_CURVE('',#16505,#16506,#14099,.T.);
#20813=EDGE_CURVE('',#16506,#16506,#14100,.T.);
#20814=EDGE_CURVE('',#16505,#16504,#14101,.T.);
#20815=EDGE_CURVE('',#16507,#16503,#546,.T.);
#20816=EDGE_CURVE('',#16508,#16507,#14102,.T.);
#20817=EDGE_CURVE('',#16509,#16508,#14103,.T.);
#20818=EDGE_CURVE('',#16504,#16509,#547,.T.);
#20819=EDGE_CURVE('',#16510,#16510,#14104,.T.);
#20820=EDGE_CURVE('',#16510,#16508,#14105,.T.);
#20821=EDGE_CURVE('',#16509,#16507,#548,.T.);
#20822=EDGE_CURVE('',#16511,#16512,#549,.T.);
#20823=EDGE_CURVE('',#16511,#16513,#14106,.T.);
#20824=EDGE_CURVE('',#16513,#16514,#14107,.T.);
#20825=EDGE_CURVE('',#16514,#16514,#14108,.T.);
#20826=EDGE_CURVE('',#16513,#16512,#14109,.T.);
#20827=EDGE_CURVE('',#16515,#16511,#550,.T.);
#20828=EDGE_CURVE('',#16516,#16515,#14110,.T.);
#20829=EDGE_CURVE('',#16517,#16516,#14111,.T.);
#20830=EDGE_CURVE('',#16512,#16517,#551,.T.);
#20831=EDGE_CURVE('',#16518,#16518,#14112,.T.);
#20832=EDGE_CURVE('',#16518,#16516,#14113,.T.);
#20833=EDGE_CURVE('',#16517,#16515,#552,.T.);
#20834=EDGE_CURVE('',#16519,#16520,#553,.T.);
#20835=EDGE_CURVE('',#16519,#16521,#14114,.T.);
#20836=EDGE_CURVE('',#16521,#16522,#14115,.T.);
#20837=EDGE_CURVE('',#16522,#16522,#14116,.T.);
#20838=EDGE_CURVE('',#16521,#16520,#14117,.T.);
#20839=EDGE_CURVE('',#16523,#16519,#554,.T.);
#20840=EDGE_CURVE('',#16524,#16523,#14118,.T.);
#20841=EDGE_CURVE('',#16525,#16524,#14119,.T.);
#20842=EDGE_CURVE('',#16520,#16525,#555,.T.);
#20843=EDGE_CURVE('',#16526,#16526,#14120,.T.);
#20844=EDGE_CURVE('',#16526,#16524,#14121,.T.);
#20845=EDGE_CURVE('',#16525,#16523,#556,.T.);
#20846=EDGE_CURVE('',#16527,#16528,#557,.T.);
#20847=EDGE_CURVE('',#16527,#16529,#14122,.T.);
#20848=EDGE_CURVE('',#16529,#16530,#14123,.T.);
#20849=EDGE_CURVE('',#16530,#16530,#14124,.T.);
#20850=EDGE_CURVE('',#16529,#16528,#14125,.T.);
#20851=EDGE_CURVE('',#16531,#16527,#558,.T.);
#20852=EDGE_CURVE('',#16532,#16531,#14126,.T.);
#20853=EDGE_CURVE('',#16533,#16532,#14127,.T.);
#20854=EDGE_CURVE('',#16528,#16533,#559,.T.);
#20855=EDGE_CURVE('',#16534,#16534,#14128,.T.);
#20856=EDGE_CURVE('',#16534,#16532,#14129,.T.);
#20857=EDGE_CURVE('',#16533,#16531,#560,.T.);
#20858=EDGE_CURVE('',#16535,#16536,#561,.T.);
#20859=EDGE_CURVE('',#16535,#16537,#14130,.T.);
#20860=EDGE_CURVE('',#16537,#16538,#14131,.T.);
#20861=EDGE_CURVE('',#16538,#16538,#14132,.T.);
#20862=EDGE_CURVE('',#16537,#16536,#14133,.T.);
#20863=EDGE_CURVE('',#16539,#16535,#562,.T.);
#20864=EDGE_CURVE('',#16540,#16539,#14134,.T.);
#20865=EDGE_CURVE('',#16541,#16540,#14135,.T.);
#20866=EDGE_CURVE('',#16536,#16541,#563,.T.);
#20867=EDGE_CURVE('',#16542,#16542,#14136,.T.);
#20868=EDGE_CURVE('',#16542,#16540,#14137,.T.);
#20869=EDGE_CURVE('',#16541,#16539,#564,.T.);
#20870=EDGE_CURVE('',#16543,#16544,#565,.T.);
#20871=EDGE_CURVE('',#16543,#16545,#14138,.T.);
#20872=EDGE_CURVE('',#16545,#16546,#14139,.T.);
#20873=EDGE_CURVE('',#16546,#16546,#14140,.T.);
#20874=EDGE_CURVE('',#16545,#16544,#14141,.T.);
#20875=EDGE_CURVE('',#16547,#16543,#566,.T.);
#20876=EDGE_CURVE('',#16548,#16547,#14142,.T.);
#20877=EDGE_CURVE('',#16549,#16548,#14143,.T.);
#20878=EDGE_CURVE('',#16544,#16549,#567,.T.);
#20879=EDGE_CURVE('',#16550,#16550,#14144,.T.);
#20880=EDGE_CURVE('',#16550,#16548,#14145,.T.);
#20881=EDGE_CURVE('',#16549,#16547,#568,.T.);
#20882=EDGE_CURVE('',#16551,#16552,#569,.T.);
#20883=EDGE_CURVE('',#16551,#16553,#14146,.T.);
#20884=EDGE_CURVE('',#16553,#16554,#14147,.T.);
#20885=EDGE_CURVE('',#16554,#16554,#14148,.T.);
#20886=EDGE_CURVE('',#16553,#16552,#14149,.T.);
#20887=EDGE_CURVE('',#16555,#16551,#570,.T.);
#20888=EDGE_CURVE('',#16556,#16555,#14150,.T.);
#20889=EDGE_CURVE('',#16557,#16556,#14151,.T.);
#20890=EDGE_CURVE('',#16552,#16557,#571,.T.);
#20891=EDGE_CURVE('',#16558,#16558,#14152,.T.);
#20892=EDGE_CURVE('',#16558,#16556,#14153,.T.);
#20893=EDGE_CURVE('',#16557,#16555,#572,.T.);
#20894=EDGE_CURVE('',#16379,#16559,#9939,.T.);
#20895=EDGE_CURVE('',#16559,#16559,#14154,.T.);
#20896=EDGE_CURVE('',#16374,#16470,#9940,.T.);
#20897=EDGE_CURVE('',#16462,#16380,#9941,.T.);
#20898=EDGE_CURVE('',#16560,#16560,#14155,.T.);
#20899=EDGE_CURVE('',#16560,#16375,#9942,.T.);
#20900=EDGE_CURVE('',#16561,#16561,#14156,.T.);
#20901=EDGE_CURVE('',#16561,#16562,#9943,.T.);
#20902=EDGE_CURVE('',#16562,#16562,#14157,.T.);
#20903=EDGE_CURVE('',#16562,#16563,#9944,.T.);
#20904=EDGE_CURVE('',#16563,#16563,#14158,.T.);
#20905=EDGE_CURVE('',#16563,#16564,#9945,.T.);
#20906=EDGE_CURVE('',#16564,#16564,#14159,.T.);
#20907=EDGE_CURVE('',#16565,#16565,#14160,.T.);
#20908=EDGE_CURVE('',#16565,#16566,#9946,.T.);
#20909=EDGE_CURVE('',#16566,#16566,#14161,.T.);
#20910=EDGE_CURVE('',#16567,#16567,#14162,.T.);
#20911=EDGE_CURVE('',#16567,#16565,#9947,.T.);
#20912=EDGE_CURVE('',#16568,#16568,#14163,.T.);
#20913=EDGE_CURVE('',#16568,#16567,#9948,.T.);
#20914=EDGE_CURVE('',#16569,#16569,#14164,.T.);
#20915=EDGE_CURVE('',#16569,#16570,#9949,.T.);
#20916=EDGE_CURVE('',#16570,#16570,#14165,.T.);
#20917=EDGE_CURVE('',#16570,#16571,#9950,.T.);
#20918=EDGE_CURVE('',#16571,#16571,#14166,.T.);
#20919=EDGE_CURVE('',#16571,#16572,#9951,.T.);
#20920=EDGE_CURVE('',#16572,#16572,#14167,.T.);
#20921=EDGE_CURVE('',#16573,#16574,#14168,.T.);
#20922=EDGE_CURVE('',#16574,#16573,#14169,.T.);
#20923=EDGE_CURVE('',#16573,#16575,#9952,.T.);
#20924=EDGE_CURVE('',#16575,#16575,#14170,.T.);
#20925=EDGE_CURVE('',#16576,#16576,#14171,.T.);
#20926=EDGE_CURVE('',#16577,#16577,#14172,.T.);
#20927=EDGE_CURVE('',#16577,#16574,#9953,.T.);
#20928=EDGE_CURVE('',#16578,#16578,#14173,.T.);
#20929=EDGE_CURVE('',#16578,#16579,#9954,.T.);
#20930=EDGE_CURVE('',#16579,#16580,#14174,.T.);
#20931=EDGE_CURVE('',#16580,#16579,#14175,.T.);
#20932=EDGE_CURVE('',#16580,#16581,#9955,.T.);
#20933=EDGE_CURVE('',#16581,#16581,#14176,.T.);
#20934=EDGE_CURVE('',#16582,#16582,#14177,.T.);
#20935=EDGE_CURVE('',#16583,#16584,#573,.T.);
#20936=EDGE_CURVE('',#16583,#16585,#14178,.T.);
#20937=EDGE_CURVE('',#16585,#16586,#14179,.T.);
#20938=EDGE_CURVE('',#16586,#16586,#14180,.T.);
#20939=EDGE_CURVE('',#16585,#16584,#14181,.T.);
#20940=EDGE_CURVE('',#16587,#16583,#574,.T.);
#20941=EDGE_CURVE('',#16588,#16587,#14182,.T.);
#20942=EDGE_CURVE('',#16589,#16588,#14183,.T.);
#20943=EDGE_CURVE('',#16584,#16589,#575,.T.);
#20944=EDGE_CURVE('',#16590,#16590,#14184,.T.);
#20945=EDGE_CURVE('',#16590,#16588,#14185,.T.);
#20946=EDGE_CURVE('',#16589,#16587,#576,.T.);
#20947=EDGE_CURVE('',#16591,#16592,#577,.T.);
#20948=EDGE_CURVE('',#16591,#16593,#14186,.T.);
#20949=EDGE_CURVE('',#16593,#16594,#14187,.T.);
#20950=EDGE_CURVE('',#16594,#16594,#14188,.T.);
#20951=EDGE_CURVE('',#16593,#16592,#14189,.T.);
#20952=EDGE_CURVE('',#16595,#16591,#578,.T.);
#20953=EDGE_CURVE('',#16596,#16595,#14190,.T.);
#20954=EDGE_CURVE('',#16597,#16596,#14191,.T.);
#20955=EDGE_CURVE('',#16592,#16597,#579,.T.);
#20956=EDGE_CURVE('',#16598,#16598,#14192,.T.);
#20957=EDGE_CURVE('',#16598,#16596,#14193,.T.);
#20958=EDGE_CURVE('',#16597,#16595,#580,.T.);
#20959=EDGE_CURVE('',#16599,#16600,#581,.T.);
#20960=EDGE_CURVE('',#16599,#16601,#14194,.T.);
#20961=EDGE_CURVE('',#16601,#16602,#14195,.T.);
#20962=EDGE_CURVE('',#16602,#16602,#14196,.T.);
#20963=EDGE_CURVE('',#16601,#16600,#14197,.T.);
#20964=EDGE_CURVE('',#16603,#16599,#582,.T.);
#20965=EDGE_CURVE('',#16604,#16603,#14198,.T.);
#20966=EDGE_CURVE('',#16605,#16604,#14199,.T.);
#20967=EDGE_CURVE('',#16600,#16605,#583,.T.);
#20968=EDGE_CURVE('',#16606,#16606,#14200,.T.);
#20969=EDGE_CURVE('',#16606,#16604,#14201,.T.);
#20970=EDGE_CURVE('',#16605,#16603,#584,.T.);
#20971=EDGE_CURVE('',#16607,#16608,#585,.T.);
#20972=EDGE_CURVE('',#16607,#16609,#14202,.T.);
#20973=EDGE_CURVE('',#16609,#16610,#14203,.T.);
#20974=EDGE_CURVE('',#16610,#16610,#14204,.T.);
#20975=EDGE_CURVE('',#16609,#16608,#14205,.T.);
#20976=EDGE_CURVE('',#16611,#16607,#586,.T.);
#20977=EDGE_CURVE('',#16612,#16611,#14206,.T.);
#20978=EDGE_CURVE('',#16613,#16612,#14207,.T.);
#20979=EDGE_CURVE('',#16608,#16613,#587,.T.);
#20980=EDGE_CURVE('',#16614,#16614,#14208,.T.);
#20981=EDGE_CURVE('',#16614,#16612,#14209,.T.);
#20982=EDGE_CURVE('',#16613,#16611,#588,.T.);
#20983=EDGE_CURVE('',#16615,#16616,#589,.T.);
#20984=EDGE_CURVE('',#16615,#16617,#14210,.T.);
#20985=EDGE_CURVE('',#16617,#16618,#14211,.T.);
#20986=EDGE_CURVE('',#16618,#16618,#14212,.T.);
#20987=EDGE_CURVE('',#16617,#16616,#14213,.T.);
#20988=EDGE_CURVE('',#16619,#16615,#590,.T.);
#20989=EDGE_CURVE('',#16620,#16619,#14214,.T.);
#20990=EDGE_CURVE('',#16621,#16620,#14215,.T.);
#20991=EDGE_CURVE('',#16616,#16621,#591,.T.);
#20992=EDGE_CURVE('',#16622,#16622,#14216,.T.);
#20993=EDGE_CURVE('',#16622,#16620,#14217,.T.);
#20994=EDGE_CURVE('',#16621,#16619,#592,.T.);
#20995=EDGE_CURVE('',#16623,#16624,#593,.T.);
#20996=EDGE_CURVE('',#16623,#16625,#14218,.T.);
#20997=EDGE_CURVE('',#16625,#16626,#14219,.T.);
#20998=EDGE_CURVE('',#16626,#16626,#14220,.T.);
#20999=EDGE_CURVE('',#16625,#16624,#14221,.T.);
#21000=EDGE_CURVE('',#16627,#16623,#594,.T.);
#21001=EDGE_CURVE('',#16628,#16627,#14222,.T.);
#21002=EDGE_CURVE('',#16629,#16628,#14223,.T.);
#21003=EDGE_CURVE('',#16624,#16629,#595,.T.);
#21004=EDGE_CURVE('',#16630,#16630,#14224,.T.);
#21005=EDGE_CURVE('',#16630,#16628,#14225,.T.);
#21006=EDGE_CURVE('',#16629,#16627,#596,.T.);
#21007=EDGE_CURVE('',#16631,#16632,#597,.T.);
#21008=EDGE_CURVE('',#16631,#16633,#14226,.T.);
#21009=EDGE_CURVE('',#16633,#16634,#14227,.T.);
#21010=EDGE_CURVE('',#16634,#16634,#14228,.T.);
#21011=EDGE_CURVE('',#16633,#16632,#14229,.T.);
#21012=EDGE_CURVE('',#16635,#16631,#598,.T.);
#21013=EDGE_CURVE('',#16636,#16635,#14230,.T.);
#21014=EDGE_CURVE('',#16637,#16636,#14231,.T.);
#21015=EDGE_CURVE('',#16632,#16637,#599,.T.);
#21016=EDGE_CURVE('',#16638,#16638,#14232,.T.);
#21017=EDGE_CURVE('',#16638,#16636,#14233,.T.);
#21018=EDGE_CURVE('',#16637,#16635,#600,.T.);
#21019=EDGE_CURVE('',#16639,#16640,#601,.T.);
#21020=EDGE_CURVE('',#16639,#16641,#14234,.T.);
#21021=EDGE_CURVE('',#16641,#16642,#14235,.T.);
#21022=EDGE_CURVE('',#16642,#16642,#14236,.T.);
#21023=EDGE_CURVE('',#16641,#16640,#14237,.T.);
#21024=EDGE_CURVE('',#16643,#16639,#602,.T.);
#21025=EDGE_CURVE('',#16644,#16643,#14238,.T.);
#21026=EDGE_CURVE('',#16645,#16644,#14239,.T.);
#21027=EDGE_CURVE('',#16640,#16645,#603,.T.);
#21028=EDGE_CURVE('',#16646,#16646,#14240,.T.);
#21029=EDGE_CURVE('',#16646,#16644,#14241,.T.);
#21030=EDGE_CURVE('',#16645,#16643,#604,.T.);
#21031=EDGE_CURVE('',#16647,#16648,#605,.T.);
#21032=EDGE_CURVE('',#16647,#16649,#14242,.T.);
#21033=EDGE_CURVE('',#16649,#16650,#14243,.T.);
#21034=EDGE_CURVE('',#16650,#16650,#14244,.T.);
#21035=EDGE_CURVE('',#16649,#16648,#14245,.T.);
#21036=EDGE_CURVE('',#16651,#16647,#606,.T.);
#21037=EDGE_CURVE('',#16652,#16651,#14246,.T.);
#21038=EDGE_CURVE('',#16653,#16652,#14247,.T.);
#21039=EDGE_CURVE('',#16648,#16653,#607,.T.);
#21040=EDGE_CURVE('',#16654,#16654,#14248,.T.);
#21041=EDGE_CURVE('',#16654,#16652,#14249,.T.);
#21042=EDGE_CURVE('',#16653,#16651,#608,.T.);
#21043=EDGE_CURVE('',#16655,#16656,#609,.T.);
#21044=EDGE_CURVE('',#16655,#16657,#14250,.T.);
#21045=EDGE_CURVE('',#16657,#16658,#14251,.T.);
#21046=EDGE_CURVE('',#16658,#16658,#14252,.T.);
#21047=EDGE_CURVE('',#16657,#16659,#14253,.T.);
#21048=EDGE_CURVE('',#16656,#16659,#610,.T.);
#21049=EDGE_CURVE('',#16660,#16655,#611,.T.);
#21050=EDGE_CURVE('',#16661,#16660,#14254,.T.);
#21051=EDGE_CURVE('',#16662,#16661,#14255,.T.);
#21052=EDGE_CURVE('',#16659,#16662,#612,.T.);
#21053=EDGE_CURVE('',#16663,#16663,#14256,.T.);
#21054=EDGE_CURVE('',#16663,#16661,#14257,.T.);
#21055=EDGE_CURVE('',#16664,#16660,#613,.T.);
#21056=EDGE_CURVE('',#16662,#16664,#614,.T.);
#21057=EDGE_CURVE('',#16665,#16666,#615,.T.);
#21058=EDGE_CURVE('',#16665,#16667,#14258,.T.);
#21059=EDGE_CURVE('',#16667,#16668,#14259,.T.);
#21060=EDGE_CURVE('',#16668,#16668,#14260,.T.);
#21061=EDGE_CURVE('',#16667,#16666,#14261,.T.);
#21062=EDGE_CURVE('',#16669,#16665,#616,.T.);
#21063=EDGE_CURVE('',#16670,#16669,#14262,.T.);
#21064=EDGE_CURVE('',#16671,#16670,#14263,.T.);
#21065=EDGE_CURVE('',#16666,#16671,#617,.T.);
#21066=EDGE_CURVE('',#16672,#16672,#14264,.T.);
#21067=EDGE_CURVE('',#16672,#16670,#14265,.T.);
#21068=EDGE_CURVE('',#16671,#16669,#618,.T.);
#21069=EDGE_CURVE('',#16673,#16674,#619,.T.);
#21070=EDGE_CURVE('',#16673,#16675,#14266,.T.);
#21071=EDGE_CURVE('',#16675,#16676,#14267,.T.);
#21072=EDGE_CURVE('',#16676,#16676,#14268,.T.);
#21073=EDGE_CURVE('',#16675,#16674,#14269,.T.);
#21074=EDGE_CURVE('',#16677,#16673,#620,.T.);
#21075=EDGE_CURVE('',#16678,#16677,#14270,.T.);
#21076=EDGE_CURVE('',#16679,#16678,#14271,.T.);
#21077=EDGE_CURVE('',#16674,#16679,#621,.T.);
#21078=EDGE_CURVE('',#16680,#16680,#14272,.T.);
#21079=EDGE_CURVE('',#16680,#16678,#14273,.T.);
#21080=EDGE_CURVE('',#16679,#16677,#622,.T.);
#21081=EDGE_CURVE('',#16681,#16682,#623,.T.);
#21082=EDGE_CURVE('',#16681,#16683,#14274,.T.);
#21083=EDGE_CURVE('',#16683,#16684,#14275,.T.);
#21084=EDGE_CURVE('',#16684,#16684,#14276,.T.);
#21085=EDGE_CURVE('',#16683,#16682,#14277,.T.);
#21086=EDGE_CURVE('',#16685,#16681,#624,.T.);
#21087=EDGE_CURVE('',#16686,#16685,#14278,.T.);
#21088=EDGE_CURVE('',#16687,#16686,#14279,.T.);
#21089=EDGE_CURVE('',#16682,#16687,#625,.T.);
#21090=EDGE_CURVE('',#16688,#16688,#14280,.T.);
#21091=EDGE_CURVE('',#16688,#16686,#14281,.T.);
#21092=EDGE_CURVE('',#16687,#16685,#626,.T.);
#21093=EDGE_CURVE('',#16689,#16690,#627,.T.);
#21094=EDGE_CURVE('',#16689,#16691,#14282,.T.);
#21095=EDGE_CURVE('',#16691,#16692,#14283,.T.);
#21096=EDGE_CURVE('',#16692,#16692,#14284,.T.);
#21097=EDGE_CURVE('',#16691,#16690,#14285,.T.);
#21098=EDGE_CURVE('',#16693,#16689,#628,.T.);
#21099=EDGE_CURVE('',#16694,#16693,#14286,.T.);
#21100=EDGE_CURVE('',#16695,#16694,#14287,.T.);
#21101=EDGE_CURVE('',#16690,#16695,#629,.T.);
#21102=EDGE_CURVE('',#16696,#16696,#14288,.T.);
#21103=EDGE_CURVE('',#16696,#16694,#14289,.T.);
#21104=EDGE_CURVE('',#16695,#16693,#630,.T.);
#21105=EDGE_CURVE('',#16697,#16698,#631,.T.);
#21106=EDGE_CURVE('',#16697,#16699,#14290,.T.);
#21107=EDGE_CURVE('',#16699,#16700,#14291,.T.);
#21108=EDGE_CURVE('',#16700,#16700,#14292,.T.);
#21109=EDGE_CURVE('',#16699,#16698,#14293,.T.);
#21110=EDGE_CURVE('',#16701,#16697,#632,.T.);
#21111=EDGE_CURVE('',#16702,#16701,#14294,.T.);
#21112=EDGE_CURVE('',#16703,#16702,#14295,.T.);
#21113=EDGE_CURVE('',#16698,#16703,#633,.T.);
#21114=EDGE_CURVE('',#16704,#16704,#14296,.T.);
#21115=EDGE_CURVE('',#16704,#16702,#14297,.T.);
#21116=EDGE_CURVE('',#16703,#16701,#634,.T.);
#21117=EDGE_CURVE('',#16705,#16706,#635,.T.);
#21118=EDGE_CURVE('',#16705,#16707,#14298,.T.);
#21119=EDGE_CURVE('',#16707,#16708,#14299,.T.);
#21120=EDGE_CURVE('',#16708,#16708,#14300,.T.);
#21121=EDGE_CURVE('',#16707,#16706,#14301,.T.);
#21122=EDGE_CURVE('',#16709,#16705,#636,.T.);
#21123=EDGE_CURVE('',#16710,#16709,#14302,.T.);
#21124=EDGE_CURVE('',#16711,#16710,#14303,.T.);
#21125=EDGE_CURVE('',#16706,#16711,#637,.T.);
#21126=EDGE_CURVE('',#16712,#16712,#14304,.T.);
#21127=EDGE_CURVE('',#16712,#16710,#14305,.T.);
#21128=EDGE_CURVE('',#16711,#16709,#638,.T.);
#21129=EDGE_CURVE('',#16713,#16714,#639,.T.);
#21130=EDGE_CURVE('',#16713,#16715,#14306,.T.);
#21131=EDGE_CURVE('',#16715,#16716,#14307,.T.);
#21132=EDGE_CURVE('',#16716,#16716,#14308,.T.);
#21133=EDGE_CURVE('',#16715,#16714,#14309,.T.);
#21134=EDGE_CURVE('',#16717,#16713,#640,.T.);
#21135=EDGE_CURVE('',#16718,#16717,#14310,.T.);
#21136=EDGE_CURVE('',#16719,#16718,#14311,.T.);
#21137=EDGE_CURVE('',#16714,#16719,#641,.T.);
#21138=EDGE_CURVE('',#16720,#16720,#14312,.T.);
#21139=EDGE_CURVE('',#16720,#16718,#14313,.T.);
#21140=EDGE_CURVE('',#16719,#16717,#642,.T.);
#21141=EDGE_CURVE('',#16721,#16722,#643,.T.);
#21142=EDGE_CURVE('',#16721,#16723,#14314,.T.);
#21143=EDGE_CURVE('',#16723,#16724,#14315,.T.);
#21144=EDGE_CURVE('',#16724,#16724,#14316,.T.);
#21145=EDGE_CURVE('',#16723,#16722,#14317,.T.);
#21146=EDGE_CURVE('',#16725,#16721,#644,.T.);
#21147=EDGE_CURVE('',#16726,#16725,#14318,.T.);
#21148=EDGE_CURVE('',#16727,#16726,#14319,.T.);
#21149=EDGE_CURVE('',#16722,#16727,#645,.T.);
#21150=EDGE_CURVE('',#16728,#16728,#14320,.T.);
#21151=EDGE_CURVE('',#16728,#16726,#14321,.T.);
#21152=EDGE_CURVE('',#16727,#16725,#646,.T.);
#21153=EDGE_CURVE('',#16729,#16730,#647,.T.);
#21154=EDGE_CURVE('',#16729,#16731,#14322,.T.);
#21155=EDGE_CURVE('',#16731,#16732,#14323,.T.);
#21156=EDGE_CURVE('',#16732,#16732,#14324,.T.);
#21157=EDGE_CURVE('',#16731,#16730,#14325,.T.);
#21158=EDGE_CURVE('',#16733,#16729,#648,.T.);
#21159=EDGE_CURVE('',#16734,#16733,#14326,.T.);
#21160=EDGE_CURVE('',#16735,#16734,#14327,.T.);
#21161=EDGE_CURVE('',#16730,#16735,#649,.T.);
#21162=EDGE_CURVE('',#16736,#16736,#14328,.T.);
#21163=EDGE_CURVE('',#16736,#16734,#14329,.T.);
#21164=EDGE_CURVE('',#16735,#16733,#650,.T.);
#21165=EDGE_CURVE('',#16737,#16738,#651,.T.);
#21166=EDGE_CURVE('',#16737,#16739,#14330,.T.);
#21167=EDGE_CURVE('',#16739,#16740,#14331,.T.);
#21168=EDGE_CURVE('',#16740,#16740,#14332,.T.);
#21169=EDGE_CURVE('',#16739,#16738,#14333,.T.);
#21170=EDGE_CURVE('',#16741,#16737,#652,.T.);
#21171=EDGE_CURVE('',#16742,#16741,#14334,.T.);
#21172=EDGE_CURVE('',#16743,#16742,#14335,.T.);
#21173=EDGE_CURVE('',#16738,#16743,#653,.T.);
#21174=EDGE_CURVE('',#16744,#16744,#14336,.T.);
#21175=EDGE_CURVE('',#16744,#16742,#14337,.T.);
#21176=EDGE_CURVE('',#16743,#16741,#654,.T.);
#21177=EDGE_CURVE('',#16581,#16745,#9956,.T.);
#21178=EDGE_CURVE('',#16745,#16745,#14338,.T.);
#21179=EDGE_CURVE('',#16576,#16664,#9957,.T.);
#21180=EDGE_CURVE('',#16656,#16582,#9958,.T.);
#21181=EDGE_CURVE('',#16746,#16746,#14339,.T.);
#21182=EDGE_CURVE('',#16746,#16577,#9959,.T.);
#21183=EDGE_CURVE('',#16747,#16747,#14340,.T.);
#21184=EDGE_CURVE('',#16747,#16748,#9960,.T.);
#21185=EDGE_CURVE('',#16748,#16748,#14341,.T.);
#21186=EDGE_CURVE('',#16748,#16749,#9961,.T.);
#21187=EDGE_CURVE('',#16749,#16749,#14342,.T.);
#21188=EDGE_CURVE('',#16749,#16750,#9962,.T.);
#21189=EDGE_CURVE('',#16750,#16750,#14343,.T.);
#21190=EDGE_CURVE('',#16751,#16752,#9963,.T.);
#21191=EDGE_CURVE('',#16752,#16753,#9964,.T.);
#21192=EDGE_CURVE('',#16753,#16754,#9965,.T.);
#21193=EDGE_CURVE('',#16754,#16751,#9966,.T.);
#21194=EDGE_CURVE('',#16755,#16751,#9967,.T.);
#21195=EDGE_CURVE('',#16756,#16755,#9968,.T.);
#21196=EDGE_CURVE('',#16756,#16757,#9969,.T.);
#21197=EDGE_CURVE('',#16758,#16757,#9970,.T.);
#21198=EDGE_CURVE('',#16752,#16758,#9971,.T.);
#21199=EDGE_CURVE('',#16759,#16754,#9972,.T.);
#21200=EDGE_CURVE('',#16755,#16759,#9973,.T.);
#21201=EDGE_CURVE('',#16759,#16760,#9974,.T.);
#21202=EDGE_CURVE('',#16760,#16756,#9975,.T.);
#21203=EDGE_CURVE('',#16761,#16753,#9976,.T.);
#21204=EDGE_CURVE('',#16762,#16761,#9977,.T.);
#21205=EDGE_CURVE('',#16762,#16760,#9978,.T.);
#21206=EDGE_CURVE('',#16763,#16763,#14344,.T.);
#21207=EDGE_CURVE('',#16761,#16758,#14345,.T.);
#21208=EDGE_CURVE('',#16762,#16757,#14346,.T.);
#21209=EDGE_CURVE('',#16764,#16764,#14347,.T.);
#21210=EDGE_CURVE('',#16765,#16765,#14348,.T.);
#21211=EDGE_CURVE('',#16765,#16764,#9979,.T.);
#21212=EDGE_CURVE('',#16766,#16766,#14349,.T.);
#21213=EDGE_CURVE('',#16766,#16765,#9980,.T.);
#21214=EDGE_CURVE('',#16763,#16766,#9981,.T.);
#21215=EDGE_CURVE('',#16767,#16768,#183,.T.);
#21216=EDGE_CURVE('',#16768,#16769,#9982,.T.);
#21217=EDGE_CURVE('',#16769,#16770,#184,.T.);
#21218=EDGE_CURVE('',#16770,#16771,#9983,.T.);
#21219=EDGE_CURVE('',#16771,#16767,#9984,.T.);
#21220=EDGE_CURVE('',#16768,#16772,#14350,.T.);
#21221=EDGE_CURVE('',#16773,#16772,#9985,.T.);
#21222=EDGE_CURVE('',#16769,#16773,#14351,.T.);
#21223=EDGE_CURVE('',#16767,#16774,#185,.T.);
#21224=EDGE_CURVE('',#16775,#16774,#186,.T.);
#21225=EDGE_CURVE('',#16776,#16775,#187,.T.);
#21226=EDGE_CURVE('',#16777,#16776,#188,.T.);
#21227=EDGE_CURVE('',#16777,#16778,#189,.T.);
#21228=EDGE_CURVE('',#16772,#16778,#190,.T.);
#21229=EDGE_CURVE('',#16779,#16771,#9986,.T.);
#21230=EDGE_CURVE('',#16780,#16779,#191,.T.);
#21231=EDGE_CURVE('',#16780,#16781,#9987,.T.);
#21232=EDGE_CURVE('',#16782,#16781,#9988,.F.);
#21233=EDGE_CURVE('',#16774,#16782,#9989,.T.);
#21234=EDGE_CURVE('',#16782,#16783,#9990,.F.);
#21235=EDGE_CURVE('',#16783,#16775,#9991,.T.);
#21236=EDGE_CURVE('',#16784,#16777,#9992,.T.);
#21237=EDGE_CURVE('',#16776,#16785,#9993,.T.);
#21238=EDGE_CURVE('',#16785,#16784,#9994,.T.);
#21239=EDGE_CURVE('',#16785,#16786,#9995,.T.);
#21240=EDGE_CURVE('',#16786,#16787,#9996,.T.);
#21241=EDGE_CURVE('',#16787,#16788,#9997,.T.);
#21242=EDGE_CURVE('',#16788,#16789,#9998,.T.);
#21243=EDGE_CURVE('',#16789,#16784,#9999,.T.);
#21244=EDGE_CURVE('',#16789,#16790,#10000,.T.);
#21245=EDGE_CURVE('',#16791,#16790,#192,.T.);
#21246=EDGE_CURVE('',#16792,#16791,#10001,.T.);
#21247=EDGE_CURVE('',#16778,#16792,#10002,.T.);
#21248=EDGE_CURVE('',#16793,#16788,#10003,.T.);
#21249=EDGE_CURVE('',#16794,#16793,#10004,.T.);
#21250=EDGE_CURVE('',#16790,#16794,#14352,.T.);
#21251=EDGE_CURVE('',#16787,#16795,#10005,.T.);
#21252=EDGE_CURVE('',#16795,#16796,#10006,.T.);
#21253=EDGE_CURVE('',#16797,#16796,#10007,.T.);
#21254=EDGE_CURVE('',#16797,#16793,#10008,.T.);
#21255=EDGE_CURVE('',#16798,#16773,#193,.T.);
#21256=EDGE_CURVE('',#16792,#16798,#10009,.T.);
#21257=EDGE_CURVE('',#16798,#16799,#655,.T.);
#21258=EDGE_CURVE('',#16799,#16800,#14353,.T.);
#21259=EDGE_CURVE('',#16770,#16800,#656,.T.);
#21260=EDGE_CURVE('',#16801,#16802,#10010,.T.);
#21261=EDGE_CURVE('',#16802,#16803,#10011,.T.);
#21262=EDGE_CURVE('',#16803,#16804,#194,.T.);
#21263=EDGE_CURVE('',#16804,#16805,#10012,.T.);
#21264=EDGE_CURVE('',#16805,#16801,#10013,.T.);
#21265=EDGE_CURVE('',#16806,#16802,#10014,.T.);
#21266=EDGE_CURVE('',#16807,#16806,#10015,.T.);
#21267=EDGE_CURVE('',#16807,#16808,#195,.T.);
#21268=EDGE_CURVE('',#16809,#16808,#10016,.T.);
#21269=EDGE_CURVE('',#16810,#16809,#10017,.T.);
#21270=EDGE_CURVE('',#16811,#16810,#10018,.T.);
#21271=EDGE_CURVE('',#16811,#16803,#196,.T.);
#21272=EDGE_CURVE('',#16812,#16801,#10019,.T.);
#21273=EDGE_CURVE('',#16812,#16813,#10020,.T.);
#21274=EDGE_CURVE('',#16813,#16814,#10021,.T.);
#21275=EDGE_CURVE('',#16806,#16814,#10022,.T.);
#21276=EDGE_CURVE('',#16805,#16783,#10023,.T.);
#21277=EDGE_CURVE('',#16781,#16812,#10024,.T.);
#21278=EDGE_CURVE('',#16815,#16816,#197,.T.);
#21279=EDGE_CURVE('',#16816,#16817,#10025,.T.);
#21280=EDGE_CURVE('',#16817,#16818,#198,.T.);
#21281=EDGE_CURVE('',#16818,#16819,#10026,.T.);
#21282=EDGE_CURVE('',#16819,#16815,#10027,.T.);
#21283=EDGE_CURVE('',#16817,#16820,#14354,.T.);
#21284=EDGE_CURVE('',#16821,#16820,#199,.T.);
#21285=EDGE_CURVE('',#16821,#16822,#657,.T.);
#21286=EDGE_CURVE('',#16822,#16823,#14355,.T.);
#21287=EDGE_CURVE('',#16823,#16818,#658,.T.);
#21288=EDGE_CURVE('',#16816,#16824,#14356,.T.);
#21289=EDGE_CURVE('',#16820,#16824,#10028,.T.);
#21290=EDGE_CURVE('',#16815,#16825,#200,.T.);
#21291=EDGE_CURVE('',#16826,#16825,#201,.T.);
#21292=EDGE_CURVE('',#16827,#16826,#202,.T.);
#21293=EDGE_CURVE('',#16828,#16827,#203,.T.);
#21294=EDGE_CURVE('',#16828,#16829,#204,.T.);
#21295=EDGE_CURVE('',#16824,#16829,#205,.T.);
#21296=EDGE_CURVE('',#16796,#16826,#10029,.T.);
#21297=EDGE_CURVE('',#16825,#16797,#10030,.T.);
#21298=EDGE_CURVE('',#16786,#16830,#10031,.T.);
#21299=EDGE_CURVE('',#16830,#16831,#206,.T.);
#21300=EDGE_CURVE('',#16831,#16795,#10032,.T.);
#21301=EDGE_CURVE('',#16831,#16832,#207,.T.);
#21302=EDGE_CURVE('',#16833,#16832,#10033,.T.);
#21303=EDGE_CURVE('',#16834,#16833,#10034,.T.);
#21304=EDGE_CURVE('',#16827,#16834,#10035,.T.);
#21305=EDGE_CURVE('',#16835,#16835,#14357,.T.);
#21306=EDGE_CURVE('',#16835,#16836,#10036,.T.);
#21307=EDGE_CURVE('',#16804,#16836,#208,.T.);
#21308=EDGE_CURVE('',#16837,#16811,#209,.T.);
#21309=EDGE_CURVE('',#16838,#16837,#210,.T.);
#21310=EDGE_CURVE('',#16839,#16838,#211,.T.);
#21311=EDGE_CURVE('',#16840,#16839,#212,.T.);
#21312=EDGE_CURVE('',#16841,#16840,#213,.T.);
#21313=EDGE_CURVE('',#16842,#16841,#214,.T.);
#21314=EDGE_CURVE('',#16832,#16842,#215,.T.);
#21315=EDGE_CURVE('',#16836,#16830,#216,.T.);
#21316=EDGE_CURVE('',#16843,#16844,#217,.T.);
#21317=EDGE_CURVE('',#16844,#16845,#10037,.T.);
#21318=EDGE_CURVE('',#16845,#16846,#218,.T.);
#21319=EDGE_CURVE('',#16846,#16847,#10038,.T.);
#21320=EDGE_CURVE('',#16847,#16843,#10039,.T.);
#21321=EDGE_CURVE('',#16844,#16848,#14358,.T.);
#21322=EDGE_CURVE('',#16849,#16848,#10040,.T.);
#21323=EDGE_CURVE('',#16845,#16849,#14359,.T.);
#21324=EDGE_CURVE('',#16843,#16850,#219,.T.);
#21325=EDGE_CURVE('',#16851,#16850,#220,.T.);
#21326=EDGE_CURVE('',#16852,#16851,#221,.T.);
#21327=EDGE_CURVE('',#16853,#16852,#222,.T.);
#21328=EDGE_CURVE('',#16853,#16854,#223,.T.);
#21329=EDGE_CURVE('',#16848,#16854,#224,.T.);
#21330=EDGE_CURVE('',#16855,#16847,#10041,.T.);
#21331=EDGE_CURVE('',#16856,#16855,#225,.T.);
#21332=EDGE_CURVE('',#16856,#16857,#10042,.T.);
#21333=EDGE_CURVE('',#16858,#16857,#10043,.T.);
#21334=EDGE_CURVE('',#16850,#16858,#10044,.T.);
#21335=EDGE_CURVE('',#16859,#16851,#10045,.T.);
#21336=EDGE_CURVE('',#16858,#16859,#10046,.T.);
#21337=EDGE_CURVE('',#16860,#16833,#10047,.T.);
#21338=EDGE_CURVE('',#16861,#16860,#10048,.T.);
#21339=EDGE_CURVE('',#16833,#16861,#10049,.T.);
#21340=EDGE_CURVE('',#16857,#16861,#10050,.T.);
#21341=EDGE_CURVE('',#16860,#16859,#10051,.T.);
#21342=EDGE_CURVE('',#16862,#16828,#10052,.T.);
#21343=EDGE_CURVE('',#16834,#16862,#10053,.T.);
#21344=EDGE_CURVE('',#16861,#16863,#10054,.T.);
#21345=EDGE_CURVE('',#16863,#16862,#10055,.T.);
#21346=EDGE_CURVE('',#16842,#16860,#10056,.T.);
#21347=EDGE_CURVE('',#16864,#16841,#10057,.T.);
#21348=EDGE_CURVE('',#16865,#16864,#10058,.T.);
#21349=EDGE_CURVE('',#16852,#16865,#10059,.T.);
#21350=EDGE_CURVE('',#16829,#16866,#10060,.T.);
#21351=EDGE_CURVE('',#16866,#16821,#10061,.T.);
#21352=EDGE_CURVE('',#16867,#16853,#10062,.T.);
#21353=EDGE_CURVE('',#16865,#16867,#10063,.T.);
#21354=EDGE_CURVE('',#16864,#16868,#10064,.T.);
#21355=EDGE_CURVE('',#16868,#16869,#10065,.T.);
#21356=EDGE_CURVE('',#16869,#16870,#10066,.T.);
#21357=EDGE_CURVE('',#16870,#16867,#10067,.T.);
#21358=EDGE_CURVE('',#16870,#16871,#10068,.T.);
#21359=EDGE_CURVE('',#16872,#16871,#226,.T.);
#21360=EDGE_CURVE('',#16873,#16872,#10069,.T.);
#21361=EDGE_CURVE('',#16854,#16873,#10070,.T.);
#21362=EDGE_CURVE('',#16874,#16869,#10071,.T.);
#21363=EDGE_CURVE('',#16875,#16874,#10072,.T.);
#21364=EDGE_CURVE('',#16871,#16875,#14360,.T.);
#21365=EDGE_CURVE('',#16868,#16876,#10073,.T.);
#21366=EDGE_CURVE('',#16876,#16877,#10074,.T.);
#21367=EDGE_CURVE('',#16878,#16877,#10075,.T.);
#21368=EDGE_CURVE('',#16878,#16874,#10076,.T.);
#21369=EDGE_CURVE('',#16879,#16849,#227,.T.);
#21370=EDGE_CURVE('',#16873,#16879,#10077,.T.);
#21371=EDGE_CURVE('',#16879,#16880,#659,.T.);
#21372=EDGE_CURVE('',#16880,#16881,#14361,.T.);
#21373=EDGE_CURVE('',#16846,#16881,#660,.T.);
#21374=EDGE_CURVE('',#16882,#16810,#10078,.T.);
#21375=EDGE_CURVE('',#16809,#16883,#10079,.F.);
#21376=EDGE_CURVE('',#16883,#16884,#10080,.F.);
#21377=EDGE_CURVE('',#16884,#16885,#10081,.T.);
#21378=EDGE_CURVE('',#16885,#16882,#10082,.T.);
#21379=EDGE_CURVE('',#16882,#16886,#10083,.T.);
#21380=EDGE_CURVE('',#16886,#16837,#10084,.T.);
#21381=EDGE_CURVE('',#16814,#16887,#10085,.T.);
#21382=EDGE_CURVE('',#16887,#16807,#228,.T.);
#21383=EDGE_CURVE('',#16887,#16888,#229,.T.);
#21384=EDGE_CURVE('',#16889,#16888,#230,.T.);
#21385=EDGE_CURVE('',#16890,#16889,#14362,.T.);
#21386=EDGE_CURVE('',#16891,#16890,#231,.T.);
#21387=EDGE_CURVE('',#16891,#16892,#232,.T.);
#21388=EDGE_CURVE('',#16808,#16892,#233,.T.);
#21389=EDGE_CURVE('',#16813,#16893,#10086,.T.);
#21390=EDGE_CURVE('',#16894,#16893,#234,.T.);
#21391=EDGE_CURVE('',#16895,#16894,#10087,.T.);
#21392=EDGE_CURVE('',#16888,#16895,#10088,.T.);
#21393=EDGE_CURVE('',#16893,#16780,#14363,.T.);
#21394=EDGE_CURVE('',#16896,#16886,#10089,.T.);
#21395=EDGE_CURVE('',#16897,#16896,#10090,.T.);
#21396=EDGE_CURVE('',#16897,#16898,#235,.T.);
#21397=EDGE_CURVE('',#16899,#16898,#10091,.T.);
#21398=EDGE_CURVE('',#16900,#16899,#10092,.T.);
#21399=EDGE_CURVE('',#16838,#16900,#10093,.T.);
#21400=EDGE_CURVE('',#16885,#16901,#10094,.T.);
#21401=EDGE_CURVE('',#16901,#16902,#10095,.F.);
#21402=EDGE_CURVE('',#16896,#16902,#10096,.F.);
#21403=EDGE_CURVE('',#16903,#16897,#236,.T.);
#21404=EDGE_CURVE('',#16902,#16903,#10097,.T.);
#21405=EDGE_CURVE('',#16901,#16904,#10098,.T.);
#21406=EDGE_CURVE('',#16905,#16904,#237,.T.);
#21407=EDGE_CURVE('',#16906,#16905,#10099,.T.);
#21408=EDGE_CURVE('',#16907,#16906,#10100,.T.);
#21409=EDGE_CURVE('',#16903,#16907,#238,.T.);
#21410=EDGE_CURVE('',#16892,#16883,#10101,.T.);
#21411=EDGE_CURVE('',#16908,#16891,#10102,.T.);
#21412=EDGE_CURVE('',#16909,#16908,#10103,.T.);
#21413=EDGE_CURVE('',#16910,#16909,#239,.T.);
#21414=EDGE_CURVE('',#16910,#16884,#10104,.T.);
#21415=EDGE_CURVE('',#16890,#16911,#10105,.T.);
#21416=EDGE_CURVE('',#16911,#16912,#240,.T.);
#21417=EDGE_CURVE('',#16912,#16908,#10106,.T.);
#21418=EDGE_CURVE('',#16911,#16913,#14364,.T.);
#21419=EDGE_CURVE('',#16913,#16914,#241,.F.);
#21420=EDGE_CURVE('',#16914,#16915,#14365,.T.);
#21421=EDGE_CURVE('',#16915,#16912,#242,.T.);
#21422=EDGE_CURVE('',#16913,#16889,#10107,.T.);
#21423=EDGE_CURVE('',#16914,#16895,#10108,.T.);
#21424=EDGE_CURVE('',#16895,#16913,#10109,.T.);
#21425=EDGE_CURVE('',#16916,#16914,#10110,.T.);
#21426=EDGE_CURVE('',#16894,#16916,#661,.T.);
#21427=EDGE_CURVE('',#16800,#16917,#10111,.T.);
#21428=EDGE_CURVE('',#16917,#16779,#662,.T.);
#21429=EDGE_CURVE('',#16791,#16918,#663,.T.);
#21430=EDGE_CURVE('',#16918,#16799,#10112,.T.);
#21431=EDGE_CURVE('',#16866,#16919,#10113,.T.);
#21432=EDGE_CURVE('',#16919,#16920,#664,.T.);
#21433=EDGE_CURVE('',#16920,#16822,#10114,.T.);
#21434=EDGE_CURVE('',#16881,#16921,#10115,.T.);
#21435=EDGE_CURVE('',#16921,#16855,#665,.T.);
#21436=EDGE_CURVE('',#16872,#16922,#666,.T.);
#21437=EDGE_CURVE('',#16922,#16880,#10116,.T.);
#21438=EDGE_CURVE('',#16923,#16924,#10117,.T.);
#21439=EDGE_CURVE('',#16924,#16925,#10118,.T.);
#21440=EDGE_CURVE('',#16925,#16926,#243,.T.);
#21441=EDGE_CURVE('',#16926,#16927,#10119,.T.);
#21442=EDGE_CURVE('',#16927,#16923,#667,.T.);
#21443=EDGE_CURVE('',#16875,#16923,#244,.T.);
#21444=EDGE_CURVE('',#16927,#16922,#14366,.T.);
#21445=EDGE_CURVE('',#16928,#16856,#14367,.T.);
#21446=EDGE_CURVE('',#16921,#16920,#14368,.T.);
#21447=EDGE_CURVE('',#16919,#16928,#245,.T.);
#21448=EDGE_CURVE('',#16823,#16929,#10120,.T.);
#21449=EDGE_CURVE('',#16929,#16930,#668,.T.);
#21450=EDGE_CURVE('',#16930,#16819,#10121,.T.);
#21451=EDGE_CURVE('',#16794,#16930,#246,.T.);
#21452=EDGE_CURVE('',#16929,#16918,#14369,.T.);
#21453=EDGE_CURVE('',#16917,#16916,#14370,.T.);
#21454=EDGE_CURVE('',#16915,#16931,#10122,.T.);
#21455=EDGE_CURVE('',#16931,#16909,#669,.T.);
#21456=EDGE_CURVE('',#16932,#16926,#14371,.T.);
#21457=EDGE_CURVE('',#16933,#16932,#10123,.T.);
#21458=EDGE_CURVE('',#16934,#16933,#14372,.T.);
#21459=EDGE_CURVE('',#16935,#16934,#10124,.T.);
#21460=EDGE_CURVE('',#16936,#16935,#14373,.T.);
#21461=EDGE_CURVE('',#16937,#16936,#10125,.T.);
#21462=EDGE_CURVE('',#16938,#16937,#14374,.T.);
#21463=EDGE_CURVE('',#16938,#16939,#10126,.T.);
#21464=EDGE_CURVE('',#16939,#16940,#14375,.T.);
#21465=EDGE_CURVE('',#16940,#16939,#14376,.T.);
#21466=EDGE_CURVE('',#16931,#16938,#14377,.T.);
#21467=EDGE_CURVE('',#16941,#16925,#670,.T.);
#21468=EDGE_CURVE('',#16941,#16942,#14378,.T.);
#21469=EDGE_CURVE('',#16942,#16932,#247,.F.);
#21470=EDGE_CURVE('',#16924,#16943,#10127,.T.);
#21471=EDGE_CURVE('',#16943,#16944,#248,.T.);
#21472=EDGE_CURVE('',#16944,#16941,#10128,.T.);
#21473=EDGE_CURVE('',#16877,#16945,#10129,.T.);
#21474=EDGE_CURVE('',#16945,#16946,#249,.T.);
#21475=EDGE_CURVE('',#16946,#16878,#10130,.T.);
#21476=EDGE_CURVE('',#16840,#16876,#10131,.T.);
#21477=EDGE_CURVE('',#16947,#16945,#250,.T.);
#21478=EDGE_CURVE('',#16948,#16947,#251,.T.);
#21479=EDGE_CURVE('',#16948,#16949,#252,.T.);
#21480=EDGE_CURVE('',#16950,#16949,#253,.T.);
#21481=EDGE_CURVE('',#16944,#16950,#14379,.T.);
#21482=EDGE_CURVE('',#16943,#16946,#254,.T.);
#21483=EDGE_CURVE('',#16951,#16839,#10132,.T.);
#21484=EDGE_CURVE('',#16952,#16951,#10133,.T.);
#21485=EDGE_CURVE('',#16947,#16952,#10134,.T.);
#21486=EDGE_CURVE('',#16936,#16906,#10135,.T.);
#21487=EDGE_CURVE('',#16953,#16936,#255,.F.);
#21488=EDGE_CURVE('',#16906,#16953,#10136,.T.);
#21489=EDGE_CURVE('',#16935,#16954,#256,.F.);
#21490=EDGE_CURVE('',#16955,#16935,#10137,.T.);
#21491=EDGE_CURVE('',#16954,#16955,#10138,.T.);
#21492=EDGE_CURVE('',#16956,#16955,#10139,.T.);
#21493=EDGE_CURVE('',#16934,#16956,#671,.T.);
#21494=EDGE_CURVE('',#16932,#16957,#10140,.T.);
#21495=EDGE_CURVE('',#16957,#16942,#10141,.T.);
#21496=EDGE_CURVE('',#16949,#16957,#10142,.T.);
#21497=EDGE_CURVE('',#16942,#16950,#10143,.T.);
#21498=EDGE_CURVE('',#16957,#16958,#10144,.T.);
#21499=EDGE_CURVE('',#16958,#16933,#672,.T.);
#21500=EDGE_CURVE('',#16958,#16959,#257,.T.);
#21501=EDGE_CURVE('',#16959,#16960,#14380,.T.);
#21502=EDGE_CURVE('',#16960,#16956,#258,.T.);
#21503=EDGE_CURVE('',#16961,#16962,#259,.T.);
#21504=EDGE_CURVE('',#16962,#16954,#10145,.T.);
#21505=EDGE_CURVE('',#16955,#16961,#10146,.T.);
#21506=EDGE_CURVE('',#16954,#16953,#14381,.T.);
#21507=EDGE_CURVE('',#16963,#16907,#260,.T.);
#21508=EDGE_CURVE('',#16953,#16963,#10147,.T.);
#21509=EDGE_CURVE('',#16905,#16937,#673,.T.);
#21510=EDGE_CURVE('',#16904,#16910,#14382,.T.);
#21511=EDGE_CURVE('',#16898,#16964,#261,.T.);
#21512=EDGE_CURVE('',#16964,#16965,#10148,.T.);
#21513=EDGE_CURVE('',#16965,#16899,#10149,.T.);
#21514=EDGE_CURVE('',#16900,#16951,#10150,.T.);
#21515=EDGE_CURVE('',#16966,#16900,#10151,.T.);
#21516=EDGE_CURVE('',#16951,#16966,#10152,.T.);
#21517=EDGE_CURVE('',#16967,#16966,#10153,.T.);
#21518=EDGE_CURVE('',#16965,#16967,#10154,.T.);
#21519=EDGE_CURVE('',#16968,#16948,#10155,.T.);
#21520=EDGE_CURVE('',#16952,#16968,#10156,.T.);
#21521=EDGE_CURVE('',#16966,#16969,#10157,.T.);
#21522=EDGE_CURVE('',#16969,#16968,#10158,.T.);
#21523=EDGE_CURVE('',#16962,#16963,#14383,.T.);
#21524=EDGE_CURVE('',#16961,#16964,#262,.T.);
#21525=EDGE_CURVE('',#16970,#16970,#14384,.T.);
#21526=EDGE_CURVE('',#16970,#16940,#10159,.T.);
#21527=EDGE_CURVE('',#16969,#16959,#10160,.T.);
#21528=EDGE_CURVE('',#16960,#16967,#10161,.T.);
#21529=EDGE_CURVE('',#16863,#16928,#10162,.T.);
#21530=EDGE_CURVE('',#16971,#16972,#674,.F.);
#21531=EDGE_CURVE('',#16972,#16973,#14385,.T.);
#21532=EDGE_CURVE('',#16973,#16974,#14386,.T.);
#21533=EDGE_CURVE('',#16974,#16975,#675,.F.);
#21534=EDGE_CURVE('',#16975,#16971,#14387,.T.);
#21535=EDGE_CURVE('',#16972,#16974,#676,.T.);
#21536=EDGE_CURVE('',#16973,#16976,#10163,.T.);
#21537=EDGE_CURVE('',#16976,#16977,#14388,.T.);
#21538=EDGE_CURVE('',#16978,#16977,#10164,.T.);
#21539=EDGE_CURVE('',#16979,#16978,#14389,.T.);
#21540=EDGE_CURVE('',#16980,#16979,#10165,.T.);
#21541=EDGE_CURVE('',#16980,#16981,#14390,.T.);
#21542=EDGE_CURVE('',#16982,#16981,#10166,.T.);
#21543=EDGE_CURVE('',#16983,#16982,#14391,.T.);
#21544=EDGE_CURVE('',#16984,#16983,#10167,.T.);
#21545=EDGE_CURVE('',#16984,#16976,#14392,.T.);
#21546=EDGE_CURVE('',#16985,#16978,#263,.T.);
#21547=EDGE_CURVE('',#16977,#16986,#10168,.F.);
#21548=EDGE_CURVE('',#16986,#16987,#10169,.T.);
#21549=EDGE_CURVE('',#16987,#16985,#10170,.T.);
#21550=EDGE_CURVE('',#16985,#16988,#677,.T.);
#21551=EDGE_CURVE('',#16988,#16989,#14393,.T.);
#21552=EDGE_CURVE('',#16990,#16989,#678,.T.);
#21553=EDGE_CURVE('',#16979,#16990,#264,.T.);
#21554=EDGE_CURVE('',#16987,#16991,#10171,.T.);
#21555=EDGE_CURVE('',#16990,#16991,#10172,.T.);
#21556=EDGE_CURVE('',#16989,#16988,#10173,.T.);
#21557=EDGE_CURVE('',#16986,#16992,#10174,.T.);
#21558=EDGE_CURVE('',#16991,#16992,#10175,.T.);
#21559=EDGE_CURVE('',#16993,#16994,#10176,.T.);
#21560=EDGE_CURVE('',#16994,#16995,#10177,.T.);
#21561=EDGE_CURVE('',#16995,#16984,#10178,.F.);
#21562=EDGE_CURVE('',#16983,#16993,#265,.T.);
#21563=EDGE_CURVE('',#16996,#16994,#10179,.T.);
#21564=EDGE_CURVE('',#16997,#16996,#10180,.T.);
#21565=EDGE_CURVE('',#16997,#16995,#10181,.T.);
#21566=EDGE_CURVE('',#16998,#16993,#679,.T.);
#21567=EDGE_CURVE('',#16998,#16999,#10182,.T.);
#21568=EDGE_CURVE('',#17000,#16999,#680,.T.);
#21569=EDGE_CURVE('',#16996,#17000,#10183,.T.);
#21570=EDGE_CURVE('',#17000,#16982,#266,.T.);
#21571=EDGE_CURVE('',#16981,#16997,#10184,.F.);
#21572=EDGE_CURVE('',#16992,#16980,#10185,.F.);
#21573=EDGE_CURVE('',#16999,#16998,#14394,.T.);
#21574=EDGE_CURVE('',#17001,#17001,#14395,.T.);
#21575=EDGE_CURVE('',#17001,#17001,#14396,.T.);
#21576=EDGE_CURVE('',#16975,#16971,#681,.T.);
#21577=EDGE_CURVE('',#17002,#17003,#14397,.T.);
#21578=EDGE_CURVE('',#17003,#17002,#14398,.T.);
#21579=EDGE_CURVE('',#17002,#17004,#10186,.T.);
#21580=EDGE_CURVE('',#17004,#17005,#14399,.T.);
#21581=EDGE_CURVE('',#17005,#17004,#14400,.T.);
#21582=EDGE_CURVE('',#17005,#17006,#10187,.T.);
#21583=EDGE_CURVE('',#17007,#17006,#14401,.T.);
#21584=EDGE_CURVE('',#17006,#17007,#14402,.T.);
#21585=EDGE_CURVE('',#17008,#17008,#14403,.T.);
#21586=EDGE_CURVE('',#17008,#17003,#10188,.T.);
#21587=EDGE_CURVE('',#17007,#17009,#10189,.T.);
#21588=EDGE_CURVE('',#17009,#17010,#14404,.T.);
#21589=EDGE_CURVE('',#17010,#17009,#14405,.T.);
#21590=EDGE_CURVE('',#17010,#17011,#10190,.T.);
#21591=EDGE_CURVE('',#17012,#17011,#14406,.T.);
#21592=EDGE_CURVE('',#17011,#17012,#14407,.T.);
#21593=EDGE_CURVE('',#17012,#17013,#10191,.T.);
#21594=EDGE_CURVE('',#17013,#17014,#14408,.T.);
#21595=EDGE_CURVE('',#17014,#17013,#14409,.T.);
#21596=EDGE_CURVE('',#17014,#17015,#10192,.T.);
#21597=EDGE_CURVE('',#17016,#17015,#14410,.T.);
#21598=EDGE_CURVE('',#17015,#17016,#14411,.T.);
#21599=EDGE_CURVE('',#17016,#17017,#10193,.T.);
#21600=EDGE_CURVE('',#17017,#17018,#14412,.T.);
#21601=EDGE_CURVE('',#17018,#17017,#14413,.T.);
#21602=EDGE_CURVE('',#17018,#17019,#10194,.T.);
#21603=EDGE_CURVE('',#17019,#17019,#14414,.T.);
#21604=EDGE_CURVE('',#17020,#17020,#14415,.T.);
#21605=EDGE_CURVE('',#17021,#17021,#14416,.T.);
#21606=EDGE_CURVE('',#17022,#17022,#14417,.T.);
#21607=EDGE_CURVE('',#17022,#17020,#10195,.T.);
#21608=EDGE_CURVE('',#17023,#17023,#14418,.T.);
#21609=EDGE_CURVE('',#17023,#17022,#10196,.T.);
#21610=EDGE_CURVE('',#17024,#17024,#14419,.T.);
#21611=EDGE_CURVE('',#17025,#17025,#14420,.T.);
#21612=EDGE_CURVE('',#17025,#17024,#10197,.T.);
#21613=EDGE_CURVE('',#17019,#17025,#10198,.T.);
#21614=EDGE_CURVE('',#17026,#17026,#14421,.T.);
#21615=EDGE_CURVE('',#17026,#17027,#10199,.T.);
#21616=EDGE_CURVE('',#17027,#17027,#14422,.T.);
#21617=EDGE_CURVE('',#17027,#17028,#10200,.T.);
#21618=EDGE_CURVE('',#17028,#17028,#14423,.T.);
#21619=EDGE_CURVE('',#17028,#17029,#10201,.T.);
#21620=EDGE_CURVE('',#17029,#17029,#14424,.T.);
#21621=EDGE_CURVE('',#17029,#17030,#10202,.T.);
#21622=EDGE_CURVE('',#17030,#17030,#14425,.T.);
#21623=EDGE_CURVE('',#17030,#17031,#10203,.T.);
#21624=EDGE_CURVE('',#17031,#17031,#14426,.T.);
#21625=EDGE_CURVE('',#17031,#17021,#10204,.T.);
#21626=EDGE_CURVE('',#17032,#17033,#10205,.T.);
#21627=EDGE_CURVE('',#17032,#17034,#682,.T.);
#21628=EDGE_CURVE('',#17034,#17035,#14427,.F.);
#21629=EDGE_CURVE('',#17035,#17033,#683,.T.);
#21630=EDGE_CURVE('',#17036,#17037,#10206,.T.);
#21631=EDGE_CURVE('',#17036,#17032,#684,.T.);
#21632=EDGE_CURVE('',#17033,#17037,#685,.T.);
#21633=EDGE_CURVE('',#17038,#17039,#10207,.T.);
#21634=EDGE_CURVE('',#17038,#17036,#686,.T.);
#21635=EDGE_CURVE('',#17037,#17039,#687,.T.);
#21636=EDGE_CURVE('',#17040,#17041,#10208,.T.);
#21637=EDGE_CURVE('',#17040,#17038,#688,.T.);
#21638=EDGE_CURVE('',#17039,#17041,#689,.T.);
#21639=EDGE_CURVE('',#17042,#17043,#10209,.T.);
#21640=EDGE_CURVE('',#17042,#17040,#690,.T.);
#21641=EDGE_CURVE('',#17041,#17043,#691,.T.);
#21642=EDGE_CURVE('',#17044,#17045,#10210,.T.);
#21643=EDGE_CURVE('',#17044,#17042,#692,.T.);
#21644=EDGE_CURVE('',#17043,#17045,#693,.T.);
#21645=EDGE_CURVE('',#17046,#17047,#10211,.T.);
#21646=EDGE_CURVE('',#17046,#17044,#694,.T.);
#21647=EDGE_CURVE('',#17045,#17047,#695,.T.);
#21648=EDGE_CURVE('',#17048,#17049,#10212,.T.);
#21649=EDGE_CURVE('',#17048,#17046,#696,.T.);
#21650=EDGE_CURVE('',#17047,#17049,#697,.T.);
#21651=EDGE_CURVE('',#17050,#17051,#10213,.T.);
#21652=EDGE_CURVE('',#17050,#17048,#698,.T.);
#21653=EDGE_CURVE('',#17049,#17051,#699,.T.);
#21654=EDGE_CURVE('',#17052,#17053,#10214,.T.);
#21655=EDGE_CURVE('',#17052,#17050,#700,.T.);
#21656=EDGE_CURVE('',#17051,#17053,#701,.T.);
#21657=EDGE_CURVE('',#17054,#17055,#10215,.T.);
#21658=EDGE_CURVE('',#17054,#17052,#702,.T.);
#21659=EDGE_CURVE('',#17053,#17055,#703,.T.);
#21660=EDGE_CURVE('',#17056,#17057,#10216,.T.);
#21661=EDGE_CURVE('',#17056,#17054,#704,.T.);
#21662=EDGE_CURVE('',#17055,#17057,#705,.T.);
#21663=EDGE_CURVE('',#17058,#17059,#10217,.T.);
#21664=EDGE_CURVE('',#17058,#17056,#706,.T.);
#21665=EDGE_CURVE('',#17057,#17059,#707,.T.);
#21666=EDGE_CURVE('',#17060,#17061,#10218,.T.);
#21667=EDGE_CURVE('',#17060,#17058,#708,.T.);
#21668=EDGE_CURVE('',#17059,#17061,#709,.T.);
#21669=EDGE_CURVE('',#17062,#17063,#10219,.T.);
#21670=EDGE_CURVE('',#17062,#17060,#710,.T.);
#21671=EDGE_CURVE('',#17061,#17063,#711,.T.);
#21672=EDGE_CURVE('',#17064,#17065,#10220,.T.);
#21673=EDGE_CURVE('',#17064,#17062,#712,.T.);
#21674=EDGE_CURVE('',#17063,#17065,#713,.T.);
#21675=EDGE_CURVE('',#17066,#17067,#10221,.T.);
#21676=EDGE_CURVE('',#17066,#17064,#714,.T.);
#21677=EDGE_CURVE('',#17065,#17067,#715,.T.);
#21678=EDGE_CURVE('',#17068,#17069,#10222,.T.);
#21679=EDGE_CURVE('',#17068,#17066,#716,.T.);
#21680=EDGE_CURVE('',#17067,#17069,#717,.T.);
#21681=EDGE_CURVE('',#17070,#17071,#10223,.T.);
#21682=EDGE_CURVE('',#17070,#17068,#718,.T.);
#21683=EDGE_CURVE('',#17069,#17071,#719,.T.);
#21684=EDGE_CURVE('',#17072,#17073,#10224,.T.);
#21685=EDGE_CURVE('',#17072,#17070,#720,.T.);
#21686=EDGE_CURVE('',#17071,#17073,#721,.T.);
#21687=EDGE_CURVE('',#17074,#17075,#10225,.T.);
#21688=EDGE_CURVE('',#17074,#17072,#722,.T.);
#21689=EDGE_CURVE('',#17073,#17075,#723,.T.);
#21690=EDGE_CURVE('',#17076,#17077,#10226,.T.);
#21691=EDGE_CURVE('',#17076,#17074,#724,.T.);
#21692=EDGE_CURVE('',#17075,#17077,#725,.T.);
#21693=EDGE_CURVE('',#17078,#17079,#10227,.T.);
#21694=EDGE_CURVE('',#17078,#17076,#726,.T.);
#21695=EDGE_CURVE('',#17077,#17079,#727,.T.);
#21696=EDGE_CURVE('',#17080,#17081,#10228,.T.);
#21697=EDGE_CURVE('',#17080,#17078,#728,.T.);
#21698=EDGE_CURVE('',#17079,#17081,#729,.T.);
#21699=EDGE_CURVE('',#17082,#17083,#10229,.T.);
#21700=EDGE_CURVE('',#17082,#17080,#730,.T.);
#21701=EDGE_CURVE('',#17081,#17083,#731,.T.);
#21702=EDGE_CURVE('',#17084,#17085,#10230,.T.);
#21703=EDGE_CURVE('',#17084,#17082,#732,.T.);
#21704=EDGE_CURVE('',#17083,#17085,#733,.T.);
#21705=EDGE_CURVE('',#17086,#17087,#10231,.T.);
#21706=EDGE_CURVE('',#17086,#17084,#734,.T.);
#21707=EDGE_CURVE('',#17085,#17087,#735,.T.);
#21708=EDGE_CURVE('',#17088,#17089,#10232,.T.);
#21709=EDGE_CURVE('',#17088,#17086,#736,.T.);
#21710=EDGE_CURVE('',#17087,#17089,#737,.T.);
#21711=EDGE_CURVE('',#17090,#17091,#10233,.T.);
#21712=EDGE_CURVE('',#17090,#17088,#738,.T.);
#21713=EDGE_CURVE('',#17089,#17091,#739,.T.);
#21714=EDGE_CURVE('',#17092,#17093,#10234,.T.);
#21715=EDGE_CURVE('',#17092,#17094,#740,.T.);
#21716=EDGE_CURVE('',#17093,#17094,#14428,.T.);
#21717=EDGE_CURVE('',#17095,#17096,#10235,.T.);
#21718=EDGE_CURVE('',#17095,#17092,#741,.T.);
#21719=EDGE_CURVE('',#17097,#17093,#14429,.T.);
#21720=EDGE_CURVE('',#17096,#17097,#742,.T.);
#21721=EDGE_CURVE('',#17098,#17099,#10236,.T.);
#21722=EDGE_CURVE('',#17098,#17095,#743,.T.);
#21723=EDGE_CURVE('',#17099,#17096,#744,.T.);
#21724=EDGE_CURVE('',#17100,#17101,#10237,.T.);
#21725=EDGE_CURVE('',#17100,#17098,#745,.T.);
#21726=EDGE_CURVE('',#17101,#17099,#746,.T.);
#21727=EDGE_CURVE('',#17102,#17103,#10238,.T.);
#21728=EDGE_CURVE('',#17102,#17100,#747,.T.);
#21729=EDGE_CURVE('',#17103,#17101,#748,.T.);
#21730=EDGE_CURVE('',#17104,#17105,#10239,.T.);
#21731=EDGE_CURVE('',#17104,#17102,#749,.T.);
#21732=EDGE_CURVE('',#17105,#17103,#750,.T.);
#21733=EDGE_CURVE('',#17106,#17107,#10240,.T.);
#21734=EDGE_CURVE('',#17106,#17104,#751,.T.);
#21735=EDGE_CURVE('',#17107,#17105,#752,.T.);
#21736=EDGE_CURVE('',#17108,#17109,#10241,.T.);
#21737=EDGE_CURVE('',#17108,#17106,#753,.T.);
#21738=EDGE_CURVE('',#17109,#17107,#754,.T.);
#21739=EDGE_CURVE('',#17110,#17111,#10242,.T.);
#21740=EDGE_CURVE('',#17110,#17108,#755,.T.);
#21741=EDGE_CURVE('',#17111,#17109,#756,.T.);
#21742=EDGE_CURVE('',#17112,#17113,#10243,.T.);
#21743=EDGE_CURVE('',#17112,#17110,#757,.T.);
#21744=EDGE_CURVE('',#17113,#17111,#758,.T.);
#21745=EDGE_CURVE('',#17114,#17115,#10244,.T.);
#21746=EDGE_CURVE('',#17114,#17112,#759,.T.);
#21747=EDGE_CURVE('',#17115,#17113,#760,.T.);
#21748=EDGE_CURVE('',#17116,#17117,#10245,.T.);
#21749=EDGE_CURVE('',#17116,#17114,#761,.T.);
#21750=EDGE_CURVE('',#17117,#17115,#762,.T.);
#21751=EDGE_CURVE('',#17118,#17119,#10246,.T.);
#21752=EDGE_CURVE('',#17118,#17116,#763,.T.);
#21753=EDGE_CURVE('',#17119,#17117,#764,.T.);
#21754=EDGE_CURVE('',#17120,#17121,#10247,.T.);
#21755=EDGE_CURVE('',#17120,#17118,#765,.T.);
#21756=EDGE_CURVE('',#17121,#17119,#766,.T.);
#21757=EDGE_CURVE('',#17122,#17123,#10248,.T.);
#21758=EDGE_CURVE('',#17122,#17120,#767,.T.);
#21759=EDGE_CURVE('',#17123,#17121,#768,.T.);
#21760=EDGE_CURVE('',#17124,#17125,#10249,.T.);
#21761=EDGE_CURVE('',#17124,#17122,#769,.T.);
#21762=EDGE_CURVE('',#17125,#17123,#770,.T.);
#21763=EDGE_CURVE('',#17126,#17127,#10250,.T.);
#21764=EDGE_CURVE('',#17126,#17124,#771,.T.);
#21765=EDGE_CURVE('',#17127,#17125,#772,.T.);
#21766=EDGE_CURVE('',#17128,#17129,#10251,.T.);
#21767=EDGE_CURVE('',#17128,#17126,#773,.T.);
#21768=EDGE_CURVE('',#17129,#17127,#774,.T.);
#21769=EDGE_CURVE('',#17130,#17131,#10252,.T.);
#21770=EDGE_CURVE('',#17130,#17128,#775,.T.);
#21771=EDGE_CURVE('',#17131,#17129,#776,.T.);
#21772=EDGE_CURVE('',#17132,#17133,#10253,.T.);
#21773=EDGE_CURVE('',#17132,#17130,#777,.T.);
#21774=EDGE_CURVE('',#17133,#17131,#778,.T.);
#21775=EDGE_CURVE('',#17134,#17135,#10254,.T.);
#21776=EDGE_CURVE('',#17134,#17132,#779,.T.);
#21777=EDGE_CURVE('',#17135,#17133,#780,.T.);
#21778=EDGE_CURVE('',#17136,#17137,#10255,.T.);
#21779=EDGE_CURVE('',#17136,#17134,#781,.T.);
#21780=EDGE_CURVE('',#17137,#17135,#782,.T.);
#21781=EDGE_CURVE('',#17138,#17139,#10256,.T.);
#21782=EDGE_CURVE('',#17138,#17136,#783,.T.);
#21783=EDGE_CURVE('',#17139,#17137,#784,.T.);
#21784=EDGE_CURVE('',#17140,#17141,#10257,.T.);
#21785=EDGE_CURVE('',#17140,#17138,#785,.T.);
#21786=EDGE_CURVE('',#17141,#17139,#786,.T.);
#21787=EDGE_CURVE('',#17142,#17143,#10258,.T.);
#21788=EDGE_CURVE('',#17142,#17140,#787,.T.);
#21789=EDGE_CURVE('',#17143,#17141,#788,.T.);
#21790=EDGE_CURVE('',#17144,#17145,#10259,.T.);
#21791=EDGE_CURVE('',#17144,#17142,#789,.T.);
#21792=EDGE_CURVE('',#17145,#17143,#790,.T.);
#21793=EDGE_CURVE('',#17146,#17147,#10260,.T.);
#21794=EDGE_CURVE('',#17146,#17144,#791,.T.);
#21795=EDGE_CURVE('',#17147,#17145,#792,.T.);
#21796=EDGE_CURVE('',#17148,#17149,#10261,.T.);
#21797=EDGE_CURVE('',#17148,#17146,#793,.T.);
#21798=EDGE_CURVE('',#17149,#17147,#794,.T.);
#21799=EDGE_CURVE('',#17150,#17151,#10262,.T.);
#21800=EDGE_CURVE('',#17150,#17148,#795,.T.);
#21801=EDGE_CURVE('',#17151,#17149,#796,.T.);
#21802=EDGE_CURVE('',#17152,#17152,#14430,.T.);
#21803=EDGE_CURVE('',#17152,#17153,#10263,.T.);
#21804=EDGE_CURVE('',#17153,#17154,#14431,.T.);
#21805=EDGE_CURVE('',#17154,#17153,#14432,.T.);
#21806=EDGE_CURVE('',#17154,#17155,#10264,.T.);
#21807=EDGE_CURVE('',#17155,#17156,#14433,.F.);
#21808=EDGE_CURVE('',#17156,#17157,#14434,.F.);
#21809=EDGE_CURVE('',#17157,#17155,#14435,.F.);
#21810=EDGE_CURVE('',#17158,#17159,#267,.T.);
#21811=EDGE_CURVE('',#17159,#17160,#10265,.T.);
#21812=EDGE_CURVE('',#17160,#17161,#268,.T.);
#21813=EDGE_CURVE('',#17161,#17162,#10266,.T.);
#21814=EDGE_CURVE('',#17162,#17163,#10267,.T.);
#21815=EDGE_CURVE('',#17163,#17158,#10268,.T.);
#21816=EDGE_CURVE('',#17159,#17160,#14436,.T.);
#21817=EDGE_CURVE('',#17164,#17164,#14437,.T.);
#21818=EDGE_CURVE('',#17163,#17165,#10269,.T.);
#21819=EDGE_CURVE('',#17165,#17166,#10270,.T.);
#21820=EDGE_CURVE('',#17166,#17167,#269,.T.);
#21821=EDGE_CURVE('',#17167,#17168,#10271,.T.);
#21822=EDGE_CURVE('',#17168,#17158,#270,.T.);
#21823=EDGE_CURVE('',#17167,#17169,#14438,.T.);
#21824=EDGE_CURVE('',#17170,#17169,#10272,.T.);
#21825=EDGE_CURVE('',#17168,#17170,#14439,.T.);
#21826=EDGE_CURVE('',#17171,#17166,#271,.T.);
#21827=EDGE_CURVE('',#17171,#17172,#14440,.T.);
#21828=EDGE_CURVE('',#17173,#17172,#272,.T.);
#21829=EDGE_CURVE('',#17169,#17173,#273,.T.);
#21830=EDGE_CURVE('',#17165,#17174,#10273,.T.);
#21831=EDGE_CURVE('',#17174,#17173,#10274,.T.);
#21832=EDGE_CURVE('',#17172,#17171,#10275,.T.);
#21833=EDGE_CURVE('',#17174,#17162,#10276,.T.);
#21834=EDGE_CURVE('',#17161,#17170,#274,.T.);
#21835=EDGE_CURVE('',#17094,#17156,#797,.T.);
#21836=EDGE_CURVE('',#17157,#17097,#798,.T.);
#21837=EDGE_CURVE('',#17091,#17157,#799,.T.);
#21838=EDGE_CURVE('',#17175,#17035,#800,.T.);
#21839=EDGE_CURVE('',#17175,#17151,#801,.T.);
#21840=EDGE_CURVE('',#17035,#17176,#14441,.F.);
#21841=EDGE_CURVE('',#17176,#17034,#14442,.F.);
#21842=EDGE_CURVE('',#17034,#17177,#802,.T.);
#21843=EDGE_CURVE('',#17177,#17175,#14443,.T.);
#21844=EDGE_CURVE('',#17177,#17150,#803,.T.);
#21845=EDGE_CURVE('',#17156,#17090,#804,.T.);
#21846=EDGE_CURVE('',#17178,#17179,#10277,.T.);
#21847=EDGE_CURVE('',#17178,#17180,#10278,.T.);
#21848=EDGE_CURVE('',#17181,#17180,#10279,.T.);
#21849=EDGE_CURVE('',#17179,#17181,#10280,.T.);
#21850=EDGE_CURVE('',#17179,#17182,#14444,.T.);
#21851=EDGE_CURVE('',#17181,#17182,#10281,.T.);
#21852=EDGE_CURVE('',#17182,#17183,#10282,.T.);
#21853=EDGE_CURVE('',#17180,#17183,#10283,.T.);
#21854=EDGE_CURVE('',#17183,#17178,#14445,.T.);
#21855=EDGE_CURVE('',#17184,#17185,#10284,.T.);
#21856=EDGE_CURVE('',#17184,#17186,#10285,.T.);
#21857=EDGE_CURVE('',#17187,#17186,#10286,.T.);
#21858=EDGE_CURVE('',#17185,#17187,#10287,.T.);
#21859=EDGE_CURVE('',#17185,#17188,#14446,.T.);
#21860=EDGE_CURVE('',#17187,#17188,#10288,.T.);
#21861=EDGE_CURVE('',#17188,#17189,#10289,.T.);
#21862=EDGE_CURVE('',#17186,#17189,#10290,.T.);
#21863=EDGE_CURVE('',#17189,#17184,#14447,.T.);
#21864=EDGE_CURVE('',#17190,#17191,#10291,.T.);
#21865=EDGE_CURVE('',#17190,#17192,#10292,.T.);
#21866=EDGE_CURVE('',#17193,#17192,#10293,.T.);
#21867=EDGE_CURVE('',#17191,#17193,#10294,.T.);
#21868=EDGE_CURVE('',#17191,#17194,#14448,.T.);
#21869=EDGE_CURVE('',#17193,#17194,#10295,.T.);
#21870=EDGE_CURVE('',#17194,#17195,#10296,.T.);
#21871=EDGE_CURVE('',#17192,#17195,#10297,.T.);
#21872=EDGE_CURVE('',#17195,#17190,#14449,.T.);
#21873=EDGE_CURVE('',#17196,#17197,#10298,.T.);
#21874=EDGE_CURVE('',#17196,#17198,#10299,.T.);
#21875=EDGE_CURVE('',#17199,#17198,#10300,.T.);
#21876=EDGE_CURVE('',#17197,#17199,#10301,.T.);
#21877=EDGE_CURVE('',#17197,#17200,#14450,.T.);
#21878=EDGE_CURVE('',#17199,#17200,#10302,.T.);
#21879=EDGE_CURVE('',#17200,#17201,#10303,.T.);
#21880=EDGE_CURVE('',#17198,#17201,#10304,.T.);
#21881=EDGE_CURVE('',#17201,#17196,#14451,.T.);
#21882=EDGE_CURVE('',#17202,#17203,#10305,.T.);
#21883=EDGE_CURVE('',#17202,#17204,#10306,.T.);
#21884=EDGE_CURVE('',#17205,#17204,#10307,.T.);
#21885=EDGE_CURVE('',#17203,#17205,#10308,.T.);
#21886=EDGE_CURVE('',#17203,#17206,#14452,.T.);
#21887=EDGE_CURVE('',#17205,#17206,#10309,.T.);
#21888=EDGE_CURVE('',#17206,#17207,#10310,.T.);
#21889=EDGE_CURVE('',#17204,#17207,#10311,.T.);
#21890=EDGE_CURVE('',#17207,#17202,#14453,.T.);
#21891=EDGE_CURVE('',#17208,#17209,#10312,.T.);
#21892=EDGE_CURVE('',#17208,#17210,#10313,.T.);
#21893=EDGE_CURVE('',#17211,#17210,#10314,.T.);
#21894=EDGE_CURVE('',#17209,#17211,#10315,.T.);
#21895=EDGE_CURVE('',#17209,#17212,#14454,.T.);
#21896=EDGE_CURVE('',#17211,#17212,#10316,.T.);
#21897=EDGE_CURVE('',#17212,#17213,#10317,.T.);
#21898=EDGE_CURVE('',#17210,#17213,#10318,.T.);
#21899=EDGE_CURVE('',#17213,#17208,#14455,.T.);
#21900=EDGE_CURVE('',#17214,#17215,#10319,.T.);
#21901=EDGE_CURVE('',#17214,#17216,#10320,.T.);
#21902=EDGE_CURVE('',#17217,#17216,#10321,.T.);
#21903=EDGE_CURVE('',#17215,#17217,#10322,.T.);
#21904=EDGE_CURVE('',#17215,#17218,#14456,.T.);
#21905=EDGE_CURVE('',#17217,#17218,#10323,.T.);
#21906=EDGE_CURVE('',#17218,#17219,#10324,.T.);
#21907=EDGE_CURVE('',#17216,#17219,#10325,.T.);
#21908=EDGE_CURVE('',#17219,#17214,#14457,.T.);
#21909=EDGE_CURVE('',#17220,#17221,#10326,.T.);
#21910=EDGE_CURVE('',#17220,#17222,#10327,.T.);
#21911=EDGE_CURVE('',#17223,#17222,#10328,.T.);
#21912=EDGE_CURVE('',#17221,#17223,#10329,.T.);
#21913=EDGE_CURVE('',#17221,#17224,#14458,.T.);
#21914=EDGE_CURVE('',#17223,#17224,#10330,.T.);
#21915=EDGE_CURVE('',#17224,#17225,#10331,.T.);
#21916=EDGE_CURVE('',#17222,#17225,#10332,.T.);
#21917=EDGE_CURVE('',#17225,#17220,#14459,.T.);
#21918=EDGE_CURVE('',#17226,#17227,#10333,.T.);
#21919=EDGE_CURVE('',#17226,#17228,#10334,.T.);
#21920=EDGE_CURVE('',#17229,#17228,#10335,.T.);
#21921=EDGE_CURVE('',#17227,#17229,#10336,.T.);
#21922=EDGE_CURVE('',#17227,#17230,#14460,.T.);
#21923=EDGE_CURVE('',#17229,#17230,#10337,.T.);
#21924=EDGE_CURVE('',#17230,#17231,#10338,.T.);
#21925=EDGE_CURVE('',#17228,#17231,#10339,.T.);
#21926=EDGE_CURVE('',#17231,#17226,#14461,.T.);
#21927=EDGE_CURVE('',#17232,#17233,#10340,.T.);
#21928=EDGE_CURVE('',#17232,#17234,#10341,.T.);
#21929=EDGE_CURVE('',#17235,#17234,#10342,.T.);
#21930=EDGE_CURVE('',#17233,#17235,#10343,.T.);
#21931=EDGE_CURVE('',#17233,#17236,#14462,.T.);
#21932=EDGE_CURVE('',#17235,#17236,#10344,.T.);
#21933=EDGE_CURVE('',#17236,#17237,#10345,.T.);
#21934=EDGE_CURVE('',#17234,#17237,#10346,.T.);
#21935=EDGE_CURVE('',#17237,#17232,#14463,.T.);
#21936=EDGE_CURVE('',#17238,#17239,#10347,.T.);
#21937=EDGE_CURVE('',#17238,#17240,#10348,.T.);
#21938=EDGE_CURVE('',#17241,#17240,#10349,.T.);
#21939=EDGE_CURVE('',#17239,#17241,#10350,.T.);
#21940=EDGE_CURVE('',#17239,#17242,#14464,.T.);
#21941=EDGE_CURVE('',#17241,#17242,#10351,.T.);
#21942=EDGE_CURVE('',#17242,#17243,#10352,.T.);
#21943=EDGE_CURVE('',#17240,#17243,#10353,.T.);
#21944=EDGE_CURVE('',#17243,#17238,#14465,.T.);
#21945=EDGE_CURVE('',#17244,#17245,#10354,.T.);
#21946=EDGE_CURVE('',#17244,#17246,#10355,.T.);
#21947=EDGE_CURVE('',#17247,#17246,#10356,.T.);
#21948=EDGE_CURVE('',#17245,#17247,#10357,.T.);
#21949=EDGE_CURVE('',#17245,#17248,#14466,.T.);
#21950=EDGE_CURVE('',#17247,#17248,#10358,.T.);
#21951=EDGE_CURVE('',#17248,#17249,#10359,.T.);
#21952=EDGE_CURVE('',#17246,#17249,#10360,.T.);
#21953=EDGE_CURVE('',#17249,#17244,#14467,.T.);
#21954=EDGE_CURVE('',#17250,#17251,#10361,.T.);
#21955=EDGE_CURVE('',#17250,#17252,#10362,.T.);
#21956=EDGE_CURVE('',#17253,#17252,#10363,.T.);
#21957=EDGE_CURVE('',#17251,#17253,#10364,.T.);
#21958=EDGE_CURVE('',#17251,#17254,#14468,.T.);
#21959=EDGE_CURVE('',#17253,#17254,#10365,.T.);
#21960=EDGE_CURVE('',#17254,#17255,#10366,.T.);
#21961=EDGE_CURVE('',#17252,#17255,#10367,.T.);
#21962=EDGE_CURVE('',#17255,#17250,#14469,.T.);
#21963=EDGE_CURVE('',#17256,#17257,#10368,.T.);
#21964=EDGE_CURVE('',#17256,#17258,#10369,.T.);
#21965=EDGE_CURVE('',#17259,#17258,#10370,.T.);
#21966=EDGE_CURVE('',#17257,#17259,#10371,.T.);
#21967=EDGE_CURVE('',#17257,#17260,#14470,.T.);
#21968=EDGE_CURVE('',#17259,#17260,#10372,.T.);
#21969=EDGE_CURVE('',#17260,#17261,#10373,.T.);
#21970=EDGE_CURVE('',#17258,#17261,#10374,.T.);
#21971=EDGE_CURVE('',#17261,#17256,#14471,.T.);
#21972=EDGE_CURVE('',#17262,#17263,#10375,.T.);
#21973=EDGE_CURVE('',#17262,#17264,#10376,.T.);
#21974=EDGE_CURVE('',#17265,#17264,#10377,.T.);
#21975=EDGE_CURVE('',#17263,#17265,#10378,.T.);
#21976=EDGE_CURVE('',#17263,#17266,#14472,.T.);
#21977=EDGE_CURVE('',#17265,#17266,#10379,.T.);
#21978=EDGE_CURVE('',#17266,#17267,#10380,.T.);
#21979=EDGE_CURVE('',#17264,#17267,#10381,.T.);
#21980=EDGE_CURVE('',#17267,#17262,#14473,.T.);
#21981=EDGE_CURVE('',#17268,#17269,#10382,.T.);
#21982=EDGE_CURVE('',#17268,#17270,#10383,.T.);
#21983=EDGE_CURVE('',#17271,#17270,#10384,.T.);
#21984=EDGE_CURVE('',#17269,#17271,#10385,.T.);
#21985=EDGE_CURVE('',#17269,#17272,#14474,.T.);
#21986=EDGE_CURVE('',#17271,#17272,#10386,.T.);
#21987=EDGE_CURVE('',#17272,#17273,#10387,.T.);
#21988=EDGE_CURVE('',#17270,#17273,#10388,.T.);
#21989=EDGE_CURVE('',#17273,#17268,#14475,.T.);
#21990=EDGE_CURVE('',#17274,#17275,#10389,.T.);
#21991=EDGE_CURVE('',#17274,#17276,#10390,.T.);
#21992=EDGE_CURVE('',#17277,#17276,#10391,.T.);
#21993=EDGE_CURVE('',#17275,#17277,#10392,.T.);
#21994=EDGE_CURVE('',#17275,#17278,#14476,.T.);
#21995=EDGE_CURVE('',#17277,#17278,#10393,.T.);
#21996=EDGE_CURVE('',#17278,#17279,#10394,.T.);
#21997=EDGE_CURVE('',#17276,#17279,#10395,.T.);
#21998=EDGE_CURVE('',#17279,#17274,#14477,.T.);
#21999=EDGE_CURVE('',#17280,#17281,#10396,.T.);
#22000=EDGE_CURVE('',#17280,#17282,#10397,.T.);
#22001=EDGE_CURVE('',#17283,#17282,#10398,.T.);
#22002=EDGE_CURVE('',#17281,#17283,#10399,.T.);
#22003=EDGE_CURVE('',#17281,#17284,#14478,.T.);
#22004=EDGE_CURVE('',#17283,#17285,#10400,.T.);
#22005=EDGE_CURVE('',#17284,#17285,#14479,.T.);
#22006=EDGE_CURVE('',#17285,#17286,#10401,.T.);
#22007=EDGE_CURVE('',#17282,#17286,#10402,.T.);
#22008=EDGE_CURVE('',#17286,#17287,#14480,.T.);
#22009=EDGE_CURVE('',#17287,#17280,#14481,.T.);
#22010=EDGE_CURVE('',#17288,#17289,#10403,.T.);
#22011=EDGE_CURVE('',#17288,#17290,#10404,.T.);
#22012=EDGE_CURVE('',#17291,#17290,#10405,.T.);
#22013=EDGE_CURVE('',#17289,#17291,#10406,.T.);
#22014=EDGE_CURVE('',#17289,#17292,#14482,.T.);
#22015=EDGE_CURVE('',#17291,#17292,#10407,.T.);
#22016=EDGE_CURVE('',#17292,#17293,#10408,.T.);
#22017=EDGE_CURVE('',#17290,#17293,#10409,.T.);
#22018=EDGE_CURVE('',#17293,#17288,#14483,.T.);
#22019=EDGE_CURVE('',#17294,#17295,#10410,.T.);
#22020=EDGE_CURVE('',#17294,#17296,#10411,.T.);
#22021=EDGE_CURVE('',#17297,#17296,#10412,.T.);
#22022=EDGE_CURVE('',#17295,#17297,#10413,.T.);
#22023=EDGE_CURVE('',#17295,#17298,#14484,.T.);
#22024=EDGE_CURVE('',#17297,#17298,#10414,.T.);
#22025=EDGE_CURVE('',#17298,#17299,#10415,.T.);
#22026=EDGE_CURVE('',#17296,#17299,#10416,.T.);
#22027=EDGE_CURVE('',#17299,#17294,#14485,.T.);
#22028=EDGE_CURVE('',#17300,#17301,#10417,.T.);
#22029=EDGE_CURVE('',#17300,#17302,#10418,.T.);
#22030=EDGE_CURVE('',#17303,#17302,#10419,.T.);
#22031=EDGE_CURVE('',#17301,#17303,#10420,.T.);
#22032=EDGE_CURVE('',#17301,#17304,#14486,.T.);
#22033=EDGE_CURVE('',#17303,#17304,#10421,.T.);
#22034=EDGE_CURVE('',#17304,#17305,#10422,.T.);
#22035=EDGE_CURVE('',#17302,#17305,#10423,.T.);
#22036=EDGE_CURVE('',#17305,#17300,#14487,.T.);
#22037=EDGE_CURVE('',#17306,#17307,#10424,.T.);
#22038=EDGE_CURVE('',#17306,#17308,#10425,.T.);
#22039=EDGE_CURVE('',#17309,#17308,#10426,.T.);
#22040=EDGE_CURVE('',#17307,#17309,#10427,.T.);
#22041=EDGE_CURVE('',#17307,#17310,#14488,.T.);
#22042=EDGE_CURVE('',#17309,#17310,#10428,.T.);
#22043=EDGE_CURVE('',#17310,#17311,#10429,.T.);
#22044=EDGE_CURVE('',#17308,#17311,#10430,.T.);
#22045=EDGE_CURVE('',#17311,#17306,#14489,.T.);
#22046=EDGE_CURVE('',#17312,#17313,#10431,.T.);
#22047=EDGE_CURVE('',#17312,#17314,#10432,.T.);
#22048=EDGE_CURVE('',#17315,#17314,#10433,.T.);
#22049=EDGE_CURVE('',#17313,#17315,#10434,.T.);
#22050=EDGE_CURVE('',#17313,#17316,#14490,.T.);
#22051=EDGE_CURVE('',#17315,#17316,#10435,.T.);
#22052=EDGE_CURVE('',#17316,#17317,#10436,.T.);
#22053=EDGE_CURVE('',#17314,#17317,#10437,.T.);
#22054=EDGE_CURVE('',#17317,#17312,#14491,.T.);
#22055=EDGE_CURVE('',#17318,#17319,#10438,.T.);
#22056=EDGE_CURVE('',#17318,#17320,#10439,.T.);
#22057=EDGE_CURVE('',#17321,#17320,#10440,.T.);
#22058=EDGE_CURVE('',#17319,#17321,#10441,.T.);
#22059=EDGE_CURVE('',#17319,#17322,#14492,.T.);
#22060=EDGE_CURVE('',#17321,#17322,#10442,.T.);
#22061=EDGE_CURVE('',#17322,#17323,#10443,.T.);
#22062=EDGE_CURVE('',#17320,#17323,#10444,.T.);
#22063=EDGE_CURVE('',#17323,#17318,#14493,.T.);
#22064=EDGE_CURVE('',#17324,#17325,#10445,.T.);
#22065=EDGE_CURVE('',#17324,#17326,#10446,.T.);
#22066=EDGE_CURVE('',#17327,#17326,#10447,.T.);
#22067=EDGE_CURVE('',#17325,#17327,#10448,.T.);
#22068=EDGE_CURVE('',#17325,#17328,#14494,.T.);
#22069=EDGE_CURVE('',#17327,#17328,#10449,.T.);
#22070=EDGE_CURVE('',#17328,#17329,#10450,.T.);
#22071=EDGE_CURVE('',#17326,#17329,#10451,.T.);
#22072=EDGE_CURVE('',#17329,#17324,#14495,.T.);
#22073=EDGE_CURVE('',#17330,#17331,#10452,.T.);
#22074=EDGE_CURVE('',#17330,#17332,#10453,.T.);
#22075=EDGE_CURVE('',#17333,#17332,#10454,.T.);
#22076=EDGE_CURVE('',#17331,#17333,#10455,.T.);
#22077=EDGE_CURVE('',#17331,#17334,#14496,.T.);
#22078=EDGE_CURVE('',#17333,#17334,#10456,.T.);
#22079=EDGE_CURVE('',#17334,#17335,#10457,.T.);
#22080=EDGE_CURVE('',#17332,#17335,#10458,.T.);
#22081=EDGE_CURVE('',#17335,#17330,#14497,.T.);
#22082=EDGE_CURVE('',#17336,#17337,#10459,.T.);
#22083=EDGE_CURVE('',#17336,#17338,#10460,.T.);
#22084=EDGE_CURVE('',#17339,#17338,#10461,.T.);
#22085=EDGE_CURVE('',#17337,#17339,#10462,.T.);
#22086=EDGE_CURVE('',#17337,#17340,#14498,.T.);
#22087=EDGE_CURVE('',#17339,#17340,#10463,.T.);
#22088=EDGE_CURVE('',#17340,#17341,#10464,.T.);
#22089=EDGE_CURVE('',#17338,#17341,#10465,.T.);
#22090=EDGE_CURVE('',#17341,#17336,#14499,.T.);
#22091=EDGE_CURVE('',#17342,#17343,#10466,.T.);
#22092=EDGE_CURVE('',#17342,#17344,#10467,.T.);
#22093=EDGE_CURVE('',#17345,#17344,#10468,.T.);
#22094=EDGE_CURVE('',#17343,#17345,#10469,.T.);
#22095=EDGE_CURVE('',#17343,#17346,#14500,.T.);
#22096=EDGE_CURVE('',#17345,#17346,#10470,.T.);
#22097=EDGE_CURVE('',#17346,#17347,#10471,.T.);
#22098=EDGE_CURVE('',#17344,#17347,#10472,.T.);
#22099=EDGE_CURVE('',#17347,#17342,#14501,.T.);
#22100=EDGE_CURVE('',#17348,#17349,#10473,.T.);
#22101=EDGE_CURVE('',#17348,#17350,#10474,.T.);
#22102=EDGE_CURVE('',#17351,#17350,#10475,.T.);
#22103=EDGE_CURVE('',#17349,#17351,#10476,.T.);
#22104=EDGE_CURVE('',#17349,#17352,#14502,.T.);
#22105=EDGE_CURVE('',#17351,#17352,#10477,.T.);
#22106=EDGE_CURVE('',#17352,#17353,#10478,.T.);
#22107=EDGE_CURVE('',#17350,#17353,#10479,.T.);
#22108=EDGE_CURVE('',#17353,#17348,#14503,.T.);
#22109=EDGE_CURVE('',#17354,#17355,#10480,.T.);
#22110=EDGE_CURVE('',#17354,#17356,#10481,.T.);
#22111=EDGE_CURVE('',#17357,#17356,#10482,.T.);
#22112=EDGE_CURVE('',#17355,#17357,#10483,.T.);
#22113=EDGE_CURVE('',#17355,#17358,#14504,.T.);
#22114=EDGE_CURVE('',#17357,#17358,#10484,.T.);
#22115=EDGE_CURVE('',#17358,#17359,#10485,.T.);
#22116=EDGE_CURVE('',#17356,#17359,#10486,.T.);
#22117=EDGE_CURVE('',#17359,#17354,#14505,.T.);
#22118=EDGE_CURVE('',#17360,#17361,#10487,.T.);
#22119=EDGE_CURVE('',#17360,#17362,#10488,.T.);
#22120=EDGE_CURVE('',#17363,#17362,#10489,.T.);
#22121=EDGE_CURVE('',#17361,#17363,#10490,.T.);
#22122=EDGE_CURVE('',#17361,#17364,#14506,.T.);
#22123=EDGE_CURVE('',#17363,#17364,#10491,.T.);
#22124=EDGE_CURVE('',#17364,#17365,#10492,.T.);
#22125=EDGE_CURVE('',#17362,#17365,#10493,.T.);
#22126=EDGE_CURVE('',#17365,#17360,#14507,.T.);
#22127=EDGE_CURVE('',#17366,#17367,#10494,.T.);
#22128=EDGE_CURVE('',#17366,#17368,#10495,.T.);
#22129=EDGE_CURVE('',#17369,#17368,#10496,.T.);
#22130=EDGE_CURVE('',#17367,#17369,#10497,.T.);
#22131=EDGE_CURVE('',#17367,#17370,#14508,.T.);
#22132=EDGE_CURVE('',#17369,#17370,#10498,.T.);
#22133=EDGE_CURVE('',#17370,#17371,#10499,.T.);
#22134=EDGE_CURVE('',#17368,#17371,#10500,.T.);
#22135=EDGE_CURVE('',#17371,#17366,#14509,.T.);
#22136=EDGE_CURVE('',#17372,#17373,#10501,.T.);
#22137=EDGE_CURVE('',#17372,#17374,#10502,.T.);
#22138=EDGE_CURVE('',#17375,#17374,#10503,.T.);
#22139=EDGE_CURVE('',#17373,#17375,#10504,.T.);
#22140=EDGE_CURVE('',#17373,#17376,#14510,.T.);
#22141=EDGE_CURVE('',#17375,#17376,#10505,.T.);
#22142=EDGE_CURVE('',#17376,#17377,#10506,.T.);
#22143=EDGE_CURVE('',#17374,#17377,#10507,.T.);
#22144=EDGE_CURVE('',#17377,#17372,#14511,.T.);
#22145=EDGE_CURVE('',#17378,#17379,#10508,.T.);
#22146=EDGE_CURVE('',#17378,#17380,#10509,.T.);
#22147=EDGE_CURVE('',#17381,#17380,#10510,.T.);
#22148=EDGE_CURVE('',#17379,#17381,#10511,.T.);
#22149=EDGE_CURVE('',#17379,#17382,#14512,.T.);
#22150=EDGE_CURVE('',#17381,#17382,#10512,.T.);
#22151=EDGE_CURVE('',#17382,#17383,#10513,.T.);
#22152=EDGE_CURVE('',#17380,#17383,#10514,.T.);
#22153=EDGE_CURVE('',#17383,#17378,#14513,.T.);
#22154=EDGE_CURVE('',#17384,#17385,#10515,.T.);
#22155=EDGE_CURVE('',#17384,#17386,#10516,.T.);
#22156=EDGE_CURVE('',#17387,#17386,#10517,.T.);
#22157=EDGE_CURVE('',#17385,#17387,#10518,.T.);
#22158=EDGE_CURVE('',#17385,#17388,#14514,.T.);
#22159=EDGE_CURVE('',#17387,#17388,#10519,.T.);
#22160=EDGE_CURVE('',#17388,#17389,#10520,.T.);
#22161=EDGE_CURVE('',#17386,#17389,#10521,.T.);
#22162=EDGE_CURVE('',#17389,#17384,#14515,.T.);
#22163=EDGE_CURVE('',#17390,#17391,#10522,.T.);
#22164=EDGE_CURVE('',#17390,#17392,#10523,.T.);
#22165=EDGE_CURVE('',#17393,#17392,#10524,.T.);
#22166=EDGE_CURVE('',#17391,#17393,#10525,.T.);
#22167=EDGE_CURVE('',#17391,#17394,#14516,.T.);
#22168=EDGE_CURVE('',#17393,#17394,#10526,.T.);
#22169=EDGE_CURVE('',#17394,#17395,#10527,.T.);
#22170=EDGE_CURVE('',#17392,#17395,#10528,.T.);
#22171=EDGE_CURVE('',#17395,#17390,#14517,.T.);
#22172=EDGE_CURVE('',#17396,#17396,#14518,.T.);
#22173=EDGE_CURVE('',#17396,#17287,#10529,.T.);
#22174=EDGE_CURVE('',#17284,#17164,#10530,.T.);
#22175=EDGE_CURVE('',#17176,#17396,#10531,.T.);
#22176=EDGE_CURVE('',#17397,#17397,#14519,.T.);
#22177=EDGE_CURVE('',#17397,#17398,#10532,.T.);
#22178=EDGE_CURVE('',#17398,#17399,#805,.T.);
#22179=EDGE_CURVE('',#17399,#17400,#14520,.T.);
#22180=EDGE_CURVE('',#17400,#17401,#806,.T.);
#22181=EDGE_CURVE('',#17401,#17402,#14521,.T.);
#22182=EDGE_CURVE('',#17402,#17403,#807,.T.);
#22183=EDGE_CURVE('',#17403,#17404,#14522,.T.);
#22184=EDGE_CURVE('',#17404,#17405,#808,.T.);
#22185=EDGE_CURVE('',#17405,#17406,#14523,.T.);
#22186=EDGE_CURVE('',#17406,#17407,#809,.T.);
#22187=EDGE_CURVE('',#17407,#17408,#14524,.T.);
#22188=EDGE_CURVE('',#17408,#17409,#810,.T.);
#22189=EDGE_CURVE('',#17409,#17410,#14525,.T.);
#22190=EDGE_CURVE('',#17410,#17398,#811,.T.);
#22191=EDGE_CURVE('',#17400,#17411,#812,.T.);
#22192=EDGE_CURVE('',#17411,#17412,#813,.F.);
#22193=EDGE_CURVE('',#17412,#17413,#814,.T.);
#22194=EDGE_CURVE('',#17413,#17414,#815,.F.);
#22195=EDGE_CURVE('',#17414,#17401,#816,.T.);
#22196=EDGE_CURVE('',#17410,#17415,#817,.T.);
#22197=EDGE_CURVE('',#17415,#17416,#818,.F.);
#22198=EDGE_CURVE('',#17416,#17417,#819,.T.);
#22199=EDGE_CURVE('',#17417,#17411,#820,.F.);
#22200=EDGE_CURVE('',#17411,#17399,#821,.T.);
#22201=EDGE_CURVE('',#17415,#17409,#822,.T.);
#22202=EDGE_CURVE('',#17418,#17407,#823,.T.);
#22203=EDGE_CURVE('',#17408,#17418,#824,.T.);
#22204=EDGE_CURVE('',#17419,#17405,#825,.T.);
#22205=EDGE_CURVE('',#17406,#17419,#826,.T.);
#22206=EDGE_CURVE('',#17420,#17403,#827,.T.);
#22207=EDGE_CURVE('',#17404,#17420,#828,.T.);
#22208=EDGE_CURVE('',#17402,#17414,#829,.T.);
#22209=EDGE_CURVE('',#17418,#17421,#830,.F.);
#22210=EDGE_CURVE('',#17421,#17422,#831,.T.);
#22211=EDGE_CURVE('',#17422,#17415,#832,.F.);
#22212=EDGE_CURVE('',#17423,#17423,#14526,.T.);
#22213=EDGE_CURVE('',#17424,#17425,#10533,.T.);
#22214=EDGE_CURVE('',#17426,#17424,#10534,.T.);
#22215=EDGE_CURVE('',#17425,#17426,#10535,.T.);
#22216=EDGE_CURVE('',#17427,#17428,#10536,.T.);
#22217=EDGE_CURVE('',#17429,#17427,#10537,.T.);
#22218=EDGE_CURVE('',#17428,#17429,#10538,.T.);
#22219=EDGE_CURVE('',#17430,#17431,#10539,.T.);
#22220=EDGE_CURVE('',#17432,#17430,#10540,.T.);
#22221=EDGE_CURVE('',#17431,#17432,#10541,.T.);
#22222=EDGE_CURVE('',#17430,#17425,#10542,.T.);
#22223=EDGE_CURVE('',#17426,#17432,#10543,.T.);
#22224=EDGE_CURVE('',#17416,#17422,#10544,.T.);
#22225=EDGE_CURVE('',#17433,#17434,#10545,.T.);
#22226=EDGE_CURVE('',#17435,#17433,#10546,.T.);
#22227=EDGE_CURVE('',#17434,#17435,#10547,.T.);
#22228=EDGE_CURVE('',#17436,#17418,#833,.F.);
#22229=EDGE_CURVE('',#17421,#17436,#10548,.T.);
#22230=EDGE_CURVE('',#17437,#17438,#10549,.T.);
#22231=EDGE_CURVE('',#17439,#17437,#10550,.T.);
#22232=EDGE_CURVE('',#17438,#17439,#10551,.T.);
#22233=EDGE_CURVE('',#17437,#17431,#10552,.T.);
#22234=EDGE_CURVE('',#17432,#17439,#10553,.T.);
#22235=EDGE_CURVE('',#17412,#17417,#10554,.T.);
#22236=EDGE_CURVE('',#17440,#17441,#10555,.T.);
#22237=EDGE_CURVE('',#17442,#17440,#10556,.T.);
#22238=EDGE_CURVE('',#17441,#17442,#10557,.T.);
#22239=EDGE_CURVE('',#17433,#17442,#10558,.T.);
#22240=EDGE_CURVE('',#17440,#17435,#10559,.T.);
#22241=EDGE_CURVE('',#17419,#17443,#834,.F.);
#22242=EDGE_CURVE('',#17444,#17419,#835,.F.);
#22243=EDGE_CURVE('',#17443,#17444,#10560,.T.);
#22244=EDGE_CURVE('',#17445,#17413,#10561,.T.);
#22245=EDGE_CURVE('',#17414,#17445,#836,.F.);
#22246=EDGE_CURVE('',#17420,#17446,#837,.F.);
#22247=EDGE_CURVE('',#17447,#17420,#838,.F.);
#22248=EDGE_CURVE('',#17446,#17447,#10562,.T.);
#22249=EDGE_CURVE('',#17445,#17447,#839,.T.);
#22250=EDGE_CURVE('',#17447,#17441,#10563,.T.);
#22251=EDGE_CURVE('',#17442,#17446,#10564,.T.);
#22252=EDGE_CURVE('',#17446,#17444,#840,.T.);
#22253=EDGE_CURVE('',#17413,#17437,#10565,.T.);
#22254=EDGE_CURVE('',#17438,#17445,#10566,.T.);
#22255=EDGE_CURVE('',#17444,#17433,#10567,.T.);
#22256=EDGE_CURVE('',#17434,#17443,#10568,.T.);
#22257=EDGE_CURVE('',#17443,#17436,#841,.T.);
#22258=EDGE_CURVE('',#17441,#17438,#10569,.T.);
#22259=EDGE_CURVE('',#17439,#17440,#10570,.T.);
#22260=EDGE_CURVE('',#17417,#17430,#10571,.T.);
#22261=EDGE_CURVE('',#17431,#17412,#10572,.T.);
#22262=EDGE_CURVE('',#17436,#17427,#10573,.T.);
#22263=EDGE_CURVE('',#17428,#17421,#10574,.T.);
#22264=EDGE_CURVE('',#17427,#17434,#10575,.T.);
#22265=EDGE_CURVE('',#17435,#17429,#10576,.T.);
#22266=EDGE_CURVE('',#17422,#17424,#10577,.T.);
#22267=EDGE_CURVE('',#17425,#17416,#10578,.T.);
#22268=EDGE_CURVE('',#17424,#17428,#10579,.T.);
#22269=EDGE_CURVE('',#17429,#17426,#10580,.T.);
#22270=EDGE_CURVE('',#17448,#17448,#14527,.T.);
#22271=EDGE_CURVE('',#17449,#17450,#14528,.T.);
#22272=EDGE_CURVE('',#17449,#17423,#10581,.T.);
#22273=EDGE_CURVE('',#17450,#17449,#14529,.T.);
#22274=EDGE_CURVE('',#17448,#17451,#10582,.T.);
#22275=EDGE_CURVE('',#17451,#17451,#14530,.T.);
#22276=EDGE_CURVE('',#17452,#17452,#14531,.T.);
#22277=EDGE_CURVE('',#17450,#17452,#10583,.T.);
#22278=ORIENTED_EDGE('',*,*,#17453,.T.);
#22279=ORIENTED_EDGE('',*,*,#17454,.T.);
#22280=ORIENTED_EDGE('',*,*,#17455,.T.);
#22281=ORIENTED_EDGE('',*,*,#17456,.T.);
#22282=ORIENTED_EDGE('',*,*,#17457,.T.);
#22283=ORIENTED_EDGE('',*,*,#17455,.F.);
#22284=ORIENTED_EDGE('',*,*,#17456,.F.);
#22285=ORIENTED_EDGE('',*,*,#17457,.F.);
#22286=ORIENTED_EDGE('',*,*,#17458,.T.);
#22287=ORIENTED_EDGE('',*,*,#17459,.F.);
#22288=ORIENTED_EDGE('',*,*,#17460,.F.);
#22289=ORIENTED_EDGE('',*,*,#17458,.F.);
#22290=ORIENTED_EDGE('',*,*,#17461,.F.);
#22291=ORIENTED_EDGE('',*,*,#17462,.T.);
#22292=ORIENTED_EDGE('',*,*,#17453,.F.);
#22293=ORIENTED_EDGE('',*,*,#17454,.F.);
#22294=ORIENTED_EDGE('',*,*,#17462,.F.);
#22295=ORIENTED_EDGE('',*,*,#17459,.T.);
#22296=ORIENTED_EDGE('',*,*,#17460,.T.);
#22297=ORIENTED_EDGE('',*,*,#17463,.T.);
#22298=ORIENTED_EDGE('',*,*,#17464,.T.);
#22299=ORIENTED_EDGE('',*,*,#17463,.F.);
#22300=ORIENTED_EDGE('',*,*,#17464,.F.);
#22301=ORIENTED_EDGE('',*,*,#17465,.T.);
#22302=ORIENTED_EDGE('',*,*,#17466,.T.);
#22303=ORIENTED_EDGE('',*,*,#17467,.T.);
#22304=ORIENTED_EDGE('',*,*,#17468,.T.);
#22305=ORIENTED_EDGE('',*,*,#17469,.T.);
#22306=ORIENTED_EDGE('',*,*,#17467,.F.);
#22307=ORIENTED_EDGE('',*,*,#17470,.T.);
#22308=ORIENTED_EDGE('',*,*,#17471,.T.);
#22309=ORIENTED_EDGE('',*,*,#17468,.F.);
#22310=ORIENTED_EDGE('',*,*,#17469,.F.);
#22311=ORIENTED_EDGE('',*,*,#17471,.F.);
#22312=ORIENTED_EDGE('',*,*,#17472,.F.);
#22313=ORIENTED_EDGE('',*,*,#17466,.F.);
#22314=ORIENTED_EDGE('',*,*,#17473,.T.);
#22315=ORIENTED_EDGE('',*,*,#17474,.T.);
#22316=ORIENTED_EDGE('',*,*,#17475,.T.);
#22317=ORIENTED_EDGE('',*,*,#17476,.T.);
#22318=ORIENTED_EDGE('',*,*,#17474,.F.);
#22319=ORIENTED_EDGE('',*,*,#17475,.F.);
#22320=ORIENTED_EDGE('',*,*,#17476,.F.);
#22321=ORIENTED_EDGE('',*,*,#17477,.T.);
#22322=ORIENTED_EDGE('',*,*,#17478,.F.);
#22323=ORIENTED_EDGE('',*,*,#17479,.F.);
#22324=ORIENTED_EDGE('',*,*,#17477,.F.);
#22325=ORIENTED_EDGE('',*,*,#17473,.F.);
#22326=ORIENTED_EDGE('',*,*,#17480,.F.);
#22327=ORIENTED_EDGE('',*,*,#17478,.T.);
#22328=ORIENTED_EDGE('',*,*,#17479,.T.);
#22329=ORIENTED_EDGE('',*,*,#17481,.T.);
#22330=ORIENTED_EDGE('',*,*,#17482,.T.);
#22331=ORIENTED_EDGE('',*,*,#17483,.T.);
#22332=ORIENTED_EDGE('',*,*,#17481,.F.);
#22333=ORIENTED_EDGE('',*,*,#17482,.F.);
#22334=ORIENTED_EDGE('',*,*,#17483,.F.);
#22335=ORIENTED_EDGE('',*,*,#17484,.T.);
#22336=ORIENTED_EDGE('',*,*,#17485,.T.);
#22337=ORIENTED_EDGE('',*,*,#17484,.F.);
#22338=ORIENTED_EDGE('',*,*,#17486,.T.);
#22339=ORIENTED_EDGE('',*,*,#17487,.T.);
#22340=ORIENTED_EDGE('',*,*,#17488,.T.);
#22341=ORIENTED_EDGE('',*,*,#17489,.T.);
#22342=ORIENTED_EDGE('',*,*,#17490,.T.);
#22343=ORIENTED_EDGE('',*,*,#17488,.F.);
#22344=ORIENTED_EDGE('',*,*,#17489,.F.);
#22345=ORIENTED_EDGE('',*,*,#17490,.F.);
#22346=ORIENTED_EDGE('',*,*,#17491,.T.);
#22347=ORIENTED_EDGE('',*,*,#17492,.F.);
#22348=ORIENTED_EDGE('',*,*,#17493,.F.);
#22349=ORIENTED_EDGE('',*,*,#17491,.F.);
#22350=ORIENTED_EDGE('',*,*,#17494,.F.);
#22351=ORIENTED_EDGE('',*,*,#17495,.T.);
#22352=ORIENTED_EDGE('',*,*,#17486,.F.);
#22353=ORIENTED_EDGE('',*,*,#17487,.F.);
#22354=ORIENTED_EDGE('',*,*,#17495,.F.);
#22355=ORIENTED_EDGE('',*,*,#17492,.T.);
#22356=ORIENTED_EDGE('',*,*,#17493,.T.);
#22357=ORIENTED_EDGE('',*,*,#17496,.T.);
#22358=ORIENTED_EDGE('',*,*,#17497,.T.);
#22359=ORIENTED_EDGE('',*,*,#17498,.T.);
#22360=ORIENTED_EDGE('',*,*,#17496,.F.);
#22361=ORIENTED_EDGE('',*,*,#17497,.F.);
#22362=ORIENTED_EDGE('',*,*,#17498,.F.);
#22363=ORIENTED_EDGE('',*,*,#17499,.T.);
#22364=ORIENTED_EDGE('',*,*,#17500,.F.);
#22365=ORIENTED_EDGE('',*,*,#17501,.F.);
#22366=ORIENTED_EDGE('',*,*,#17499,.F.);
#22367=ORIENTED_EDGE('',*,*,#17500,.T.);
#22368=ORIENTED_EDGE('',*,*,#17501,.T.);
#22369=ORIENTED_EDGE('',*,*,#17502,.T.);
#22370=ORIENTED_EDGE('',*,*,#17503,.T.);
#22371=ORIENTED_EDGE('',*,*,#17504,.T.);
#22372=ORIENTED_EDGE('',*,*,#17502,.F.);
#22373=ORIENTED_EDGE('',*,*,#17503,.F.);
#22374=ORIENTED_EDGE('',*,*,#17504,.F.);
#22375=ORIENTED_EDGE('',*,*,#17505,.T.);
#22376=ORIENTED_EDGE('',*,*,#17506,.F.);
#22377=ORIENTED_EDGE('',*,*,#17507,.F.);
#22378=ORIENTED_EDGE('',*,*,#17505,.F.);
#22379=ORIENTED_EDGE('',*,*,#17506,.T.);
#22380=ORIENTED_EDGE('',*,*,#17507,.T.);
#22381=ORIENTED_EDGE('',*,*,#17508,.T.);
#22382=ORIENTED_EDGE('',*,*,#17509,.T.);
#22383=ORIENTED_EDGE('',*,*,#17510,.T.);
#22384=ORIENTED_EDGE('',*,*,#17508,.F.);
#22385=ORIENTED_EDGE('',*,*,#17509,.F.);
#22386=ORIENTED_EDGE('',*,*,#17510,.F.);
#22387=ORIENTED_EDGE('',*,*,#17511,.T.);
#22388=ORIENTED_EDGE('',*,*,#17512,.T.);
#22389=ORIENTED_EDGE('',*,*,#17513,.F.);
#22390=ORIENTED_EDGE('',*,*,#17514,.T.);
#22391=ORIENTED_EDGE('',*,*,#17515,.F.);
#22392=ORIENTED_EDGE('',*,*,#17516,.T.);
#22393=ORIENTED_EDGE('',*,*,#17517,.T.);
#22394=ORIENTED_EDGE('',*,*,#17518,.T.);
#22395=ORIENTED_EDGE('',*,*,#17517,.F.);
#22396=ORIENTED_EDGE('',*,*,#17519,.T.);
#22397=ORIENTED_EDGE('',*,*,#17520,.F.);
#22398=ORIENTED_EDGE('',*,*,#17521,.T.);
#22399=ORIENTED_EDGE('',*,*,#17522,.F.);
#22400=ORIENTED_EDGE('',*,*,#17523,.T.);
#22401=ORIENTED_EDGE('',*,*,#17511,.F.);
#22402=ORIENTED_EDGE('',*,*,#17524,.T.);
#22403=ORIENTED_EDGE('',*,*,#17525,.F.);
#22404=ORIENTED_EDGE('',*,*,#17526,.T.);
#22405=ORIENTED_EDGE('',*,*,#17527,.F.);
#22406=ORIENTED_EDGE('',*,*,#17528,.T.);
#22407=ORIENTED_EDGE('',*,*,#17529,.F.);
#22408=ORIENTED_EDGE('',*,*,#17530,.T.);
#22409=ORIENTED_EDGE('',*,*,#17531,.F.);
#22410=ORIENTED_EDGE('',*,*,#17532,.T.);
#22411=ORIENTED_EDGE('',*,*,#17533,.F.);
#22412=ORIENTED_EDGE('',*,*,#17534,.T.);
#22413=ORIENTED_EDGE('',*,*,#17535,.F.);
#22414=ORIENTED_EDGE('',*,*,#17536,.T.);
#22415=ORIENTED_EDGE('',*,*,#17537,.F.);
#22416=ORIENTED_EDGE('',*,*,#17538,.T.);
#22417=ORIENTED_EDGE('',*,*,#17539,.F.);
#22418=ORIENTED_EDGE('',*,*,#17540,.T.);
#22419=ORIENTED_EDGE('',*,*,#17541,.F.);
#22420=ORIENTED_EDGE('',*,*,#17542,.T.);
#22421=ORIENTED_EDGE('',*,*,#17543,.F.);
#22422=ORIENTED_EDGE('',*,*,#17544,.T.);
#22423=ORIENTED_EDGE('',*,*,#17545,.F.);
#22424=ORIENTED_EDGE('',*,*,#17546,.T.);
#22425=ORIENTED_EDGE('',*,*,#17547,.F.);
#22426=ORIENTED_EDGE('',*,*,#17548,.T.);
#22427=ORIENTED_EDGE('',*,*,#17549,.F.);
#22428=ORIENTED_EDGE('',*,*,#17550,.T.);
#22429=ORIENTED_EDGE('',*,*,#17551,.F.);
#22430=ORIENTED_EDGE('',*,*,#17552,.T.);
#22431=ORIENTED_EDGE('',*,*,#17553,.F.);
#22432=ORIENTED_EDGE('',*,*,#17554,.T.);
#22433=ORIENTED_EDGE('',*,*,#17555,.F.);
#22434=ORIENTED_EDGE('',*,*,#17556,.T.);
#22435=ORIENTED_EDGE('',*,*,#17557,.F.);
#22436=ORIENTED_EDGE('',*,*,#17558,.T.);
#22437=ORIENTED_EDGE('',*,*,#17559,.F.);
#22438=ORIENTED_EDGE('',*,*,#17560,.T.);
#22439=ORIENTED_EDGE('',*,*,#17561,.F.);
#22440=ORIENTED_EDGE('',*,*,#17562,.T.);
#22441=ORIENTED_EDGE('',*,*,#17563,.F.);
#22442=ORIENTED_EDGE('',*,*,#17564,.T.);
#22443=ORIENTED_EDGE('',*,*,#17565,.F.);
#22444=ORIENTED_EDGE('',*,*,#17566,.T.);
#22445=ORIENTED_EDGE('',*,*,#17567,.F.);
#22446=ORIENTED_EDGE('',*,*,#17568,.T.);
#22447=ORIENTED_EDGE('',*,*,#17569,.F.);
#22448=ORIENTED_EDGE('',*,*,#17570,.T.);
#22449=ORIENTED_EDGE('',*,*,#17571,.F.);
#22450=ORIENTED_EDGE('',*,*,#17572,.T.);
#22451=ORIENTED_EDGE('',*,*,#17573,.F.);
#22452=ORIENTED_EDGE('',*,*,#17574,.T.);
#22453=ORIENTED_EDGE('',*,*,#17575,.F.);
#22454=ORIENTED_EDGE('',*,*,#17576,.T.);
#22455=ORIENTED_EDGE('',*,*,#17577,.F.);
#22456=ORIENTED_EDGE('',*,*,#17578,.T.);
#22457=ORIENTED_EDGE('',*,*,#17579,.F.);
#22458=ORIENTED_EDGE('',*,*,#17580,.T.);
#22459=ORIENTED_EDGE('',*,*,#17581,.F.);
#22460=ORIENTED_EDGE('',*,*,#17582,.T.);
#22461=ORIENTED_EDGE('',*,*,#17583,.F.);
#22462=ORIENTED_EDGE('',*,*,#17584,.T.);
#22463=ORIENTED_EDGE('',*,*,#17585,.F.);
#22464=ORIENTED_EDGE('',*,*,#17586,.T.);
#22465=ORIENTED_EDGE('',*,*,#17587,.F.);
#22466=ORIENTED_EDGE('',*,*,#17588,.T.);
#22467=ORIENTED_EDGE('',*,*,#17589,.F.);
#22468=ORIENTED_EDGE('',*,*,#17590,.T.);
#22469=ORIENTED_EDGE('',*,*,#17591,.F.);
#22470=ORIENTED_EDGE('',*,*,#17592,.T.);
#22471=ORIENTED_EDGE('',*,*,#17593,.F.);
#22472=ORIENTED_EDGE('',*,*,#17594,.T.);
#22473=ORIENTED_EDGE('',*,*,#17595,.F.);
#22474=ORIENTED_EDGE('',*,*,#17596,.T.);
#22475=ORIENTED_EDGE('',*,*,#17597,.F.);
#22476=ORIENTED_EDGE('',*,*,#17598,.T.);
#22477=ORIENTED_EDGE('',*,*,#17599,.F.);
#22478=ORIENTED_EDGE('',*,*,#17600,.T.);
#22479=ORIENTED_EDGE('',*,*,#17601,.F.);
#22480=ORIENTED_EDGE('',*,*,#17602,.T.);
#22481=ORIENTED_EDGE('',*,*,#17603,.F.);
#22482=ORIENTED_EDGE('',*,*,#17604,.T.);
#22483=ORIENTED_EDGE('',*,*,#17605,.F.);
#22484=ORIENTED_EDGE('',*,*,#17606,.T.);
#22485=ORIENTED_EDGE('',*,*,#17607,.F.);
#22486=ORIENTED_EDGE('',*,*,#17608,.T.);
#22487=ORIENTED_EDGE('',*,*,#17609,.F.);
#22488=ORIENTED_EDGE('',*,*,#17610,.T.);
#22489=ORIENTED_EDGE('',*,*,#17611,.F.);
#22490=ORIENTED_EDGE('',*,*,#17612,.T.);
#22491=ORIENTED_EDGE('',*,*,#17613,.F.);
#22492=ORIENTED_EDGE('',*,*,#17614,.T.);
#22493=ORIENTED_EDGE('',*,*,#17615,.F.);
#22494=ORIENTED_EDGE('',*,*,#17616,.T.);
#22495=ORIENTED_EDGE('',*,*,#17617,.F.);
#22496=ORIENTED_EDGE('',*,*,#17618,.T.);
#22497=ORIENTED_EDGE('',*,*,#17619,.F.);
#22498=ORIENTED_EDGE('',*,*,#17620,.T.);
#22499=ORIENTED_EDGE('',*,*,#17621,.F.);
#22500=ORIENTED_EDGE('',*,*,#17622,.T.);
#22501=ORIENTED_EDGE('',*,*,#17623,.F.);
#22502=ORIENTED_EDGE('',*,*,#17624,.T.);
#22503=ORIENTED_EDGE('',*,*,#17625,.F.);
#22504=ORIENTED_EDGE('',*,*,#17626,.T.);
#22505=ORIENTED_EDGE('',*,*,#17627,.F.);
#22506=ORIENTED_EDGE('',*,*,#17628,.T.);
#22507=ORIENTED_EDGE('',*,*,#17629,.F.);
#22508=ORIENTED_EDGE('',*,*,#17630,.T.);
#22509=ORIENTED_EDGE('',*,*,#17631,.F.);
#22510=ORIENTED_EDGE('',*,*,#17632,.T.);
#22511=ORIENTED_EDGE('',*,*,#17633,.F.);
#22512=ORIENTED_EDGE('',*,*,#17634,.T.);
#22513=ORIENTED_EDGE('',*,*,#17635,.F.);
#22514=ORIENTED_EDGE('',*,*,#17636,.T.);
#22515=ORIENTED_EDGE('',*,*,#17637,.F.);
#22516=ORIENTED_EDGE('',*,*,#17638,.T.);
#22517=ORIENTED_EDGE('',*,*,#17639,.F.);
#22518=ORIENTED_EDGE('',*,*,#17640,.T.);
#22519=ORIENTED_EDGE('',*,*,#17641,.F.);
#22520=ORIENTED_EDGE('',*,*,#17642,.T.);
#22521=ORIENTED_EDGE('',*,*,#17643,.F.);
#22522=ORIENTED_EDGE('',*,*,#17644,.T.);
#22523=ORIENTED_EDGE('',*,*,#17645,.F.);
#22524=ORIENTED_EDGE('',*,*,#17646,.T.);
#22525=ORIENTED_EDGE('',*,*,#17647,.F.);
#22526=ORIENTED_EDGE('',*,*,#17648,.T.);
#22527=ORIENTED_EDGE('',*,*,#17649,.F.);
#22528=ORIENTED_EDGE('',*,*,#17650,.T.);
#22529=ORIENTED_EDGE('',*,*,#17651,.F.);
#22530=ORIENTED_EDGE('',*,*,#17652,.T.);
#22531=ORIENTED_EDGE('',*,*,#17653,.F.);
#22532=ORIENTED_EDGE('',*,*,#17654,.T.);
#22533=ORIENTED_EDGE('',*,*,#17655,.F.);
#22534=ORIENTED_EDGE('',*,*,#17656,.T.);
#22535=ORIENTED_EDGE('',*,*,#17657,.F.);
#22536=ORIENTED_EDGE('',*,*,#17658,.T.);
#22537=ORIENTED_EDGE('',*,*,#17659,.F.);
#22538=ORIENTED_EDGE('',*,*,#17660,.T.);
#22539=ORIENTED_EDGE('',*,*,#17661,.F.);
#22540=ORIENTED_EDGE('',*,*,#17662,.T.);
#22541=ORIENTED_EDGE('',*,*,#17663,.F.);
#22542=ORIENTED_EDGE('',*,*,#17664,.T.);
#22543=ORIENTED_EDGE('',*,*,#17665,.F.);
#22544=ORIENTED_EDGE('',*,*,#17666,.T.);
#22545=ORIENTED_EDGE('',*,*,#17667,.F.);
#22546=ORIENTED_EDGE('',*,*,#17668,.T.);
#22547=ORIENTED_EDGE('',*,*,#17669,.F.);
#22548=ORIENTED_EDGE('',*,*,#17670,.T.);
#22549=ORIENTED_EDGE('',*,*,#17671,.F.);
#22550=ORIENTED_EDGE('',*,*,#17672,.T.);
#22551=ORIENTED_EDGE('',*,*,#17673,.F.);
#22552=ORIENTED_EDGE('',*,*,#17674,.T.);
#22553=ORIENTED_EDGE('',*,*,#17675,.F.);
#22554=ORIENTED_EDGE('',*,*,#17676,.T.);
#22555=ORIENTED_EDGE('',*,*,#17677,.F.);
#22556=ORIENTED_EDGE('',*,*,#17678,.T.);
#22557=ORIENTED_EDGE('',*,*,#17679,.F.);
#22558=ORIENTED_EDGE('',*,*,#17680,.T.);
#22559=ORIENTED_EDGE('',*,*,#17681,.F.);
#22560=ORIENTED_EDGE('',*,*,#17682,.T.);
#22561=ORIENTED_EDGE('',*,*,#17683,.F.);
#22562=ORIENTED_EDGE('',*,*,#17684,.T.);
#22563=ORIENTED_EDGE('',*,*,#17685,.F.);
#22564=ORIENTED_EDGE('',*,*,#17686,.T.);
#22565=ORIENTED_EDGE('',*,*,#17687,.F.);
#22566=ORIENTED_EDGE('',*,*,#17688,.T.);
#22567=ORIENTED_EDGE('',*,*,#17689,.F.);
#22568=ORIENTED_EDGE('',*,*,#17690,.T.);
#22569=ORIENTED_EDGE('',*,*,#17691,.F.);
#22570=ORIENTED_EDGE('',*,*,#17692,.T.);
#22571=ORIENTED_EDGE('',*,*,#17693,.F.);
#22572=ORIENTED_EDGE('',*,*,#17694,.T.);
#22573=ORIENTED_EDGE('',*,*,#17695,.F.);
#22574=ORIENTED_EDGE('',*,*,#17696,.T.);
#22575=ORIENTED_EDGE('',*,*,#17697,.F.);
#22576=ORIENTED_EDGE('',*,*,#17698,.T.);
#22577=ORIENTED_EDGE('',*,*,#17699,.F.);
#22578=ORIENTED_EDGE('',*,*,#17700,.T.);
#22579=ORIENTED_EDGE('',*,*,#17701,.F.);
#22580=ORIENTED_EDGE('',*,*,#17702,.T.);
#22581=ORIENTED_EDGE('',*,*,#17703,.F.);
#22582=ORIENTED_EDGE('',*,*,#17704,.T.);
#22583=ORIENTED_EDGE('',*,*,#17705,.F.);
#22584=ORIENTED_EDGE('',*,*,#17706,.T.);
#22585=ORIENTED_EDGE('',*,*,#17707,.F.);
#22586=ORIENTED_EDGE('',*,*,#17708,.T.);
#22587=ORIENTED_EDGE('',*,*,#17709,.F.);
#22588=ORIENTED_EDGE('',*,*,#17710,.T.);
#22589=ORIENTED_EDGE('',*,*,#17711,.F.);
#22590=ORIENTED_EDGE('',*,*,#17712,.T.);
#22591=ORIENTED_EDGE('',*,*,#17713,.F.);
#22592=ORIENTED_EDGE('',*,*,#17714,.T.);
#22593=ORIENTED_EDGE('',*,*,#17715,.F.);
#22594=ORIENTED_EDGE('',*,*,#17716,.T.);
#22595=ORIENTED_EDGE('',*,*,#17717,.F.);
#22596=ORIENTED_EDGE('',*,*,#17718,.T.);
#22597=ORIENTED_EDGE('',*,*,#17719,.F.);
#22598=ORIENTED_EDGE('',*,*,#17720,.T.);
#22599=ORIENTED_EDGE('',*,*,#17721,.F.);
#22600=ORIENTED_EDGE('',*,*,#17722,.T.);
#22601=ORIENTED_EDGE('',*,*,#17723,.F.);
#22602=ORIENTED_EDGE('',*,*,#17724,.T.);
#22603=ORIENTED_EDGE('',*,*,#17725,.F.);
#22604=ORIENTED_EDGE('',*,*,#17726,.T.);
#22605=ORIENTED_EDGE('',*,*,#17727,.F.);
#22606=ORIENTED_EDGE('',*,*,#17728,.T.);
#22607=ORIENTED_EDGE('',*,*,#17729,.F.);
#22608=ORIENTED_EDGE('',*,*,#17730,.T.);
#22609=ORIENTED_EDGE('',*,*,#17731,.F.);
#22610=ORIENTED_EDGE('',*,*,#17732,.T.);
#22611=ORIENTED_EDGE('',*,*,#17733,.F.);
#22612=ORIENTED_EDGE('',*,*,#17734,.T.);
#22613=ORIENTED_EDGE('',*,*,#17735,.F.);
#22614=ORIENTED_EDGE('',*,*,#17736,.T.);
#22615=ORIENTED_EDGE('',*,*,#17737,.F.);
#22616=ORIENTED_EDGE('',*,*,#17738,.T.);
#22617=ORIENTED_EDGE('',*,*,#17739,.F.);
#22618=ORIENTED_EDGE('',*,*,#17740,.T.);
#22619=ORIENTED_EDGE('',*,*,#17741,.F.);
#22620=ORIENTED_EDGE('',*,*,#17742,.T.);
#22621=ORIENTED_EDGE('',*,*,#17743,.F.);
#22622=ORIENTED_EDGE('',*,*,#17744,.T.);
#22623=ORIENTED_EDGE('',*,*,#17745,.F.);
#22624=ORIENTED_EDGE('',*,*,#17746,.T.);
#22625=ORIENTED_EDGE('',*,*,#17747,.F.);
#22626=ORIENTED_EDGE('',*,*,#17748,.T.);
#22627=ORIENTED_EDGE('',*,*,#17749,.F.);
#22628=ORIENTED_EDGE('',*,*,#17750,.T.);
#22629=ORIENTED_EDGE('',*,*,#17751,.F.);
#22630=ORIENTED_EDGE('',*,*,#17752,.T.);
#22631=ORIENTED_EDGE('',*,*,#17753,.F.);
#22632=ORIENTED_EDGE('',*,*,#17754,.T.);
#22633=ORIENTED_EDGE('',*,*,#17755,.F.);
#22634=ORIENTED_EDGE('',*,*,#17756,.T.);
#22635=ORIENTED_EDGE('',*,*,#17757,.F.);
#22636=ORIENTED_EDGE('',*,*,#17758,.T.);
#22637=ORIENTED_EDGE('',*,*,#17759,.F.);
#22638=ORIENTED_EDGE('',*,*,#17760,.T.);
#22639=ORIENTED_EDGE('',*,*,#17761,.F.);
#22640=ORIENTED_EDGE('',*,*,#17762,.T.);
#22641=ORIENTED_EDGE('',*,*,#17763,.F.);
#22642=ORIENTED_EDGE('',*,*,#17764,.T.);
#22643=ORIENTED_EDGE('',*,*,#17765,.F.);
#22644=ORIENTED_EDGE('',*,*,#17766,.T.);
#22645=ORIENTED_EDGE('',*,*,#17767,.F.);
#22646=ORIENTED_EDGE('',*,*,#17768,.T.);
#22647=ORIENTED_EDGE('',*,*,#17769,.F.);
#22648=ORIENTED_EDGE('',*,*,#17770,.T.);
#22649=ORIENTED_EDGE('',*,*,#17771,.F.);
#22650=ORIENTED_EDGE('',*,*,#17772,.T.);
#22651=ORIENTED_EDGE('',*,*,#17773,.F.);
#22652=ORIENTED_EDGE('',*,*,#17774,.T.);
#22653=ORIENTED_EDGE('',*,*,#17775,.F.);
#22654=ORIENTED_EDGE('',*,*,#17776,.T.);
#22655=ORIENTED_EDGE('',*,*,#17777,.F.);
#22656=ORIENTED_EDGE('',*,*,#17778,.T.);
#22657=ORIENTED_EDGE('',*,*,#17779,.F.);
#22658=ORIENTED_EDGE('',*,*,#17780,.T.);
#22659=ORIENTED_EDGE('',*,*,#17781,.F.);
#22660=ORIENTED_EDGE('',*,*,#17782,.T.);
#22661=ORIENTED_EDGE('',*,*,#17783,.F.);
#22662=ORIENTED_EDGE('',*,*,#17784,.T.);
#22663=ORIENTED_EDGE('',*,*,#17785,.F.);
#22664=ORIENTED_EDGE('',*,*,#17786,.T.);
#22665=ORIENTED_EDGE('',*,*,#17787,.F.);
#22666=ORIENTED_EDGE('',*,*,#17788,.T.);
#22667=ORIENTED_EDGE('',*,*,#17789,.F.);
#22668=ORIENTED_EDGE('',*,*,#17790,.T.);
#22669=ORIENTED_EDGE('',*,*,#17791,.F.);
#22670=ORIENTED_EDGE('',*,*,#17792,.T.);
#22671=ORIENTED_EDGE('',*,*,#17793,.F.);
#22672=ORIENTED_EDGE('',*,*,#17794,.T.);
#22673=ORIENTED_EDGE('',*,*,#17795,.F.);
#22674=ORIENTED_EDGE('',*,*,#17796,.T.);
#22675=ORIENTED_EDGE('',*,*,#17797,.F.);
#22676=ORIENTED_EDGE('',*,*,#17798,.T.);
#22677=ORIENTED_EDGE('',*,*,#17799,.F.);
#22678=ORIENTED_EDGE('',*,*,#17800,.T.);
#22679=ORIENTED_EDGE('',*,*,#17801,.F.);
#22680=ORIENTED_EDGE('',*,*,#17802,.T.);
#22681=ORIENTED_EDGE('',*,*,#17803,.F.);
#22682=ORIENTED_EDGE('',*,*,#17804,.T.);
#22683=ORIENTED_EDGE('',*,*,#17805,.F.);
#22684=ORIENTED_EDGE('',*,*,#17806,.T.);
#22685=ORIENTED_EDGE('',*,*,#17807,.F.);
#22686=ORIENTED_EDGE('',*,*,#17808,.T.);
#22687=ORIENTED_EDGE('',*,*,#17809,.F.);
#22688=ORIENTED_EDGE('',*,*,#17810,.T.);
#22689=ORIENTED_EDGE('',*,*,#17811,.F.);
#22690=ORIENTED_EDGE('',*,*,#17812,.T.);
#22691=ORIENTED_EDGE('',*,*,#17813,.F.);
#22692=ORIENTED_EDGE('',*,*,#17814,.T.);
#22693=ORIENTED_EDGE('',*,*,#17815,.F.);
#22694=ORIENTED_EDGE('',*,*,#17816,.T.);
#22695=ORIENTED_EDGE('',*,*,#17817,.F.);
#22696=ORIENTED_EDGE('',*,*,#17818,.T.);
#22697=ORIENTED_EDGE('',*,*,#17819,.F.);
#22698=ORIENTED_EDGE('',*,*,#17820,.T.);
#22699=ORIENTED_EDGE('',*,*,#17821,.F.);
#22700=ORIENTED_EDGE('',*,*,#17822,.T.);
#22701=ORIENTED_EDGE('',*,*,#17823,.F.);
#22702=ORIENTED_EDGE('',*,*,#17824,.T.);
#22703=ORIENTED_EDGE('',*,*,#17825,.F.);
#22704=ORIENTED_EDGE('',*,*,#17826,.T.);
#22705=ORIENTED_EDGE('',*,*,#17827,.F.);
#22706=ORIENTED_EDGE('',*,*,#17828,.T.);
#22707=ORIENTED_EDGE('',*,*,#17829,.F.);
#22708=ORIENTED_EDGE('',*,*,#17830,.T.);
#22709=ORIENTED_EDGE('',*,*,#17831,.F.);
#22710=ORIENTED_EDGE('',*,*,#17832,.T.);
#22711=ORIENTED_EDGE('',*,*,#17833,.F.);
#22712=ORIENTED_EDGE('',*,*,#17834,.T.);
#22713=ORIENTED_EDGE('',*,*,#17835,.F.);
#22714=ORIENTED_EDGE('',*,*,#17836,.T.);
#22715=ORIENTED_EDGE('',*,*,#17837,.F.);
#22716=ORIENTED_EDGE('',*,*,#17838,.T.);
#22717=ORIENTED_EDGE('',*,*,#17839,.F.);
#22718=ORIENTED_EDGE('',*,*,#17840,.T.);
#22719=ORIENTED_EDGE('',*,*,#17841,.F.);
#22720=ORIENTED_EDGE('',*,*,#17842,.T.);
#22721=ORIENTED_EDGE('',*,*,#17843,.F.);
#22722=ORIENTED_EDGE('',*,*,#17844,.T.);
#22723=ORIENTED_EDGE('',*,*,#17845,.F.);
#22724=ORIENTED_EDGE('',*,*,#17846,.T.);
#22725=ORIENTED_EDGE('',*,*,#17847,.F.);
#22726=ORIENTED_EDGE('',*,*,#17848,.T.);
#22727=ORIENTED_EDGE('',*,*,#17849,.F.);
#22728=ORIENTED_EDGE('',*,*,#17850,.T.);
#22729=ORIENTED_EDGE('',*,*,#17851,.F.);
#22730=ORIENTED_EDGE('',*,*,#17852,.T.);
#22731=ORIENTED_EDGE('',*,*,#17853,.F.);
#22732=ORIENTED_EDGE('',*,*,#17854,.T.);
#22733=ORIENTED_EDGE('',*,*,#17855,.F.);
#22734=ORIENTED_EDGE('',*,*,#17856,.T.);
#22735=ORIENTED_EDGE('',*,*,#17857,.F.);
#22736=ORIENTED_EDGE('',*,*,#17858,.T.);
#22737=ORIENTED_EDGE('',*,*,#17859,.F.);
#22738=ORIENTED_EDGE('',*,*,#17860,.T.);
#22739=ORIENTED_EDGE('',*,*,#17861,.F.);
#22740=ORIENTED_EDGE('',*,*,#17862,.T.);
#22741=ORIENTED_EDGE('',*,*,#17863,.F.);
#22742=ORIENTED_EDGE('',*,*,#17864,.T.);
#22743=ORIENTED_EDGE('',*,*,#17865,.F.);
#22744=ORIENTED_EDGE('',*,*,#17866,.T.);
#22745=ORIENTED_EDGE('',*,*,#17867,.F.);
#22746=ORIENTED_EDGE('',*,*,#17868,.T.);
#22747=ORIENTED_EDGE('',*,*,#17869,.F.);
#22748=ORIENTED_EDGE('',*,*,#17870,.T.);
#22749=ORIENTED_EDGE('',*,*,#17871,.F.);
#22750=ORIENTED_EDGE('',*,*,#17872,.T.);
#22751=ORIENTED_EDGE('',*,*,#17873,.F.);
#22752=ORIENTED_EDGE('',*,*,#17874,.T.);
#22753=ORIENTED_EDGE('',*,*,#17875,.F.);
#22754=ORIENTED_EDGE('',*,*,#17876,.T.);
#22755=ORIENTED_EDGE('',*,*,#17877,.F.);
#22756=ORIENTED_EDGE('',*,*,#17878,.T.);
#22757=ORIENTED_EDGE('',*,*,#17879,.F.);
#22758=ORIENTED_EDGE('',*,*,#17880,.T.);
#22759=ORIENTED_EDGE('',*,*,#17881,.F.);
#22760=ORIENTED_EDGE('',*,*,#17882,.T.);
#22761=ORIENTED_EDGE('',*,*,#17883,.F.);
#22762=ORIENTED_EDGE('',*,*,#17884,.T.);
#22763=ORIENTED_EDGE('',*,*,#17885,.F.);
#22764=ORIENTED_EDGE('',*,*,#17886,.T.);
#22765=ORIENTED_EDGE('',*,*,#17887,.F.);
#22766=ORIENTED_EDGE('',*,*,#17888,.T.);
#22767=ORIENTED_EDGE('',*,*,#17889,.F.);
#22768=ORIENTED_EDGE('',*,*,#17890,.T.);
#22769=ORIENTED_EDGE('',*,*,#17891,.F.);
#22770=ORIENTED_EDGE('',*,*,#17892,.T.);
#22771=ORIENTED_EDGE('',*,*,#17893,.F.);
#22772=ORIENTED_EDGE('',*,*,#17894,.T.);
#22773=ORIENTED_EDGE('',*,*,#17895,.F.);
#22774=ORIENTED_EDGE('',*,*,#17896,.T.);
#22775=ORIENTED_EDGE('',*,*,#17897,.F.);
#22776=ORIENTED_EDGE('',*,*,#17898,.T.);
#22777=ORIENTED_EDGE('',*,*,#17899,.F.);
#22778=ORIENTED_EDGE('',*,*,#17900,.T.);
#22779=ORIENTED_EDGE('',*,*,#17901,.F.);
#22780=ORIENTED_EDGE('',*,*,#17902,.T.);
#22781=ORIENTED_EDGE('',*,*,#17903,.F.);
#22782=ORIENTED_EDGE('',*,*,#17904,.T.);
#22783=ORIENTED_EDGE('',*,*,#17905,.F.);
#22784=ORIENTED_EDGE('',*,*,#17906,.T.);
#22785=ORIENTED_EDGE('',*,*,#17907,.F.);
#22786=ORIENTED_EDGE('',*,*,#17908,.T.);
#22787=ORIENTED_EDGE('',*,*,#17909,.F.);
#22788=ORIENTED_EDGE('',*,*,#17910,.T.);
#22789=ORIENTED_EDGE('',*,*,#17911,.F.);
#22790=ORIENTED_EDGE('',*,*,#17912,.T.);
#22791=ORIENTED_EDGE('',*,*,#17913,.F.);
#22792=ORIENTED_EDGE('',*,*,#17914,.T.);
#22793=ORIENTED_EDGE('',*,*,#17915,.F.);
#22794=ORIENTED_EDGE('',*,*,#17916,.T.);
#22795=ORIENTED_EDGE('',*,*,#17917,.F.);
#22796=ORIENTED_EDGE('',*,*,#17918,.T.);
#22797=ORIENTED_EDGE('',*,*,#17919,.F.);
#22798=ORIENTED_EDGE('',*,*,#17920,.T.);
#22799=ORIENTED_EDGE('',*,*,#17921,.F.);
#22800=ORIENTED_EDGE('',*,*,#17922,.T.);
#22801=ORIENTED_EDGE('',*,*,#17923,.F.);
#22802=ORIENTED_EDGE('',*,*,#17924,.T.);
#22803=ORIENTED_EDGE('',*,*,#17925,.F.);
#22804=ORIENTED_EDGE('',*,*,#17926,.T.);
#22805=ORIENTED_EDGE('',*,*,#17927,.F.);
#22806=ORIENTED_EDGE('',*,*,#17928,.T.);
#22807=ORIENTED_EDGE('',*,*,#17929,.F.);
#22808=ORIENTED_EDGE('',*,*,#17930,.T.);
#22809=ORIENTED_EDGE('',*,*,#17931,.F.);
#22810=ORIENTED_EDGE('',*,*,#17932,.T.);
#22811=ORIENTED_EDGE('',*,*,#17933,.F.);
#22812=ORIENTED_EDGE('',*,*,#17934,.T.);
#22813=ORIENTED_EDGE('',*,*,#17935,.F.);
#22814=ORIENTED_EDGE('',*,*,#17936,.T.);
#22815=ORIENTED_EDGE('',*,*,#17937,.F.);
#22816=ORIENTED_EDGE('',*,*,#17938,.T.);
#22817=ORIENTED_EDGE('',*,*,#17939,.F.);
#22818=ORIENTED_EDGE('',*,*,#17940,.T.);
#22819=ORIENTED_EDGE('',*,*,#17941,.F.);
#22820=ORIENTED_EDGE('',*,*,#17942,.T.);
#22821=ORIENTED_EDGE('',*,*,#17943,.F.);
#22822=ORIENTED_EDGE('',*,*,#17944,.T.);
#22823=ORIENTED_EDGE('',*,*,#17945,.F.);
#22824=ORIENTED_EDGE('',*,*,#17946,.T.);
#22825=ORIENTED_EDGE('',*,*,#17947,.F.);
#22826=ORIENTED_EDGE('',*,*,#17948,.T.);
#22827=ORIENTED_EDGE('',*,*,#17949,.F.);
#22828=ORIENTED_EDGE('',*,*,#17950,.T.);
#22829=ORIENTED_EDGE('',*,*,#17951,.F.);
#22830=ORIENTED_EDGE('',*,*,#17952,.T.);
#22831=ORIENTED_EDGE('',*,*,#17953,.F.);
#22832=ORIENTED_EDGE('',*,*,#17954,.T.);
#22833=ORIENTED_EDGE('',*,*,#17955,.F.);
#22834=ORIENTED_EDGE('',*,*,#17956,.T.);
#22835=ORIENTED_EDGE('',*,*,#17957,.F.);
#22836=ORIENTED_EDGE('',*,*,#17958,.T.);
#22837=ORIENTED_EDGE('',*,*,#17959,.F.);
#22838=ORIENTED_EDGE('',*,*,#17960,.T.);
#22839=ORIENTED_EDGE('',*,*,#17961,.F.);
#22840=ORIENTED_EDGE('',*,*,#17962,.T.);
#22841=ORIENTED_EDGE('',*,*,#17963,.F.);
#22842=ORIENTED_EDGE('',*,*,#17964,.T.);
#22843=ORIENTED_EDGE('',*,*,#17965,.F.);
#22844=ORIENTED_EDGE('',*,*,#17966,.T.);
#22845=ORIENTED_EDGE('',*,*,#17967,.F.);
#22846=ORIENTED_EDGE('',*,*,#17968,.T.);
#22847=ORIENTED_EDGE('',*,*,#17969,.F.);
#22848=ORIENTED_EDGE('',*,*,#17970,.T.);
#22849=ORIENTED_EDGE('',*,*,#17971,.F.);
#22850=ORIENTED_EDGE('',*,*,#17972,.T.);
#22851=ORIENTED_EDGE('',*,*,#17973,.F.);
#22852=ORIENTED_EDGE('',*,*,#17974,.T.);
#22853=ORIENTED_EDGE('',*,*,#17975,.F.);
#22854=ORIENTED_EDGE('',*,*,#17976,.T.);
#22855=ORIENTED_EDGE('',*,*,#17977,.F.);
#22856=ORIENTED_EDGE('',*,*,#17978,.T.);
#22857=ORIENTED_EDGE('',*,*,#17979,.F.);
#22858=ORIENTED_EDGE('',*,*,#17980,.T.);
#22859=ORIENTED_EDGE('',*,*,#17981,.F.);
#22860=ORIENTED_EDGE('',*,*,#17982,.T.);
#22861=ORIENTED_EDGE('',*,*,#17983,.F.);
#22862=ORIENTED_EDGE('',*,*,#17984,.T.);
#22863=ORIENTED_EDGE('',*,*,#17985,.F.);
#22864=ORIENTED_EDGE('',*,*,#17986,.T.);
#22865=ORIENTED_EDGE('',*,*,#17987,.F.);
#22866=ORIENTED_EDGE('',*,*,#17988,.T.);
#22867=ORIENTED_EDGE('',*,*,#17989,.F.);
#22868=ORIENTED_EDGE('',*,*,#17990,.T.);
#22869=ORIENTED_EDGE('',*,*,#17991,.F.);
#22870=ORIENTED_EDGE('',*,*,#17992,.T.);
#22871=ORIENTED_EDGE('',*,*,#17993,.F.);
#22872=ORIENTED_EDGE('',*,*,#17994,.T.);
#22873=ORIENTED_EDGE('',*,*,#17995,.F.);
#22874=ORIENTED_EDGE('',*,*,#17996,.T.);
#22875=ORIENTED_EDGE('',*,*,#17997,.F.);
#22876=ORIENTED_EDGE('',*,*,#17998,.T.);
#22877=ORIENTED_EDGE('',*,*,#17999,.F.);
#22878=ORIENTED_EDGE('',*,*,#18000,.T.);
#22879=ORIENTED_EDGE('',*,*,#18001,.F.);
#22880=ORIENTED_EDGE('',*,*,#18002,.T.);
#22881=ORIENTED_EDGE('',*,*,#18003,.F.);
#22882=ORIENTED_EDGE('',*,*,#18004,.T.);
#22883=ORIENTED_EDGE('',*,*,#18005,.F.);
#22884=ORIENTED_EDGE('',*,*,#18006,.T.);
#22885=ORIENTED_EDGE('',*,*,#18007,.F.);
#22886=ORIENTED_EDGE('',*,*,#18008,.T.);
#22887=ORIENTED_EDGE('',*,*,#18009,.F.);
#22888=ORIENTED_EDGE('',*,*,#18010,.T.);
#22889=ORIENTED_EDGE('',*,*,#18011,.F.);
#22890=ORIENTED_EDGE('',*,*,#18012,.T.);
#22891=ORIENTED_EDGE('',*,*,#18013,.F.);
#22892=ORIENTED_EDGE('',*,*,#18014,.T.);
#22893=ORIENTED_EDGE('',*,*,#18015,.F.);
#22894=ORIENTED_EDGE('',*,*,#18016,.T.);
#22895=ORIENTED_EDGE('',*,*,#18017,.F.);
#22896=ORIENTED_EDGE('',*,*,#18018,.T.);
#22897=ORIENTED_EDGE('',*,*,#18019,.F.);
#22898=ORIENTED_EDGE('',*,*,#18020,.T.);
#22899=ORIENTED_EDGE('',*,*,#18021,.F.);
#22900=ORIENTED_EDGE('',*,*,#18022,.T.);
#22901=ORIENTED_EDGE('',*,*,#18023,.F.);
#22902=ORIENTED_EDGE('',*,*,#18024,.T.);
#22903=ORIENTED_EDGE('',*,*,#18025,.F.);
#22904=ORIENTED_EDGE('',*,*,#18026,.T.);
#22905=ORIENTED_EDGE('',*,*,#18027,.F.);
#22906=ORIENTED_EDGE('',*,*,#18028,.T.);
#22907=ORIENTED_EDGE('',*,*,#18029,.F.);
#22908=ORIENTED_EDGE('',*,*,#18030,.T.);
#22909=ORIENTED_EDGE('',*,*,#18031,.F.);
#22910=ORIENTED_EDGE('',*,*,#18032,.T.);
#22911=ORIENTED_EDGE('',*,*,#18033,.F.);
#22912=ORIENTED_EDGE('',*,*,#18034,.T.);
#22913=ORIENTED_EDGE('',*,*,#18035,.F.);
#22914=ORIENTED_EDGE('',*,*,#18036,.T.);
#22915=ORIENTED_EDGE('',*,*,#18037,.F.);
#22916=ORIENTED_EDGE('',*,*,#18038,.T.);
#22917=ORIENTED_EDGE('',*,*,#18039,.F.);
#22918=ORIENTED_EDGE('',*,*,#18040,.T.);
#22919=ORIENTED_EDGE('',*,*,#18041,.F.);
#22920=ORIENTED_EDGE('',*,*,#18042,.T.);
#22921=ORIENTED_EDGE('',*,*,#18043,.F.);
#22922=ORIENTED_EDGE('',*,*,#18044,.T.);
#22923=ORIENTED_EDGE('',*,*,#18045,.F.);
#22924=ORIENTED_EDGE('',*,*,#18046,.T.);
#22925=ORIENTED_EDGE('',*,*,#18047,.F.);
#22926=ORIENTED_EDGE('',*,*,#18048,.T.);
#22927=ORIENTED_EDGE('',*,*,#18049,.F.);
#22928=ORIENTED_EDGE('',*,*,#18050,.T.);
#22929=ORIENTED_EDGE('',*,*,#18051,.F.);
#22930=ORIENTED_EDGE('',*,*,#18052,.T.);
#22931=ORIENTED_EDGE('',*,*,#18053,.F.);
#22932=ORIENTED_EDGE('',*,*,#18054,.T.);
#22933=ORIENTED_EDGE('',*,*,#18055,.F.);
#22934=ORIENTED_EDGE('',*,*,#18056,.T.);
#22935=ORIENTED_EDGE('',*,*,#18057,.F.);
#22936=ORIENTED_EDGE('',*,*,#18058,.T.);
#22937=ORIENTED_EDGE('',*,*,#18059,.F.);
#22938=ORIENTED_EDGE('',*,*,#18060,.T.);
#22939=ORIENTED_EDGE('',*,*,#18061,.F.);
#22940=ORIENTED_EDGE('',*,*,#18062,.T.);
#22941=ORIENTED_EDGE('',*,*,#18063,.F.);
#22942=ORIENTED_EDGE('',*,*,#18064,.T.);
#22943=ORIENTED_EDGE('',*,*,#18065,.F.);
#22944=ORIENTED_EDGE('',*,*,#18066,.T.);
#22945=ORIENTED_EDGE('',*,*,#18067,.F.);
#22946=ORIENTED_EDGE('',*,*,#18068,.T.);
#22947=ORIENTED_EDGE('',*,*,#18069,.F.);
#22948=ORIENTED_EDGE('',*,*,#18070,.T.);
#22949=ORIENTED_EDGE('',*,*,#18071,.F.);
#22950=ORIENTED_EDGE('',*,*,#18072,.T.);
#22951=ORIENTED_EDGE('',*,*,#18073,.F.);
#22952=ORIENTED_EDGE('',*,*,#18074,.T.);
#22953=ORIENTED_EDGE('',*,*,#18075,.F.);
#22954=ORIENTED_EDGE('',*,*,#18076,.T.);
#22955=ORIENTED_EDGE('',*,*,#18077,.F.);
#22956=ORIENTED_EDGE('',*,*,#18078,.T.);
#22957=ORIENTED_EDGE('',*,*,#18079,.F.);
#22958=ORIENTED_EDGE('',*,*,#18080,.T.);
#22959=ORIENTED_EDGE('',*,*,#18081,.F.);
#22960=ORIENTED_EDGE('',*,*,#18082,.T.);
#22961=ORIENTED_EDGE('',*,*,#18083,.F.);
#22962=ORIENTED_EDGE('',*,*,#18084,.T.);
#22963=ORIENTED_EDGE('',*,*,#18085,.F.);
#22964=ORIENTED_EDGE('',*,*,#18086,.T.);
#22965=ORIENTED_EDGE('',*,*,#18087,.F.);
#22966=ORIENTED_EDGE('',*,*,#18088,.T.);
#22967=ORIENTED_EDGE('',*,*,#18089,.F.);
#22968=ORIENTED_EDGE('',*,*,#18090,.T.);
#22969=ORIENTED_EDGE('',*,*,#18091,.F.);
#22970=ORIENTED_EDGE('',*,*,#18092,.T.);
#22971=ORIENTED_EDGE('',*,*,#18093,.T.);
#22972=ORIENTED_EDGE('',*,*,#18094,.T.);
#22973=ORIENTED_EDGE('',*,*,#18095,.F.);
#22974=ORIENTED_EDGE('',*,*,#18096,.T.);
#22975=ORIENTED_EDGE('',*,*,#18097,.T.);
#22976=ORIENTED_EDGE('',*,*,#18098,.T.);
#22977=ORIENTED_EDGE('',*,*,#18093,.F.);
#22978=ORIENTED_EDGE('',*,*,#18099,.T.);
#22979=ORIENTED_EDGE('',*,*,#18100,.T.);
#22980=ORIENTED_EDGE('',*,*,#18101,.T.);
#22981=ORIENTED_EDGE('',*,*,#18097,.F.);
#22982=ORIENTED_EDGE('',*,*,#18102,.T.);
#22983=ORIENTED_EDGE('',*,*,#18103,.T.);
#22984=ORIENTED_EDGE('',*,*,#18104,.T.);
#22985=ORIENTED_EDGE('',*,*,#18100,.F.);
#22986=ORIENTED_EDGE('',*,*,#18105,.T.);
#22987=ORIENTED_EDGE('',*,*,#18106,.T.);
#22988=ORIENTED_EDGE('',*,*,#18107,.T.);
#22989=ORIENTED_EDGE('',*,*,#18103,.F.);
#22990=ORIENTED_EDGE('',*,*,#18108,.T.);
#22991=ORIENTED_EDGE('',*,*,#18109,.T.);
#22992=ORIENTED_EDGE('',*,*,#18110,.T.);
#22993=ORIENTED_EDGE('',*,*,#18106,.F.);
#22994=ORIENTED_EDGE('',*,*,#18111,.T.);
#22995=ORIENTED_EDGE('',*,*,#18109,.F.);
#22996=ORIENTED_EDGE('',*,*,#18112,.T.);
#22997=ORIENTED_EDGE('',*,*,#18113,.T.);
#22998=ORIENTED_EDGE('',*,*,#18114,.T.);
#22999=ORIENTED_EDGE('',*,*,#18113,.F.);
#23000=ORIENTED_EDGE('',*,*,#18115,.T.);
#23001=ORIENTED_EDGE('',*,*,#18116,.T.);
#23002=ORIENTED_EDGE('',*,*,#18117,.T.);
#23003=ORIENTED_EDGE('',*,*,#18116,.F.);
#23004=ORIENTED_EDGE('',*,*,#18118,.T.);
#23005=ORIENTED_EDGE('',*,*,#18119,.T.);
#23006=ORIENTED_EDGE('',*,*,#18120,.T.);
#23007=ORIENTED_EDGE('',*,*,#18119,.F.);
#23008=ORIENTED_EDGE('',*,*,#18121,.T.);
#23009=ORIENTED_EDGE('',*,*,#18095,.T.);
#23010=ORIENTED_EDGE('',*,*,#18110,.F.);
#23011=ORIENTED_EDGE('',*,*,#18122,.F.);
#23012=ORIENTED_EDGE('',*,*,#18123,.F.);
#23013=ORIENTED_EDGE('',*,*,#18124,.T.);
#23014=ORIENTED_EDGE('',*,*,#18111,.F.);
#23015=ORIENTED_EDGE('',*,*,#18125,.F.);
#23016=ORIENTED_EDGE('',*,*,#18126,.F.);
#23017=ORIENTED_EDGE('',*,*,#18122,.T.);
#23018=ORIENTED_EDGE('',*,*,#18114,.F.);
#23019=ORIENTED_EDGE('',*,*,#18127,.F.);
#23020=ORIENTED_EDGE('',*,*,#18128,.F.);
#23021=ORIENTED_EDGE('',*,*,#18125,.T.);
#23022=ORIENTED_EDGE('',*,*,#18117,.F.);
#23023=ORIENTED_EDGE('',*,*,#18129,.F.);
#23024=ORIENTED_EDGE('',*,*,#18130,.F.);
#23025=ORIENTED_EDGE('',*,*,#18127,.T.);
#23026=ORIENTED_EDGE('',*,*,#18120,.F.);
#23027=ORIENTED_EDGE('',*,*,#18131,.F.);
#23028=ORIENTED_EDGE('',*,*,#18132,.F.);
#23029=ORIENTED_EDGE('',*,*,#18129,.T.);
#23030=ORIENTED_EDGE('',*,*,#18094,.F.);
#23031=ORIENTED_EDGE('',*,*,#18133,.F.);
#23032=ORIENTED_EDGE('',*,*,#18134,.F.);
#23033=ORIENTED_EDGE('',*,*,#18131,.T.);
#23034=ORIENTED_EDGE('',*,*,#18108,.F.);
#23035=ORIENTED_EDGE('',*,*,#18105,.F.);
#23036=ORIENTED_EDGE('',*,*,#18102,.F.);
#23037=ORIENTED_EDGE('',*,*,#18099,.F.);
#23038=ORIENTED_EDGE('',*,*,#18096,.F.);
#23039=ORIENTED_EDGE('',*,*,#18092,.F.);
#23040=ORIENTED_EDGE('',*,*,#18121,.F.);
#23041=ORIENTED_EDGE('',*,*,#18118,.F.);
#23042=ORIENTED_EDGE('',*,*,#18115,.F.);
#23043=ORIENTED_EDGE('',*,*,#18112,.F.);
#23044=ORIENTED_EDGE('',*,*,#18135,.T.);
#23045=ORIENTED_EDGE('',*,*,#18136,.T.);
#23046=ORIENTED_EDGE('',*,*,#18137,.T.);
#23047=ORIENTED_EDGE('',*,*,#18138,.T.);
#23048=ORIENTED_EDGE('',*,*,#18139,.T.);
#23049=ORIENTED_EDGE('',*,*,#17485,.F.);
#23050=ORIENTED_EDGE('',*,*,#18140,.T.);
#23051=ORIENTED_EDGE('',*,*,#18141,.T.);
#23052=ORIENTED_EDGE('',*,*,#17529,.T.);
#23053=ORIENTED_EDGE('',*,*,#18142,.T.);
#23054=ORIENTED_EDGE('',*,*,#18143,.T.);
#23055=ORIENTED_EDGE('',*,*,#18141,.F.);
#23056=ORIENTED_EDGE('',*,*,#18144,.F.);
#23057=ORIENTED_EDGE('',*,*,#18145,.F.);
#23058=ORIENTED_EDGE('',*,*,#17530,.F.);
#23059=ORIENTED_EDGE('',*,*,#18140,.F.);
#23060=ORIENTED_EDGE('',*,*,#18146,.F.);
#23061=ORIENTED_EDGE('',*,*,#18147,.T.);
#23062=ORIENTED_EDGE('',*,*,#18148,.T.);
#23063=ORIENTED_EDGE('',*,*,#18144,.T.);
#23064=ORIENTED_EDGE('',*,*,#18143,.F.);
#23065=ORIENTED_EDGE('',*,*,#18149,.T.);
#23066=ORIENTED_EDGE('',*,*,#18150,.T.);
#23067=ORIENTED_EDGE('',*,*,#18151,.T.);
#23068=ORIENTED_EDGE('',*,*,#18146,.T.);
#23069=ORIENTED_EDGE('',*,*,#18148,.F.);
#23070=ORIENTED_EDGE('',*,*,#18152,.F.);
#23071=ORIENTED_EDGE('',*,*,#18153,.F.);
#23072=ORIENTED_EDGE('',*,*,#18150,.F.);
#23073=ORIENTED_EDGE('',*,*,#18154,.F.);
#23074=ORIENTED_EDGE('',*,*,#18155,.F.);
#23075=ORIENTED_EDGE('',*,*,#17527,.T.);
#23076=ORIENTED_EDGE('',*,*,#18156,.T.);
#23077=ORIENTED_EDGE('',*,*,#18154,.T.);
#23078=ORIENTED_EDGE('',*,*,#18157,.T.);
#23079=ORIENTED_EDGE('',*,*,#18158,.F.);
#23080=ORIENTED_EDGE('',*,*,#18159,.F.);
#23081=ORIENTED_EDGE('',*,*,#18160,.F.);
#23082=ORIENTED_EDGE('',*,*,#17525,.T.);
#23083=ORIENTED_EDGE('',*,*,#18161,.T.);
#23084=ORIENTED_EDGE('',*,*,#18159,.T.);
#23085=ORIENTED_EDGE('',*,*,#18162,.T.);
#23086=ORIENTED_EDGE('',*,*,#18152,.T.);
#23087=ORIENTED_EDGE('',*,*,#18163,.T.);
#23088=ORIENTED_EDGE('',*,*,#18160,.T.);
#23089=ORIENTED_EDGE('',*,*,#18164,.T.);
#23090=ORIENTED_EDGE('',*,*,#18158,.T.);
#23091=ORIENTED_EDGE('',*,*,#18165,.T.);
#23092=ORIENTED_EDGE('',*,*,#18155,.T.);
#23093=ORIENTED_EDGE('',*,*,#18166,.T.);
#23094=ORIENTED_EDGE('',*,*,#17531,.T.);
#23095=ORIENTED_EDGE('',*,*,#18145,.T.);
#23096=ORIENTED_EDGE('',*,*,#18153,.T.);
#23097=ORIENTED_EDGE('',*,*,#18167,.T.);
#23098=ORIENTED_EDGE('',*,*,#18142,.F.);
#23099=ORIENTED_EDGE('',*,*,#17528,.F.);
#23100=ORIENTED_EDGE('',*,*,#18157,.F.);
#23101=ORIENTED_EDGE('',*,*,#18149,.F.);
#23102=ORIENTED_EDGE('',*,*,#18163,.F.);
#23103=ORIENTED_EDGE('',*,*,#18147,.F.);
#23104=ORIENTED_EDGE('',*,*,#18151,.F.);
#23105=ORIENTED_EDGE('',*,*,#18165,.F.);
#23106=ORIENTED_EDGE('',*,*,#18168,.F.);
#23107=ORIENTED_EDGE('',*,*,#18169,.F.);
#23108=ORIENTED_EDGE('',*,*,#18170,.F.);
#23109=ORIENTED_EDGE('',*,*,#18171,.F.);
#23110=ORIENTED_EDGE('',*,*,#18172,.F.);
#23111=ORIENTED_EDGE('',*,*,#18173,.F.);
#23112=ORIENTED_EDGE('',*,*,#18174,.F.);
#23113=ORIENTED_EDGE('',*,*,#18175,.F.);
#23114=ORIENTED_EDGE('',*,*,#18176,.F.);
#23115=ORIENTED_EDGE('',*,*,#17535,.T.);
#23116=ORIENTED_EDGE('',*,*,#18177,.T.);
#23117=ORIENTED_EDGE('',*,*,#18175,.T.);
#23118=ORIENTED_EDGE('',*,*,#18178,.T.);
#23119=ORIENTED_EDGE('',*,*,#18179,.F.);
#23120=ORIENTED_EDGE('',*,*,#18180,.F.);
#23121=ORIENTED_EDGE('',*,*,#18181,.F.);
#23122=ORIENTED_EDGE('',*,*,#17533,.T.);
#23123=ORIENTED_EDGE('',*,*,#18182,.T.);
#23124=ORIENTED_EDGE('',*,*,#18180,.T.);
#23125=ORIENTED_EDGE('',*,*,#18183,.T.);
#23126=ORIENTED_EDGE('',*,*,#18172,.T.);
#23127=ORIENTED_EDGE('',*,*,#18184,.T.);
#23128=ORIENTED_EDGE('',*,*,#18181,.T.);
#23129=ORIENTED_EDGE('',*,*,#18185,.T.);
#23130=ORIENTED_EDGE('',*,*,#18179,.T.);
#23131=ORIENTED_EDGE('',*,*,#18186,.T.);
#23132=ORIENTED_EDGE('',*,*,#18176,.T.);
#23133=ORIENTED_EDGE('',*,*,#18187,.T.);
#23134=ORIENTED_EDGE('',*,*,#18169,.T.);
#23135=ORIENTED_EDGE('',*,*,#18188,.T.);
#23136=ORIENTED_EDGE('',*,*,#18174,.T.);
#23137=ORIENTED_EDGE('',*,*,#18189,.T.);
#23138=ORIENTED_EDGE('',*,*,#17539,.T.);
#23139=ORIENTED_EDGE('',*,*,#18190,.T.);
#23140=ORIENTED_EDGE('',*,*,#18173,.T.);
#23141=ORIENTED_EDGE('',*,*,#18191,.T.);
#23142=ORIENTED_EDGE('',*,*,#18171,.T.);
#23143=ORIENTED_EDGE('',*,*,#18192,.T.);
#23144=ORIENTED_EDGE('',*,*,#18170,.T.);
#23145=ORIENTED_EDGE('',*,*,#18193,.T.);
#23146=ORIENTED_EDGE('',*,*,#17537,.T.);
#23147=ORIENTED_EDGE('',*,*,#18194,.T.);
#23148=ORIENTED_EDGE('',*,*,#18168,.T.);
#23149=ORIENTED_EDGE('',*,*,#18195,.T.);
#23150=ORIENTED_EDGE('',*,*,#18183,.F.);
#23151=ORIENTED_EDGE('',*,*,#18187,.F.);
#23152=ORIENTED_EDGE('',*,*,#18177,.F.);
#23153=ORIENTED_EDGE('',*,*,#17534,.F.);
#23154=ORIENTED_EDGE('',*,*,#18178,.F.);
#23155=ORIENTED_EDGE('',*,*,#18188,.F.);
#23156=ORIENTED_EDGE('',*,*,#18194,.F.);
#23157=ORIENTED_EDGE('',*,*,#17536,.F.);
#23158=ORIENTED_EDGE('',*,*,#18184,.F.);
#23159=ORIENTED_EDGE('',*,*,#18193,.F.);
#23160=ORIENTED_EDGE('',*,*,#18189,.F.);
#23161=ORIENTED_EDGE('',*,*,#18186,.F.);
#23162=ORIENTED_EDGE('',*,*,#18196,.F.);
#23163=ORIENTED_EDGE('',*,*,#18197,.F.);
#23164=ORIENTED_EDGE('',*,*,#18198,.F.);
#23165=ORIENTED_EDGE('',*,*,#18199,.T.);
#23166=ORIENTED_EDGE('',*,*,#18200,.T.);
#23167=ORIENTED_EDGE('',*,*,#18197,.T.);
#23168=ORIENTED_EDGE('',*,*,#18201,.T.);
#23169=ORIENTED_EDGE('',*,*,#18202,.T.);
#23170=ORIENTED_EDGE('',*,*,#17547,.T.);
#23171=ORIENTED_EDGE('',*,*,#18203,.T.);
#23172=ORIENTED_EDGE('',*,*,#18198,.T.);
#23173=ORIENTED_EDGE('',*,*,#18204,.T.);
#23174=ORIENTED_EDGE('',*,*,#18205,.F.);
#23175=ORIENTED_EDGE('',*,*,#18206,.F.);
#23176=ORIENTED_EDGE('',*,*,#18207,.F.);
#23177=ORIENTED_EDGE('',*,*,#18208,.T.);
#23178=ORIENTED_EDGE('',*,*,#18209,.T.);
#23179=ORIENTED_EDGE('',*,*,#18206,.T.);
#23180=ORIENTED_EDGE('',*,*,#18210,.T.);
#23181=ORIENTED_EDGE('',*,*,#18211,.T.);
#23182=ORIENTED_EDGE('',*,*,#18196,.T.);
#23183=ORIENTED_EDGE('',*,*,#18212,.T.);
#23184=ORIENTED_EDGE('',*,*,#18207,.T.);
#23185=ORIENTED_EDGE('',*,*,#18213,.T.);
#23186=ORIENTED_EDGE('',*,*,#17545,.T.);
#23187=ORIENTED_EDGE('',*,*,#18214,.T.);
#23188=ORIENTED_EDGE('',*,*,#18205,.T.);
#23189=ORIENTED_EDGE('',*,*,#18215,.T.);
#23190=ORIENTED_EDGE('',*,*,#18199,.F.);
#23191=ORIENTED_EDGE('',*,*,#18216,.T.);
#23192=ORIENTED_EDGE('',*,*,#18217,.T.);
#23193=ORIENTED_EDGE('',*,*,#17541,.T.);
#23194=ORIENTED_EDGE('',*,*,#18218,.T.);
#23195=ORIENTED_EDGE('',*,*,#18201,.F.);
#23196=ORIENTED_EDGE('',*,*,#18213,.F.);
#23197=ORIENTED_EDGE('',*,*,#18209,.F.);
#23198=ORIENTED_EDGE('',*,*,#18219,.F.);
#23199=ORIENTED_EDGE('',*,*,#18202,.F.);
#23200=ORIENTED_EDGE('',*,*,#18219,.T.);
#23201=ORIENTED_EDGE('',*,*,#18208,.F.);
#23202=ORIENTED_EDGE('',*,*,#18220,.F.);
#23203=ORIENTED_EDGE('',*,*,#18221,.T.);
#23204=ORIENTED_EDGE('',*,*,#18216,.F.);
#23205=ORIENTED_EDGE('',*,*,#18211,.F.);
#23206=ORIENTED_EDGE('',*,*,#18222,.T.);
#23207=ORIENTED_EDGE('',*,*,#17543,.T.);
#23208=ORIENTED_EDGE('',*,*,#18223,.T.);
#23209=ORIENTED_EDGE('',*,*,#18220,.T.);
#23210=ORIENTED_EDGE('',*,*,#18210,.F.);
#23211=ORIENTED_EDGE('',*,*,#18214,.F.);
#23212=ORIENTED_EDGE('',*,*,#17544,.F.);
#23213=ORIENTED_EDGE('',*,*,#18222,.F.);
#23214=ORIENTED_EDGE('',*,*,#18200,.F.);
#23215=ORIENTED_EDGE('',*,*,#18218,.F.);
#23216=ORIENTED_EDGE('',*,*,#17540,.F.);
#23217=ORIENTED_EDGE('',*,*,#18204,.F.);
#23218=ORIENTED_EDGE('',*,*,#18224,.F.);
#23219=ORIENTED_EDGE('',*,*,#18225,.F.);
#23220=ORIENTED_EDGE('',*,*,#18226,.F.);
#23221=ORIENTED_EDGE('',*,*,#18227,.F.);
#23222=ORIENTED_EDGE('',*,*,#18228,.F.);
#23223=ORIENTED_EDGE('',*,*,#18229,.F.);
#23224=ORIENTED_EDGE('',*,*,#18230,.F.);
#23225=ORIENTED_EDGE('',*,*,#18231,.F.);
#23226=ORIENTED_EDGE('',*,*,#18232,.F.);
#23227=ORIENTED_EDGE('',*,*,#17551,.T.);
#23228=ORIENTED_EDGE('',*,*,#18233,.T.);
#23229=ORIENTED_EDGE('',*,*,#18231,.T.);
#23230=ORIENTED_EDGE('',*,*,#18234,.T.);
#23231=ORIENTED_EDGE('',*,*,#18235,.F.);
#23232=ORIENTED_EDGE('',*,*,#18236,.F.);
#23233=ORIENTED_EDGE('',*,*,#18237,.F.);
#23234=ORIENTED_EDGE('',*,*,#17549,.T.);
#23235=ORIENTED_EDGE('',*,*,#18238,.T.);
#23236=ORIENTED_EDGE('',*,*,#18236,.T.);
#23237=ORIENTED_EDGE('',*,*,#18239,.T.);
#23238=ORIENTED_EDGE('',*,*,#18228,.T.);
#23239=ORIENTED_EDGE('',*,*,#18240,.T.);
#23240=ORIENTED_EDGE('',*,*,#18237,.T.);
#23241=ORIENTED_EDGE('',*,*,#18241,.T.);
#23242=ORIENTED_EDGE('',*,*,#18235,.T.);
#23243=ORIENTED_EDGE('',*,*,#18242,.T.);
#23244=ORIENTED_EDGE('',*,*,#18232,.T.);
#23245=ORIENTED_EDGE('',*,*,#18243,.T.);
#23246=ORIENTED_EDGE('',*,*,#18225,.T.);
#23247=ORIENTED_EDGE('',*,*,#18244,.T.);
#23248=ORIENTED_EDGE('',*,*,#18230,.T.);
#23249=ORIENTED_EDGE('',*,*,#18245,.T.);
#23250=ORIENTED_EDGE('',*,*,#17555,.T.);
#23251=ORIENTED_EDGE('',*,*,#18246,.T.);
#23252=ORIENTED_EDGE('',*,*,#18229,.T.);
#23253=ORIENTED_EDGE('',*,*,#18247,.T.);
#23254=ORIENTED_EDGE('',*,*,#18227,.T.);
#23255=ORIENTED_EDGE('',*,*,#18248,.T.);
#23256=ORIENTED_EDGE('',*,*,#18226,.T.);
#23257=ORIENTED_EDGE('',*,*,#18249,.T.);
#23258=ORIENTED_EDGE('',*,*,#17553,.T.);
#23259=ORIENTED_EDGE('',*,*,#18250,.T.);
#23260=ORIENTED_EDGE('',*,*,#18224,.T.);
#23261=ORIENTED_EDGE('',*,*,#18251,.T.);
#23262=ORIENTED_EDGE('',*,*,#18239,.F.);
#23263=ORIENTED_EDGE('',*,*,#18243,.F.);
#23264=ORIENTED_EDGE('',*,*,#18233,.F.);
#23265=ORIENTED_EDGE('',*,*,#17550,.F.);
#23266=ORIENTED_EDGE('',*,*,#18234,.F.);
#23267=ORIENTED_EDGE('',*,*,#18244,.F.);
#23268=ORIENTED_EDGE('',*,*,#18250,.F.);
#23269=ORIENTED_EDGE('',*,*,#17552,.F.);
#23270=ORIENTED_EDGE('',*,*,#18240,.F.);
#23271=ORIENTED_EDGE('',*,*,#18249,.F.);
#23272=ORIENTED_EDGE('',*,*,#18245,.F.);
#23273=ORIENTED_EDGE('',*,*,#18242,.F.);
#23274=ORIENTED_EDGE('',*,*,#18252,.F.);
#23275=ORIENTED_EDGE('',*,*,#18253,.F.);
#23276=ORIENTED_EDGE('',*,*,#18254,.F.);
#23277=ORIENTED_EDGE('',*,*,#18255,.F.);
#23278=ORIENTED_EDGE('',*,*,#18256,.F.);
#23279=ORIENTED_EDGE('',*,*,#18257,.F.);
#23280=ORIENTED_EDGE('',*,*,#18258,.F.);
#23281=ORIENTED_EDGE('',*,*,#18259,.F.);
#23282=ORIENTED_EDGE('',*,*,#18260,.F.);
#23283=ORIENTED_EDGE('',*,*,#17559,.T.);
#23284=ORIENTED_EDGE('',*,*,#18261,.T.);
#23285=ORIENTED_EDGE('',*,*,#18259,.T.);
#23286=ORIENTED_EDGE('',*,*,#18262,.T.);
#23287=ORIENTED_EDGE('',*,*,#18263,.F.);
#23288=ORIENTED_EDGE('',*,*,#18264,.F.);
#23289=ORIENTED_EDGE('',*,*,#18265,.F.);
#23290=ORIENTED_EDGE('',*,*,#17557,.T.);
#23291=ORIENTED_EDGE('',*,*,#18266,.T.);
#23292=ORIENTED_EDGE('',*,*,#18264,.T.);
#23293=ORIENTED_EDGE('',*,*,#18267,.T.);
#23294=ORIENTED_EDGE('',*,*,#18256,.T.);
#23295=ORIENTED_EDGE('',*,*,#18268,.T.);
#23296=ORIENTED_EDGE('',*,*,#18265,.T.);
#23297=ORIENTED_EDGE('',*,*,#18269,.T.);
#23298=ORIENTED_EDGE('',*,*,#18263,.T.);
#23299=ORIENTED_EDGE('',*,*,#18270,.T.);
#23300=ORIENTED_EDGE('',*,*,#18260,.T.);
#23301=ORIENTED_EDGE('',*,*,#18271,.T.);
#23302=ORIENTED_EDGE('',*,*,#18253,.T.);
#23303=ORIENTED_EDGE('',*,*,#18272,.T.);
#23304=ORIENTED_EDGE('',*,*,#18258,.T.);
#23305=ORIENTED_EDGE('',*,*,#18273,.T.);
#23306=ORIENTED_EDGE('',*,*,#17563,.T.);
#23307=ORIENTED_EDGE('',*,*,#18274,.T.);
#23308=ORIENTED_EDGE('',*,*,#18257,.T.);
#23309=ORIENTED_EDGE('',*,*,#18275,.T.);
#23310=ORIENTED_EDGE('',*,*,#18255,.T.);
#23311=ORIENTED_EDGE('',*,*,#18276,.T.);
#23312=ORIENTED_EDGE('',*,*,#18254,.T.);
#23313=ORIENTED_EDGE('',*,*,#18277,.T.);
#23314=ORIENTED_EDGE('',*,*,#17561,.T.);
#23315=ORIENTED_EDGE('',*,*,#18278,.T.);
#23316=ORIENTED_EDGE('',*,*,#18252,.T.);
#23317=ORIENTED_EDGE('',*,*,#18279,.T.);
#23318=ORIENTED_EDGE('',*,*,#18267,.F.);
#23319=ORIENTED_EDGE('',*,*,#18271,.F.);
#23320=ORIENTED_EDGE('',*,*,#18261,.F.);
#23321=ORIENTED_EDGE('',*,*,#17558,.F.);
#23322=ORIENTED_EDGE('',*,*,#18262,.F.);
#23323=ORIENTED_EDGE('',*,*,#18272,.F.);
#23324=ORIENTED_EDGE('',*,*,#18278,.F.);
#23325=ORIENTED_EDGE('',*,*,#17560,.F.);
#23326=ORIENTED_EDGE('',*,*,#18268,.F.);
#23327=ORIENTED_EDGE('',*,*,#18277,.F.);
#23328=ORIENTED_EDGE('',*,*,#18273,.F.);
#23329=ORIENTED_EDGE('',*,*,#18270,.F.);
#23330=ORIENTED_EDGE('',*,*,#18280,.T.);
#23331=ORIENTED_EDGE('',*,*,#18281,.T.);
#23332=ORIENTED_EDGE('',*,*,#17569,.T.);
#23333=ORIENTED_EDGE('',*,*,#18282,.T.);
#23334=ORIENTED_EDGE('',*,*,#18283,.T.);
#23335=ORIENTED_EDGE('',*,*,#18281,.F.);
#23336=ORIENTED_EDGE('',*,*,#18284,.F.);
#23337=ORIENTED_EDGE('',*,*,#18285,.F.);
#23338=ORIENTED_EDGE('',*,*,#17570,.F.);
#23339=ORIENTED_EDGE('',*,*,#18280,.F.);
#23340=ORIENTED_EDGE('',*,*,#18286,.F.);
#23341=ORIENTED_EDGE('',*,*,#18287,.T.);
#23342=ORIENTED_EDGE('',*,*,#18288,.T.);
#23343=ORIENTED_EDGE('',*,*,#18284,.T.);
#23344=ORIENTED_EDGE('',*,*,#18283,.F.);
#23345=ORIENTED_EDGE('',*,*,#18289,.T.);
#23346=ORIENTED_EDGE('',*,*,#18290,.T.);
#23347=ORIENTED_EDGE('',*,*,#18291,.T.);
#23348=ORIENTED_EDGE('',*,*,#18286,.T.);
#23349=ORIENTED_EDGE('',*,*,#18288,.F.);
#23350=ORIENTED_EDGE('',*,*,#18292,.F.);
#23351=ORIENTED_EDGE('',*,*,#18293,.F.);
#23352=ORIENTED_EDGE('',*,*,#18290,.F.);
#23353=ORIENTED_EDGE('',*,*,#18294,.F.);
#23354=ORIENTED_EDGE('',*,*,#18295,.F.);
#23355=ORIENTED_EDGE('',*,*,#17567,.T.);
#23356=ORIENTED_EDGE('',*,*,#18296,.T.);
#23357=ORIENTED_EDGE('',*,*,#18294,.T.);
#23358=ORIENTED_EDGE('',*,*,#18297,.T.);
#23359=ORIENTED_EDGE('',*,*,#18298,.F.);
#23360=ORIENTED_EDGE('',*,*,#18299,.F.);
#23361=ORIENTED_EDGE('',*,*,#18300,.F.);
#23362=ORIENTED_EDGE('',*,*,#17565,.T.);
#23363=ORIENTED_EDGE('',*,*,#18301,.T.);
#23364=ORIENTED_EDGE('',*,*,#18299,.T.);
#23365=ORIENTED_EDGE('',*,*,#18302,.T.);
#23366=ORIENTED_EDGE('',*,*,#18292,.T.);
#23367=ORIENTED_EDGE('',*,*,#18303,.T.);
#23368=ORIENTED_EDGE('',*,*,#18300,.T.);
#23369=ORIENTED_EDGE('',*,*,#18304,.T.);
#23370=ORIENTED_EDGE('',*,*,#18298,.T.);
#23371=ORIENTED_EDGE('',*,*,#18305,.T.);
#23372=ORIENTED_EDGE('',*,*,#18295,.T.);
#23373=ORIENTED_EDGE('',*,*,#18306,.T.);
#23374=ORIENTED_EDGE('',*,*,#17571,.T.);
#23375=ORIENTED_EDGE('',*,*,#18285,.T.);
#23376=ORIENTED_EDGE('',*,*,#18293,.T.);
#23377=ORIENTED_EDGE('',*,*,#18307,.T.);
#23378=ORIENTED_EDGE('',*,*,#18282,.F.);
#23379=ORIENTED_EDGE('',*,*,#17568,.F.);
#23380=ORIENTED_EDGE('',*,*,#18297,.F.);
#23381=ORIENTED_EDGE('',*,*,#18289,.F.);
#23382=ORIENTED_EDGE('',*,*,#18303,.F.);
#23383=ORIENTED_EDGE('',*,*,#18287,.F.);
#23384=ORIENTED_EDGE('',*,*,#18291,.F.);
#23385=ORIENTED_EDGE('',*,*,#18305,.F.);
#23386=ORIENTED_EDGE('',*,*,#18308,.F.);
#23387=ORIENTED_EDGE('',*,*,#18309,.F.);
#23388=ORIENTED_EDGE('',*,*,#18310,.F.);
#23389=ORIENTED_EDGE('',*,*,#18311,.F.);
#23390=ORIENTED_EDGE('',*,*,#18312,.F.);
#23391=ORIENTED_EDGE('',*,*,#18313,.F.);
#23392=ORIENTED_EDGE('',*,*,#18314,.F.);
#23393=ORIENTED_EDGE('',*,*,#18315,.F.);
#23394=ORIENTED_EDGE('',*,*,#18316,.F.);
#23395=ORIENTED_EDGE('',*,*,#17575,.T.);
#23396=ORIENTED_EDGE('',*,*,#18317,.T.);
#23397=ORIENTED_EDGE('',*,*,#18315,.T.);
#23398=ORIENTED_EDGE('',*,*,#18318,.T.);
#23399=ORIENTED_EDGE('',*,*,#18319,.F.);
#23400=ORIENTED_EDGE('',*,*,#18320,.F.);
#23401=ORIENTED_EDGE('',*,*,#18321,.F.);
#23402=ORIENTED_EDGE('',*,*,#17573,.T.);
#23403=ORIENTED_EDGE('',*,*,#18322,.T.);
#23404=ORIENTED_EDGE('',*,*,#18320,.T.);
#23405=ORIENTED_EDGE('',*,*,#18323,.T.);
#23406=ORIENTED_EDGE('',*,*,#18312,.T.);
#23407=ORIENTED_EDGE('',*,*,#18324,.T.);
#23408=ORIENTED_EDGE('',*,*,#18321,.T.);
#23409=ORIENTED_EDGE('',*,*,#18325,.T.);
#23410=ORIENTED_EDGE('',*,*,#18319,.T.);
#23411=ORIENTED_EDGE('',*,*,#18326,.T.);
#23412=ORIENTED_EDGE('',*,*,#18316,.T.);
#23413=ORIENTED_EDGE('',*,*,#18327,.T.);
#23414=ORIENTED_EDGE('',*,*,#18309,.T.);
#23415=ORIENTED_EDGE('',*,*,#18328,.T.);
#23416=ORIENTED_EDGE('',*,*,#18314,.T.);
#23417=ORIENTED_EDGE('',*,*,#18329,.T.);
#23418=ORIENTED_EDGE('',*,*,#17579,.T.);
#23419=ORIENTED_EDGE('',*,*,#18330,.T.);
#23420=ORIENTED_EDGE('',*,*,#18313,.T.);
#23421=ORIENTED_EDGE('',*,*,#18331,.T.);
#23422=ORIENTED_EDGE('',*,*,#18311,.T.);
#23423=ORIENTED_EDGE('',*,*,#18332,.T.);
#23424=ORIENTED_EDGE('',*,*,#18310,.T.);
#23425=ORIENTED_EDGE('',*,*,#18333,.T.);
#23426=ORIENTED_EDGE('',*,*,#17577,.T.);
#23427=ORIENTED_EDGE('',*,*,#18334,.T.);
#23428=ORIENTED_EDGE('',*,*,#18308,.T.);
#23429=ORIENTED_EDGE('',*,*,#18335,.T.);
#23430=ORIENTED_EDGE('',*,*,#18323,.F.);
#23431=ORIENTED_EDGE('',*,*,#18327,.F.);
#23432=ORIENTED_EDGE('',*,*,#18317,.F.);
#23433=ORIENTED_EDGE('',*,*,#17574,.F.);
#23434=ORIENTED_EDGE('',*,*,#18318,.F.);
#23435=ORIENTED_EDGE('',*,*,#18328,.F.);
#23436=ORIENTED_EDGE('',*,*,#18334,.F.);
#23437=ORIENTED_EDGE('',*,*,#17576,.F.);
#23438=ORIENTED_EDGE('',*,*,#18324,.F.);
#23439=ORIENTED_EDGE('',*,*,#18333,.F.);
#23440=ORIENTED_EDGE('',*,*,#18329,.F.);
#23441=ORIENTED_EDGE('',*,*,#18326,.F.);
#23442=ORIENTED_EDGE('',*,*,#18336,.F.);
#23443=ORIENTED_EDGE('',*,*,#18337,.F.);
#23444=ORIENTED_EDGE('',*,*,#18338,.F.);
#23445=ORIENTED_EDGE('',*,*,#18339,.T.);
#23446=ORIENTED_EDGE('',*,*,#18340,.T.);
#23447=ORIENTED_EDGE('',*,*,#18337,.T.);
#23448=ORIENTED_EDGE('',*,*,#18341,.T.);
#23449=ORIENTED_EDGE('',*,*,#18342,.T.);
#23450=ORIENTED_EDGE('',*,*,#17587,.T.);
#23451=ORIENTED_EDGE('',*,*,#18343,.T.);
#23452=ORIENTED_EDGE('',*,*,#18338,.T.);
#23453=ORIENTED_EDGE('',*,*,#18344,.T.);
#23454=ORIENTED_EDGE('',*,*,#18345,.F.);
#23455=ORIENTED_EDGE('',*,*,#18346,.F.);
#23456=ORIENTED_EDGE('',*,*,#18347,.F.);
#23457=ORIENTED_EDGE('',*,*,#18348,.T.);
#23458=ORIENTED_EDGE('',*,*,#18349,.T.);
#23459=ORIENTED_EDGE('',*,*,#18346,.T.);
#23460=ORIENTED_EDGE('',*,*,#18350,.T.);
#23461=ORIENTED_EDGE('',*,*,#18351,.T.);
#23462=ORIENTED_EDGE('',*,*,#18336,.T.);
#23463=ORIENTED_EDGE('',*,*,#18352,.T.);
#23464=ORIENTED_EDGE('',*,*,#18347,.T.);
#23465=ORIENTED_EDGE('',*,*,#18353,.T.);
#23466=ORIENTED_EDGE('',*,*,#17585,.T.);
#23467=ORIENTED_EDGE('',*,*,#18354,.T.);
#23468=ORIENTED_EDGE('',*,*,#18345,.T.);
#23469=ORIENTED_EDGE('',*,*,#18355,.T.);
#23470=ORIENTED_EDGE('',*,*,#18339,.F.);
#23471=ORIENTED_EDGE('',*,*,#18356,.T.);
#23472=ORIENTED_EDGE('',*,*,#18357,.T.);
#23473=ORIENTED_EDGE('',*,*,#17581,.T.);
#23474=ORIENTED_EDGE('',*,*,#18358,.T.);
#23475=ORIENTED_EDGE('',*,*,#18341,.F.);
#23476=ORIENTED_EDGE('',*,*,#18353,.F.);
#23477=ORIENTED_EDGE('',*,*,#18349,.F.);
#23478=ORIENTED_EDGE('',*,*,#18359,.F.);
#23479=ORIENTED_EDGE('',*,*,#18342,.F.);
#23480=ORIENTED_EDGE('',*,*,#18359,.T.);
#23481=ORIENTED_EDGE('',*,*,#18348,.F.);
#23482=ORIENTED_EDGE('',*,*,#18360,.F.);
#23483=ORIENTED_EDGE('',*,*,#18361,.T.);
#23484=ORIENTED_EDGE('',*,*,#18356,.F.);
#23485=ORIENTED_EDGE('',*,*,#18351,.F.);
#23486=ORIENTED_EDGE('',*,*,#18362,.T.);
#23487=ORIENTED_EDGE('',*,*,#17583,.T.);
#23488=ORIENTED_EDGE('',*,*,#18363,.T.);
#23489=ORIENTED_EDGE('',*,*,#18360,.T.);
#23490=ORIENTED_EDGE('',*,*,#18350,.F.);
#23491=ORIENTED_EDGE('',*,*,#18354,.F.);
#23492=ORIENTED_EDGE('',*,*,#17584,.F.);
#23493=ORIENTED_EDGE('',*,*,#18362,.F.);
#23494=ORIENTED_EDGE('',*,*,#18340,.F.);
#23495=ORIENTED_EDGE('',*,*,#18358,.F.);
#23496=ORIENTED_EDGE('',*,*,#17580,.F.);
#23497=ORIENTED_EDGE('',*,*,#18344,.F.);
#23498=ORIENTED_EDGE('',*,*,#18364,.F.);
#23499=ORIENTED_EDGE('',*,*,#18365,.F.);
#23500=ORIENTED_EDGE('',*,*,#18366,.F.);
#23501=ORIENTED_EDGE('',*,*,#18367,.F.);
#23502=ORIENTED_EDGE('',*,*,#18368,.F.);
#23503=ORIENTED_EDGE('',*,*,#18369,.F.);
#23504=ORIENTED_EDGE('',*,*,#18370,.F.);
#23505=ORIENTED_EDGE('',*,*,#18371,.F.);
#23506=ORIENTED_EDGE('',*,*,#18372,.F.);
#23507=ORIENTED_EDGE('',*,*,#17591,.T.);
#23508=ORIENTED_EDGE('',*,*,#18373,.T.);
#23509=ORIENTED_EDGE('',*,*,#18371,.T.);
#23510=ORIENTED_EDGE('',*,*,#18374,.T.);
#23511=ORIENTED_EDGE('',*,*,#18375,.F.);
#23512=ORIENTED_EDGE('',*,*,#18376,.F.);
#23513=ORIENTED_EDGE('',*,*,#18377,.F.);
#23514=ORIENTED_EDGE('',*,*,#17589,.T.);
#23515=ORIENTED_EDGE('',*,*,#18378,.T.);
#23516=ORIENTED_EDGE('',*,*,#18376,.T.);
#23517=ORIENTED_EDGE('',*,*,#18379,.T.);
#23518=ORIENTED_EDGE('',*,*,#18368,.T.);
#23519=ORIENTED_EDGE('',*,*,#18380,.T.);
#23520=ORIENTED_EDGE('',*,*,#18377,.T.);
#23521=ORIENTED_EDGE('',*,*,#18381,.T.);
#23522=ORIENTED_EDGE('',*,*,#18375,.T.);
#23523=ORIENTED_EDGE('',*,*,#18382,.T.);
#23524=ORIENTED_EDGE('',*,*,#18372,.T.);
#23525=ORIENTED_EDGE('',*,*,#18383,.T.);
#23526=ORIENTED_EDGE('',*,*,#18365,.T.);
#23527=ORIENTED_EDGE('',*,*,#18384,.T.);
#23528=ORIENTED_EDGE('',*,*,#18370,.T.);
#23529=ORIENTED_EDGE('',*,*,#18385,.T.);
#23530=ORIENTED_EDGE('',*,*,#17595,.T.);
#23531=ORIENTED_EDGE('',*,*,#18386,.T.);
#23532=ORIENTED_EDGE('',*,*,#18369,.T.);
#23533=ORIENTED_EDGE('',*,*,#18387,.T.);
#23534=ORIENTED_EDGE('',*,*,#18367,.T.);
#23535=ORIENTED_EDGE('',*,*,#18388,.T.);
#23536=ORIENTED_EDGE('',*,*,#18366,.T.);
#23537=ORIENTED_EDGE('',*,*,#18389,.T.);
#23538=ORIENTED_EDGE('',*,*,#17593,.T.);
#23539=ORIENTED_EDGE('',*,*,#18390,.T.);
#23540=ORIENTED_EDGE('',*,*,#18364,.T.);
#23541=ORIENTED_EDGE('',*,*,#18391,.T.);
#23542=ORIENTED_EDGE('',*,*,#18379,.F.);
#23543=ORIENTED_EDGE('',*,*,#18383,.F.);
#23544=ORIENTED_EDGE('',*,*,#18373,.F.);
#23545=ORIENTED_EDGE('',*,*,#17590,.F.);
#23546=ORIENTED_EDGE('',*,*,#18374,.F.);
#23547=ORIENTED_EDGE('',*,*,#18384,.F.);
#23548=ORIENTED_EDGE('',*,*,#18390,.F.);
#23549=ORIENTED_EDGE('',*,*,#17592,.F.);
#23550=ORIENTED_EDGE('',*,*,#18380,.F.);
#23551=ORIENTED_EDGE('',*,*,#18389,.F.);
#23552=ORIENTED_EDGE('',*,*,#18385,.F.);
#23553=ORIENTED_EDGE('',*,*,#18382,.F.);
#23554=ORIENTED_EDGE('',*,*,#18392,.F.);
#23555=ORIENTED_EDGE('',*,*,#18393,.F.);
#23556=ORIENTED_EDGE('',*,*,#18394,.F.);
#23557=ORIENTED_EDGE('',*,*,#18395,.F.);
#23558=ORIENTED_EDGE('',*,*,#18396,.F.);
#23559=ORIENTED_EDGE('',*,*,#18397,.F.);
#23560=ORIENTED_EDGE('',*,*,#18398,.F.);
#23561=ORIENTED_EDGE('',*,*,#18399,.F.);
#23562=ORIENTED_EDGE('',*,*,#18400,.F.);
#23563=ORIENTED_EDGE('',*,*,#17599,.T.);
#23564=ORIENTED_EDGE('',*,*,#18401,.T.);
#23565=ORIENTED_EDGE('',*,*,#18399,.T.);
#23566=ORIENTED_EDGE('',*,*,#18402,.T.);
#23567=ORIENTED_EDGE('',*,*,#18403,.F.);
#23568=ORIENTED_EDGE('',*,*,#18404,.F.);
#23569=ORIENTED_EDGE('',*,*,#18405,.F.);
#23570=ORIENTED_EDGE('',*,*,#17597,.T.);
#23571=ORIENTED_EDGE('',*,*,#18406,.T.);
#23572=ORIENTED_EDGE('',*,*,#18404,.T.);
#23573=ORIENTED_EDGE('',*,*,#18407,.T.);
#23574=ORIENTED_EDGE('',*,*,#18396,.T.);
#23575=ORIENTED_EDGE('',*,*,#18408,.T.);
#23576=ORIENTED_EDGE('',*,*,#18405,.T.);
#23577=ORIENTED_EDGE('',*,*,#18409,.T.);
#23578=ORIENTED_EDGE('',*,*,#18403,.T.);
#23579=ORIENTED_EDGE('',*,*,#18410,.T.);
#23580=ORIENTED_EDGE('',*,*,#18400,.T.);
#23581=ORIENTED_EDGE('',*,*,#18411,.T.);
#23582=ORIENTED_EDGE('',*,*,#18393,.T.);
#23583=ORIENTED_EDGE('',*,*,#18412,.T.);
#23584=ORIENTED_EDGE('',*,*,#18398,.T.);
#23585=ORIENTED_EDGE('',*,*,#18413,.T.);
#23586=ORIENTED_EDGE('',*,*,#17603,.T.);
#23587=ORIENTED_EDGE('',*,*,#18414,.T.);
#23588=ORIENTED_EDGE('',*,*,#18397,.T.);
#23589=ORIENTED_EDGE('',*,*,#18415,.T.);
#23590=ORIENTED_EDGE('',*,*,#18395,.T.);
#23591=ORIENTED_EDGE('',*,*,#18416,.T.);
#23592=ORIENTED_EDGE('',*,*,#18394,.T.);
#23593=ORIENTED_EDGE('',*,*,#18417,.T.);
#23594=ORIENTED_EDGE('',*,*,#17601,.T.);
#23595=ORIENTED_EDGE('',*,*,#18418,.T.);
#23596=ORIENTED_EDGE('',*,*,#18392,.T.);
#23597=ORIENTED_EDGE('',*,*,#18419,.T.);
#23598=ORIENTED_EDGE('',*,*,#18407,.F.);
#23599=ORIENTED_EDGE('',*,*,#18411,.F.);
#23600=ORIENTED_EDGE('',*,*,#18401,.F.);
#23601=ORIENTED_EDGE('',*,*,#17598,.F.);
#23602=ORIENTED_EDGE('',*,*,#18402,.F.);
#23603=ORIENTED_EDGE('',*,*,#18412,.F.);
#23604=ORIENTED_EDGE('',*,*,#18418,.F.);
#23605=ORIENTED_EDGE('',*,*,#17600,.F.);
#23606=ORIENTED_EDGE('',*,*,#18408,.F.);
#23607=ORIENTED_EDGE('',*,*,#18417,.F.);
#23608=ORIENTED_EDGE('',*,*,#18413,.F.);
#23609=ORIENTED_EDGE('',*,*,#18410,.F.);
#23610=ORIENTED_EDGE('',*,*,#18420,.T.);
#23611=ORIENTED_EDGE('',*,*,#18421,.T.);
#23612=ORIENTED_EDGE('',*,*,#17609,.T.);
#23613=ORIENTED_EDGE('',*,*,#18422,.T.);
#23614=ORIENTED_EDGE('',*,*,#18423,.T.);
#23615=ORIENTED_EDGE('',*,*,#18421,.F.);
#23616=ORIENTED_EDGE('',*,*,#18424,.F.);
#23617=ORIENTED_EDGE('',*,*,#18425,.F.);
#23618=ORIENTED_EDGE('',*,*,#17610,.F.);
#23619=ORIENTED_EDGE('',*,*,#18420,.F.);
#23620=ORIENTED_EDGE('',*,*,#18426,.F.);
#23621=ORIENTED_EDGE('',*,*,#18427,.T.);
#23622=ORIENTED_EDGE('',*,*,#18428,.T.);
#23623=ORIENTED_EDGE('',*,*,#18424,.T.);
#23624=ORIENTED_EDGE('',*,*,#18423,.F.);
#23625=ORIENTED_EDGE('',*,*,#18429,.T.);
#23626=ORIENTED_EDGE('',*,*,#18430,.T.);
#23627=ORIENTED_EDGE('',*,*,#18431,.T.);
#23628=ORIENTED_EDGE('',*,*,#18426,.T.);
#23629=ORIENTED_EDGE('',*,*,#18428,.F.);
#23630=ORIENTED_EDGE('',*,*,#18432,.F.);
#23631=ORIENTED_EDGE('',*,*,#18433,.F.);
#23632=ORIENTED_EDGE('',*,*,#18430,.F.);
#23633=ORIENTED_EDGE('',*,*,#18434,.F.);
#23634=ORIENTED_EDGE('',*,*,#18435,.F.);
#23635=ORIENTED_EDGE('',*,*,#17607,.T.);
#23636=ORIENTED_EDGE('',*,*,#18436,.T.);
#23637=ORIENTED_EDGE('',*,*,#18434,.T.);
#23638=ORIENTED_EDGE('',*,*,#18437,.T.);
#23639=ORIENTED_EDGE('',*,*,#18438,.F.);
#23640=ORIENTED_EDGE('',*,*,#18439,.F.);
#23641=ORIENTED_EDGE('',*,*,#18440,.F.);
#23642=ORIENTED_EDGE('',*,*,#17605,.T.);
#23643=ORIENTED_EDGE('',*,*,#18441,.T.);
#23644=ORIENTED_EDGE('',*,*,#18439,.T.);
#23645=ORIENTED_EDGE('',*,*,#18442,.T.);
#23646=ORIENTED_EDGE('',*,*,#18432,.T.);
#23647=ORIENTED_EDGE('',*,*,#18443,.T.);
#23648=ORIENTED_EDGE('',*,*,#18440,.T.);
#23649=ORIENTED_EDGE('',*,*,#18444,.T.);
#23650=ORIENTED_EDGE('',*,*,#18438,.T.);
#23651=ORIENTED_EDGE('',*,*,#18445,.T.);
#23652=ORIENTED_EDGE('',*,*,#18435,.T.);
#23653=ORIENTED_EDGE('',*,*,#18446,.T.);
#23654=ORIENTED_EDGE('',*,*,#17611,.T.);
#23655=ORIENTED_EDGE('',*,*,#18425,.T.);
#23656=ORIENTED_EDGE('',*,*,#18433,.T.);
#23657=ORIENTED_EDGE('',*,*,#18447,.T.);
#23658=ORIENTED_EDGE('',*,*,#18422,.F.);
#23659=ORIENTED_EDGE('',*,*,#17608,.F.);
#23660=ORIENTED_EDGE('',*,*,#18437,.F.);
#23661=ORIENTED_EDGE('',*,*,#18429,.F.);
#23662=ORIENTED_EDGE('',*,*,#18443,.F.);
#23663=ORIENTED_EDGE('',*,*,#18427,.F.);
#23664=ORIENTED_EDGE('',*,*,#18431,.F.);
#23665=ORIENTED_EDGE('',*,*,#18445,.F.);
#23666=ORIENTED_EDGE('',*,*,#18448,.F.);
#23667=ORIENTED_EDGE('',*,*,#18449,.F.);
#23668=ORIENTED_EDGE('',*,*,#18450,.F.);
#23669=ORIENTED_EDGE('',*,*,#18451,.F.);
#23670=ORIENTED_EDGE('',*,*,#18452,.F.);
#23671=ORIENTED_EDGE('',*,*,#18453,.F.);
#23672=ORIENTED_EDGE('',*,*,#18454,.F.);
#23673=ORIENTED_EDGE('',*,*,#18455,.F.);
#23674=ORIENTED_EDGE('',*,*,#18456,.F.);
#23675=ORIENTED_EDGE('',*,*,#17615,.T.);
#23676=ORIENTED_EDGE('',*,*,#18457,.T.);
#23677=ORIENTED_EDGE('',*,*,#18455,.T.);
#23678=ORIENTED_EDGE('',*,*,#18458,.T.);
#23679=ORIENTED_EDGE('',*,*,#18459,.F.);
#23680=ORIENTED_EDGE('',*,*,#18460,.F.);
#23681=ORIENTED_EDGE('',*,*,#18461,.F.);
#23682=ORIENTED_EDGE('',*,*,#17613,.T.);
#23683=ORIENTED_EDGE('',*,*,#18462,.T.);
#23684=ORIENTED_EDGE('',*,*,#18460,.T.);
#23685=ORIENTED_EDGE('',*,*,#18463,.T.);
#23686=ORIENTED_EDGE('',*,*,#18452,.T.);
#23687=ORIENTED_EDGE('',*,*,#18464,.T.);
#23688=ORIENTED_EDGE('',*,*,#18461,.T.);
#23689=ORIENTED_EDGE('',*,*,#18465,.T.);
#23690=ORIENTED_EDGE('',*,*,#18459,.T.);
#23691=ORIENTED_EDGE('',*,*,#18466,.T.);
#23692=ORIENTED_EDGE('',*,*,#18456,.T.);
#23693=ORIENTED_EDGE('',*,*,#18467,.T.);
#23694=ORIENTED_EDGE('',*,*,#18449,.T.);
#23695=ORIENTED_EDGE('',*,*,#18468,.T.);
#23696=ORIENTED_EDGE('',*,*,#18454,.T.);
#23697=ORIENTED_EDGE('',*,*,#18469,.T.);
#23698=ORIENTED_EDGE('',*,*,#17619,.T.);
#23699=ORIENTED_EDGE('',*,*,#18470,.T.);
#23700=ORIENTED_EDGE('',*,*,#18453,.T.);
#23701=ORIENTED_EDGE('',*,*,#18471,.T.);
#23702=ORIENTED_EDGE('',*,*,#18451,.T.);
#23703=ORIENTED_EDGE('',*,*,#18472,.T.);
#23704=ORIENTED_EDGE('',*,*,#18450,.T.);
#23705=ORIENTED_EDGE('',*,*,#18473,.T.);
#23706=ORIENTED_EDGE('',*,*,#17617,.T.);
#23707=ORIENTED_EDGE('',*,*,#18474,.T.);
#23708=ORIENTED_EDGE('',*,*,#18448,.T.);
#23709=ORIENTED_EDGE('',*,*,#18475,.T.);
#23710=ORIENTED_EDGE('',*,*,#18463,.F.);
#23711=ORIENTED_EDGE('',*,*,#18467,.F.);
#23712=ORIENTED_EDGE('',*,*,#18457,.F.);
#23713=ORIENTED_EDGE('',*,*,#17614,.F.);
#23714=ORIENTED_EDGE('',*,*,#18458,.F.);
#23715=ORIENTED_EDGE('',*,*,#18468,.F.);
#23716=ORIENTED_EDGE('',*,*,#18474,.F.);
#23717=ORIENTED_EDGE('',*,*,#17616,.F.);
#23718=ORIENTED_EDGE('',*,*,#18464,.F.);
#23719=ORIENTED_EDGE('',*,*,#18473,.F.);
#23720=ORIENTED_EDGE('',*,*,#18469,.F.);
#23721=ORIENTED_EDGE('',*,*,#18466,.F.);
#23722=ORIENTED_EDGE('',*,*,#18476,.F.);
#23723=ORIENTED_EDGE('',*,*,#18477,.F.);
#23724=ORIENTED_EDGE('',*,*,#18478,.F.);
#23725=ORIENTED_EDGE('',*,*,#18479,.T.);
#23726=ORIENTED_EDGE('',*,*,#18480,.T.);
#23727=ORIENTED_EDGE('',*,*,#18477,.T.);
#23728=ORIENTED_EDGE('',*,*,#18481,.T.);
#23729=ORIENTED_EDGE('',*,*,#18482,.T.);
#23730=ORIENTED_EDGE('',*,*,#17627,.T.);
#23731=ORIENTED_EDGE('',*,*,#18483,.T.);
#23732=ORIENTED_EDGE('',*,*,#18478,.T.);
#23733=ORIENTED_EDGE('',*,*,#18484,.T.);
#23734=ORIENTED_EDGE('',*,*,#18485,.F.);
#23735=ORIENTED_EDGE('',*,*,#18486,.F.);
#23736=ORIENTED_EDGE('',*,*,#18487,.F.);
#23737=ORIENTED_EDGE('',*,*,#18488,.T.);
#23738=ORIENTED_EDGE('',*,*,#18489,.T.);
#23739=ORIENTED_EDGE('',*,*,#18486,.T.);
#23740=ORIENTED_EDGE('',*,*,#18490,.T.);
#23741=ORIENTED_EDGE('',*,*,#18491,.T.);
#23742=ORIENTED_EDGE('',*,*,#18476,.T.);
#23743=ORIENTED_EDGE('',*,*,#18492,.T.);
#23744=ORIENTED_EDGE('',*,*,#18487,.T.);
#23745=ORIENTED_EDGE('',*,*,#18493,.T.);
#23746=ORIENTED_EDGE('',*,*,#17625,.T.);
#23747=ORIENTED_EDGE('',*,*,#18494,.T.);
#23748=ORIENTED_EDGE('',*,*,#18485,.T.);
#23749=ORIENTED_EDGE('',*,*,#18495,.T.);
#23750=ORIENTED_EDGE('',*,*,#18479,.F.);
#23751=ORIENTED_EDGE('',*,*,#18496,.T.);
#23752=ORIENTED_EDGE('',*,*,#18497,.T.);
#23753=ORIENTED_EDGE('',*,*,#17621,.T.);
#23754=ORIENTED_EDGE('',*,*,#18498,.T.);
#23755=ORIENTED_EDGE('',*,*,#18481,.F.);
#23756=ORIENTED_EDGE('',*,*,#18493,.F.);
#23757=ORIENTED_EDGE('',*,*,#18489,.F.);
#23758=ORIENTED_EDGE('',*,*,#18499,.F.);
#23759=ORIENTED_EDGE('',*,*,#18482,.F.);
#23760=ORIENTED_EDGE('',*,*,#18499,.T.);
#23761=ORIENTED_EDGE('',*,*,#18488,.F.);
#23762=ORIENTED_EDGE('',*,*,#18500,.F.);
#23763=ORIENTED_EDGE('',*,*,#18501,.T.);
#23764=ORIENTED_EDGE('',*,*,#18496,.F.);
#23765=ORIENTED_EDGE('',*,*,#18491,.F.);
#23766=ORIENTED_EDGE('',*,*,#18502,.T.);
#23767=ORIENTED_EDGE('',*,*,#17623,.T.);
#23768=ORIENTED_EDGE('',*,*,#18503,.T.);
#23769=ORIENTED_EDGE('',*,*,#18500,.T.);
#23770=ORIENTED_EDGE('',*,*,#18490,.F.);
#23771=ORIENTED_EDGE('',*,*,#18494,.F.);
#23772=ORIENTED_EDGE('',*,*,#17624,.F.);
#23773=ORIENTED_EDGE('',*,*,#18502,.F.);
#23774=ORIENTED_EDGE('',*,*,#18480,.F.);
#23775=ORIENTED_EDGE('',*,*,#18498,.F.);
#23776=ORIENTED_EDGE('',*,*,#17620,.F.);
#23777=ORIENTED_EDGE('',*,*,#18484,.F.);
#23778=ORIENTED_EDGE('',*,*,#18504,.F.);
#23779=ORIENTED_EDGE('',*,*,#18505,.F.);
#23780=ORIENTED_EDGE('',*,*,#18506,.F.);
#23781=ORIENTED_EDGE('',*,*,#18507,.F.);
#23782=ORIENTED_EDGE('',*,*,#18508,.F.);
#23783=ORIENTED_EDGE('',*,*,#18509,.F.);
#23784=ORIENTED_EDGE('',*,*,#18510,.F.);
#23785=ORIENTED_EDGE('',*,*,#18511,.F.);
#23786=ORIENTED_EDGE('',*,*,#18512,.F.);
#23787=ORIENTED_EDGE('',*,*,#17631,.T.);
#23788=ORIENTED_EDGE('',*,*,#18513,.T.);
#23789=ORIENTED_EDGE('',*,*,#18511,.T.);
#23790=ORIENTED_EDGE('',*,*,#18514,.T.);
#23791=ORIENTED_EDGE('',*,*,#18515,.F.);
#23792=ORIENTED_EDGE('',*,*,#18516,.F.);
#23793=ORIENTED_EDGE('',*,*,#18517,.F.);
#23794=ORIENTED_EDGE('',*,*,#17629,.T.);
#23795=ORIENTED_EDGE('',*,*,#18518,.T.);
#23796=ORIENTED_EDGE('',*,*,#18516,.T.);
#23797=ORIENTED_EDGE('',*,*,#18519,.T.);
#23798=ORIENTED_EDGE('',*,*,#18508,.T.);
#23799=ORIENTED_EDGE('',*,*,#18520,.T.);
#23800=ORIENTED_EDGE('',*,*,#18517,.T.);
#23801=ORIENTED_EDGE('',*,*,#18521,.T.);
#23802=ORIENTED_EDGE('',*,*,#18515,.T.);
#23803=ORIENTED_EDGE('',*,*,#18522,.T.);
#23804=ORIENTED_EDGE('',*,*,#18512,.T.);
#23805=ORIENTED_EDGE('',*,*,#18523,.T.);
#23806=ORIENTED_EDGE('',*,*,#18505,.T.);
#23807=ORIENTED_EDGE('',*,*,#18524,.T.);
#23808=ORIENTED_EDGE('',*,*,#18510,.T.);
#23809=ORIENTED_EDGE('',*,*,#18525,.T.);
#23810=ORIENTED_EDGE('',*,*,#17635,.T.);
#23811=ORIENTED_EDGE('',*,*,#18526,.T.);
#23812=ORIENTED_EDGE('',*,*,#18509,.T.);
#23813=ORIENTED_EDGE('',*,*,#18527,.T.);
#23814=ORIENTED_EDGE('',*,*,#18507,.T.);
#23815=ORIENTED_EDGE('',*,*,#18528,.T.);
#23816=ORIENTED_EDGE('',*,*,#18506,.T.);
#23817=ORIENTED_EDGE('',*,*,#18529,.T.);
#23818=ORIENTED_EDGE('',*,*,#17633,.T.);
#23819=ORIENTED_EDGE('',*,*,#18530,.T.);
#23820=ORIENTED_EDGE('',*,*,#18504,.T.);
#23821=ORIENTED_EDGE('',*,*,#18531,.T.);
#23822=ORIENTED_EDGE('',*,*,#18519,.F.);
#23823=ORIENTED_EDGE('',*,*,#18523,.F.);
#23824=ORIENTED_EDGE('',*,*,#18513,.F.);
#23825=ORIENTED_EDGE('',*,*,#17630,.F.);
#23826=ORIENTED_EDGE('',*,*,#18514,.F.);
#23827=ORIENTED_EDGE('',*,*,#18524,.F.);
#23828=ORIENTED_EDGE('',*,*,#18530,.F.);
#23829=ORIENTED_EDGE('',*,*,#17632,.F.);
#23830=ORIENTED_EDGE('',*,*,#18520,.F.);
#23831=ORIENTED_EDGE('',*,*,#18529,.F.);
#23832=ORIENTED_EDGE('',*,*,#18525,.F.);
#23833=ORIENTED_EDGE('',*,*,#18522,.F.);
#23834=ORIENTED_EDGE('',*,*,#18532,.F.);
#23835=ORIENTED_EDGE('',*,*,#18533,.F.);
#23836=ORIENTED_EDGE('',*,*,#18534,.F.);
#23837=ORIENTED_EDGE('',*,*,#18535,.F.);
#23838=ORIENTED_EDGE('',*,*,#18536,.F.);
#23839=ORIENTED_EDGE('',*,*,#18537,.F.);
#23840=ORIENTED_EDGE('',*,*,#18538,.F.);
#23841=ORIENTED_EDGE('',*,*,#18539,.F.);
#23842=ORIENTED_EDGE('',*,*,#18540,.F.);
#23843=ORIENTED_EDGE('',*,*,#17639,.T.);
#23844=ORIENTED_EDGE('',*,*,#18541,.T.);
#23845=ORIENTED_EDGE('',*,*,#18539,.T.);
#23846=ORIENTED_EDGE('',*,*,#18542,.T.);
#23847=ORIENTED_EDGE('',*,*,#18543,.F.);
#23848=ORIENTED_EDGE('',*,*,#18544,.F.);
#23849=ORIENTED_EDGE('',*,*,#18545,.F.);
#23850=ORIENTED_EDGE('',*,*,#17637,.T.);
#23851=ORIENTED_EDGE('',*,*,#18546,.T.);
#23852=ORIENTED_EDGE('',*,*,#18544,.T.);
#23853=ORIENTED_EDGE('',*,*,#18547,.T.);
#23854=ORIENTED_EDGE('',*,*,#18536,.T.);
#23855=ORIENTED_EDGE('',*,*,#18548,.T.);
#23856=ORIENTED_EDGE('',*,*,#18545,.T.);
#23857=ORIENTED_EDGE('',*,*,#18549,.T.);
#23858=ORIENTED_EDGE('',*,*,#18543,.T.);
#23859=ORIENTED_EDGE('',*,*,#18550,.T.);
#23860=ORIENTED_EDGE('',*,*,#18540,.T.);
#23861=ORIENTED_EDGE('',*,*,#18551,.T.);
#23862=ORIENTED_EDGE('',*,*,#18533,.T.);
#23863=ORIENTED_EDGE('',*,*,#18552,.T.);
#23864=ORIENTED_EDGE('',*,*,#18538,.T.);
#23865=ORIENTED_EDGE('',*,*,#18553,.T.);
#23866=ORIENTED_EDGE('',*,*,#17643,.T.);
#23867=ORIENTED_EDGE('',*,*,#18554,.T.);
#23868=ORIENTED_EDGE('',*,*,#18537,.T.);
#23869=ORIENTED_EDGE('',*,*,#18555,.T.);
#23870=ORIENTED_EDGE('',*,*,#18535,.T.);
#23871=ORIENTED_EDGE('',*,*,#18556,.T.);
#23872=ORIENTED_EDGE('',*,*,#18534,.T.);
#23873=ORIENTED_EDGE('',*,*,#18557,.T.);
#23874=ORIENTED_EDGE('',*,*,#17641,.T.);
#23875=ORIENTED_EDGE('',*,*,#18558,.T.);
#23876=ORIENTED_EDGE('',*,*,#18532,.T.);
#23877=ORIENTED_EDGE('',*,*,#18559,.T.);
#23878=ORIENTED_EDGE('',*,*,#18547,.F.);
#23879=ORIENTED_EDGE('',*,*,#18551,.F.);
#23880=ORIENTED_EDGE('',*,*,#18541,.F.);
#23881=ORIENTED_EDGE('',*,*,#17638,.F.);
#23882=ORIENTED_EDGE('',*,*,#18542,.F.);
#23883=ORIENTED_EDGE('',*,*,#18552,.F.);
#23884=ORIENTED_EDGE('',*,*,#18558,.F.);
#23885=ORIENTED_EDGE('',*,*,#17640,.F.);
#23886=ORIENTED_EDGE('',*,*,#18548,.F.);
#23887=ORIENTED_EDGE('',*,*,#18557,.F.);
#23888=ORIENTED_EDGE('',*,*,#18553,.F.);
#23889=ORIENTED_EDGE('',*,*,#18550,.F.);
#23890=ORIENTED_EDGE('',*,*,#18560,.T.);
#23891=ORIENTED_EDGE('',*,*,#18561,.T.);
#23892=ORIENTED_EDGE('',*,*,#17649,.T.);
#23893=ORIENTED_EDGE('',*,*,#18562,.T.);
#23894=ORIENTED_EDGE('',*,*,#18563,.T.);
#23895=ORIENTED_EDGE('',*,*,#18561,.F.);
#23896=ORIENTED_EDGE('',*,*,#18564,.F.);
#23897=ORIENTED_EDGE('',*,*,#18565,.F.);
#23898=ORIENTED_EDGE('',*,*,#17650,.F.);
#23899=ORIENTED_EDGE('',*,*,#18560,.F.);
#23900=ORIENTED_EDGE('',*,*,#18566,.F.);
#23901=ORIENTED_EDGE('',*,*,#18567,.T.);
#23902=ORIENTED_EDGE('',*,*,#18568,.T.);
#23903=ORIENTED_EDGE('',*,*,#18564,.T.);
#23904=ORIENTED_EDGE('',*,*,#18563,.F.);
#23905=ORIENTED_EDGE('',*,*,#18569,.T.);
#23906=ORIENTED_EDGE('',*,*,#18570,.T.);
#23907=ORIENTED_EDGE('',*,*,#18571,.T.);
#23908=ORIENTED_EDGE('',*,*,#18566,.T.);
#23909=ORIENTED_EDGE('',*,*,#18568,.F.);
#23910=ORIENTED_EDGE('',*,*,#18572,.F.);
#23911=ORIENTED_EDGE('',*,*,#18573,.F.);
#23912=ORIENTED_EDGE('',*,*,#18570,.F.);
#23913=ORIENTED_EDGE('',*,*,#18574,.F.);
#23914=ORIENTED_EDGE('',*,*,#18575,.F.);
#23915=ORIENTED_EDGE('',*,*,#17647,.T.);
#23916=ORIENTED_EDGE('',*,*,#18576,.T.);
#23917=ORIENTED_EDGE('',*,*,#18574,.T.);
#23918=ORIENTED_EDGE('',*,*,#18577,.T.);
#23919=ORIENTED_EDGE('',*,*,#18578,.F.);
#23920=ORIENTED_EDGE('',*,*,#18579,.F.);
#23921=ORIENTED_EDGE('',*,*,#18580,.F.);
#23922=ORIENTED_EDGE('',*,*,#17645,.T.);
#23923=ORIENTED_EDGE('',*,*,#18581,.T.);
#23924=ORIENTED_EDGE('',*,*,#18579,.T.);
#23925=ORIENTED_EDGE('',*,*,#18582,.T.);
#23926=ORIENTED_EDGE('',*,*,#18572,.T.);
#23927=ORIENTED_EDGE('',*,*,#18583,.T.);
#23928=ORIENTED_EDGE('',*,*,#18580,.T.);
#23929=ORIENTED_EDGE('',*,*,#18584,.T.);
#23930=ORIENTED_EDGE('',*,*,#18578,.T.);
#23931=ORIENTED_EDGE('',*,*,#18585,.T.);
#23932=ORIENTED_EDGE('',*,*,#18575,.T.);
#23933=ORIENTED_EDGE('',*,*,#18586,.T.);
#23934=ORIENTED_EDGE('',*,*,#17651,.T.);
#23935=ORIENTED_EDGE('',*,*,#18565,.T.);
#23936=ORIENTED_EDGE('',*,*,#18573,.T.);
#23937=ORIENTED_EDGE('',*,*,#18587,.T.);
#23938=ORIENTED_EDGE('',*,*,#18562,.F.);
#23939=ORIENTED_EDGE('',*,*,#17648,.F.);
#23940=ORIENTED_EDGE('',*,*,#18577,.F.);
#23941=ORIENTED_EDGE('',*,*,#18569,.F.);
#23942=ORIENTED_EDGE('',*,*,#18583,.F.);
#23943=ORIENTED_EDGE('',*,*,#18567,.F.);
#23944=ORIENTED_EDGE('',*,*,#18571,.F.);
#23945=ORIENTED_EDGE('',*,*,#18585,.F.);
#23946=ORIENTED_EDGE('',*,*,#18588,.F.);
#23947=ORIENTED_EDGE('',*,*,#18589,.F.);
#23948=ORIENTED_EDGE('',*,*,#18590,.F.);
#23949=ORIENTED_EDGE('',*,*,#18591,.F.);
#23950=ORIENTED_EDGE('',*,*,#18592,.F.);
#23951=ORIENTED_EDGE('',*,*,#18593,.F.);
#23952=ORIENTED_EDGE('',*,*,#18594,.F.);
#23953=ORIENTED_EDGE('',*,*,#18595,.F.);
#23954=ORIENTED_EDGE('',*,*,#18596,.F.);
#23955=ORIENTED_EDGE('',*,*,#17655,.T.);
#23956=ORIENTED_EDGE('',*,*,#18597,.T.);
#23957=ORIENTED_EDGE('',*,*,#18595,.T.);
#23958=ORIENTED_EDGE('',*,*,#18598,.T.);
#23959=ORIENTED_EDGE('',*,*,#18599,.F.);
#23960=ORIENTED_EDGE('',*,*,#18600,.F.);
#23961=ORIENTED_EDGE('',*,*,#18601,.F.);
#23962=ORIENTED_EDGE('',*,*,#17653,.T.);
#23963=ORIENTED_EDGE('',*,*,#18602,.T.);
#23964=ORIENTED_EDGE('',*,*,#18600,.T.);
#23965=ORIENTED_EDGE('',*,*,#18603,.T.);
#23966=ORIENTED_EDGE('',*,*,#18592,.T.);
#23967=ORIENTED_EDGE('',*,*,#18604,.T.);
#23968=ORIENTED_EDGE('',*,*,#18601,.T.);
#23969=ORIENTED_EDGE('',*,*,#18605,.T.);
#23970=ORIENTED_EDGE('',*,*,#18599,.T.);
#23971=ORIENTED_EDGE('',*,*,#18606,.T.);
#23972=ORIENTED_EDGE('',*,*,#18596,.T.);
#23973=ORIENTED_EDGE('',*,*,#18607,.T.);
#23974=ORIENTED_EDGE('',*,*,#18589,.T.);
#23975=ORIENTED_EDGE('',*,*,#18608,.T.);
#23976=ORIENTED_EDGE('',*,*,#18594,.T.);
#23977=ORIENTED_EDGE('',*,*,#18609,.T.);
#23978=ORIENTED_EDGE('',*,*,#17659,.T.);
#23979=ORIENTED_EDGE('',*,*,#18610,.T.);
#23980=ORIENTED_EDGE('',*,*,#18593,.T.);
#23981=ORIENTED_EDGE('',*,*,#18611,.T.);
#23982=ORIENTED_EDGE('',*,*,#18591,.T.);
#23983=ORIENTED_EDGE('',*,*,#18612,.T.);
#23984=ORIENTED_EDGE('',*,*,#18590,.T.);
#23985=ORIENTED_EDGE('',*,*,#18613,.T.);
#23986=ORIENTED_EDGE('',*,*,#17657,.T.);
#23987=ORIENTED_EDGE('',*,*,#18614,.T.);
#23988=ORIENTED_EDGE('',*,*,#18588,.T.);
#23989=ORIENTED_EDGE('',*,*,#18615,.T.);
#23990=ORIENTED_EDGE('',*,*,#18603,.F.);
#23991=ORIENTED_EDGE('',*,*,#18607,.F.);
#23992=ORIENTED_EDGE('',*,*,#18597,.F.);
#23993=ORIENTED_EDGE('',*,*,#17654,.F.);
#23994=ORIENTED_EDGE('',*,*,#18598,.F.);
#23995=ORIENTED_EDGE('',*,*,#18608,.F.);
#23996=ORIENTED_EDGE('',*,*,#18614,.F.);
#23997=ORIENTED_EDGE('',*,*,#17656,.F.);
#23998=ORIENTED_EDGE('',*,*,#18604,.F.);
#23999=ORIENTED_EDGE('',*,*,#18613,.F.);
#24000=ORIENTED_EDGE('',*,*,#18609,.F.);
#24001=ORIENTED_EDGE('',*,*,#18606,.F.);
#24002=ORIENTED_EDGE('',*,*,#18616,.F.);
#24003=ORIENTED_EDGE('',*,*,#18617,.F.);
#24004=ORIENTED_EDGE('',*,*,#18618,.F.);
#24005=ORIENTED_EDGE('',*,*,#18619,.T.);
#24006=ORIENTED_EDGE('',*,*,#18620,.T.);
#24007=ORIENTED_EDGE('',*,*,#18617,.T.);
#24008=ORIENTED_EDGE('',*,*,#18621,.T.);
#24009=ORIENTED_EDGE('',*,*,#18622,.T.);
#24010=ORIENTED_EDGE('',*,*,#17667,.T.);
#24011=ORIENTED_EDGE('',*,*,#18623,.T.);
#24012=ORIENTED_EDGE('',*,*,#18618,.T.);
#24013=ORIENTED_EDGE('',*,*,#18624,.T.);
#24014=ORIENTED_EDGE('',*,*,#18625,.F.);
#24015=ORIENTED_EDGE('',*,*,#18626,.F.);
#24016=ORIENTED_EDGE('',*,*,#18627,.F.);
#24017=ORIENTED_EDGE('',*,*,#18628,.T.);
#24018=ORIENTED_EDGE('',*,*,#18629,.T.);
#24019=ORIENTED_EDGE('',*,*,#18626,.T.);
#24020=ORIENTED_EDGE('',*,*,#18630,.T.);
#24021=ORIENTED_EDGE('',*,*,#18631,.T.);
#24022=ORIENTED_EDGE('',*,*,#18616,.T.);
#24023=ORIENTED_EDGE('',*,*,#18632,.T.);
#24024=ORIENTED_EDGE('',*,*,#18627,.T.);
#24025=ORIENTED_EDGE('',*,*,#18633,.T.);
#24026=ORIENTED_EDGE('',*,*,#17665,.T.);
#24027=ORIENTED_EDGE('',*,*,#18634,.T.);
#24028=ORIENTED_EDGE('',*,*,#18625,.T.);
#24029=ORIENTED_EDGE('',*,*,#18635,.T.);
#24030=ORIENTED_EDGE('',*,*,#18619,.F.);
#24031=ORIENTED_EDGE('',*,*,#18636,.T.);
#24032=ORIENTED_EDGE('',*,*,#18637,.T.);
#24033=ORIENTED_EDGE('',*,*,#17661,.T.);
#24034=ORIENTED_EDGE('',*,*,#18638,.T.);
#24035=ORIENTED_EDGE('',*,*,#18621,.F.);
#24036=ORIENTED_EDGE('',*,*,#18633,.F.);
#24037=ORIENTED_EDGE('',*,*,#18629,.F.);
#24038=ORIENTED_EDGE('',*,*,#18639,.F.);
#24039=ORIENTED_EDGE('',*,*,#18622,.F.);
#24040=ORIENTED_EDGE('',*,*,#18639,.T.);
#24041=ORIENTED_EDGE('',*,*,#18628,.F.);
#24042=ORIENTED_EDGE('',*,*,#18640,.F.);
#24043=ORIENTED_EDGE('',*,*,#18641,.T.);
#24044=ORIENTED_EDGE('',*,*,#18636,.F.);
#24045=ORIENTED_EDGE('',*,*,#18631,.F.);
#24046=ORIENTED_EDGE('',*,*,#18642,.T.);
#24047=ORIENTED_EDGE('',*,*,#17663,.T.);
#24048=ORIENTED_EDGE('',*,*,#18643,.T.);
#24049=ORIENTED_EDGE('',*,*,#18640,.T.);
#24050=ORIENTED_EDGE('',*,*,#18630,.F.);
#24051=ORIENTED_EDGE('',*,*,#18634,.F.);
#24052=ORIENTED_EDGE('',*,*,#17664,.F.);
#24053=ORIENTED_EDGE('',*,*,#18642,.F.);
#24054=ORIENTED_EDGE('',*,*,#18620,.F.);
#24055=ORIENTED_EDGE('',*,*,#18638,.F.);
#24056=ORIENTED_EDGE('',*,*,#17660,.F.);
#24057=ORIENTED_EDGE('',*,*,#18624,.F.);
#24058=ORIENTED_EDGE('',*,*,#18644,.F.);
#24059=ORIENTED_EDGE('',*,*,#18645,.F.);
#24060=ORIENTED_EDGE('',*,*,#18646,.F.);
#24061=ORIENTED_EDGE('',*,*,#18647,.F.);
#24062=ORIENTED_EDGE('',*,*,#18648,.F.);
#24063=ORIENTED_EDGE('',*,*,#18649,.F.);
#24064=ORIENTED_EDGE('',*,*,#18650,.F.);
#24065=ORIENTED_EDGE('',*,*,#18651,.F.);
#24066=ORIENTED_EDGE('',*,*,#18652,.F.);
#24067=ORIENTED_EDGE('',*,*,#17520,.T.);
#24068=ORIENTED_EDGE('',*,*,#18653,.T.);
#24069=ORIENTED_EDGE('',*,*,#18651,.T.);
#24070=ORIENTED_EDGE('',*,*,#18654,.T.);
#24071=ORIENTED_EDGE('',*,*,#18655,.F.);
#24072=ORIENTED_EDGE('',*,*,#18656,.F.);
#24073=ORIENTED_EDGE('',*,*,#18657,.F.);
#24074=ORIENTED_EDGE('',*,*,#17515,.T.);
#24075=ORIENTED_EDGE('',*,*,#18658,.T.);
#24076=ORIENTED_EDGE('',*,*,#18656,.T.);
#24077=ORIENTED_EDGE('',*,*,#18659,.T.);
#24078=ORIENTED_EDGE('',*,*,#18648,.T.);
#24079=ORIENTED_EDGE('',*,*,#18660,.T.);
#24080=ORIENTED_EDGE('',*,*,#18657,.T.);
#24081=ORIENTED_EDGE('',*,*,#18661,.T.);
#24082=ORIENTED_EDGE('',*,*,#18655,.T.);
#24083=ORIENTED_EDGE('',*,*,#18662,.T.);
#24084=ORIENTED_EDGE('',*,*,#18652,.T.);
#24085=ORIENTED_EDGE('',*,*,#18663,.T.);
#24086=ORIENTED_EDGE('',*,*,#18645,.T.);
#24087=ORIENTED_EDGE('',*,*,#18664,.T.);
#24088=ORIENTED_EDGE('',*,*,#18650,.T.);
#24089=ORIENTED_EDGE('',*,*,#18665,.T.);
#24090=ORIENTED_EDGE('',*,*,#17513,.T.);
#24091=ORIENTED_EDGE('',*,*,#18666,.T.);
#24092=ORIENTED_EDGE('',*,*,#18649,.T.);
#24093=ORIENTED_EDGE('',*,*,#18667,.T.);
#24094=ORIENTED_EDGE('',*,*,#18647,.T.);
#24095=ORIENTED_EDGE('',*,*,#18668,.T.);
#24096=ORIENTED_EDGE('',*,*,#18646,.T.);
#24097=ORIENTED_EDGE('',*,*,#18669,.T.);
#24098=ORIENTED_EDGE('',*,*,#17522,.T.);
#24099=ORIENTED_EDGE('',*,*,#18670,.T.);
#24100=ORIENTED_EDGE('',*,*,#18644,.T.);
#24101=ORIENTED_EDGE('',*,*,#18671,.T.);
#24102=ORIENTED_EDGE('',*,*,#18659,.F.);
#24103=ORIENTED_EDGE('',*,*,#18663,.F.);
#24104=ORIENTED_EDGE('',*,*,#18653,.F.);
#24105=ORIENTED_EDGE('',*,*,#17519,.F.);
#24106=ORIENTED_EDGE('',*,*,#17516,.F.);
#24107=ORIENTED_EDGE('',*,*,#18654,.F.);
#24108=ORIENTED_EDGE('',*,*,#18664,.F.);
#24109=ORIENTED_EDGE('',*,*,#18670,.F.);
#24110=ORIENTED_EDGE('',*,*,#17521,.F.);
#24111=ORIENTED_EDGE('',*,*,#18660,.F.);
#24112=ORIENTED_EDGE('',*,*,#18669,.F.);
#24113=ORIENTED_EDGE('',*,*,#18665,.F.);
#24114=ORIENTED_EDGE('',*,*,#18662,.F.);
#24115=ORIENTED_EDGE('',*,*,#18672,.F.);
#24116=ORIENTED_EDGE('',*,*,#18673,.F.);
#24117=ORIENTED_EDGE('',*,*,#18674,.F.);
#24118=ORIENTED_EDGE('',*,*,#18675,.F.);
#24119=ORIENTED_EDGE('',*,*,#18676,.F.);
#24120=ORIENTED_EDGE('',*,*,#18677,.F.);
#24121=ORIENTED_EDGE('',*,*,#18678,.F.);
#24122=ORIENTED_EDGE('',*,*,#18679,.F.);
#24123=ORIENTED_EDGE('',*,*,#18680,.F.);
#24124=ORIENTED_EDGE('',*,*,#17671,.T.);
#24125=ORIENTED_EDGE('',*,*,#18681,.T.);
#24126=ORIENTED_EDGE('',*,*,#18679,.T.);
#24127=ORIENTED_EDGE('',*,*,#18682,.T.);
#24128=ORIENTED_EDGE('',*,*,#18683,.F.);
#24129=ORIENTED_EDGE('',*,*,#18684,.F.);
#24130=ORIENTED_EDGE('',*,*,#18685,.F.);
#24131=ORIENTED_EDGE('',*,*,#17669,.T.);
#24132=ORIENTED_EDGE('',*,*,#18686,.T.);
#24133=ORIENTED_EDGE('',*,*,#18684,.T.);
#24134=ORIENTED_EDGE('',*,*,#18687,.T.);
#24135=ORIENTED_EDGE('',*,*,#18676,.T.);
#24136=ORIENTED_EDGE('',*,*,#18688,.T.);
#24137=ORIENTED_EDGE('',*,*,#18685,.T.);
#24138=ORIENTED_EDGE('',*,*,#18689,.T.);
#24139=ORIENTED_EDGE('',*,*,#18683,.T.);
#24140=ORIENTED_EDGE('',*,*,#18690,.T.);
#24141=ORIENTED_EDGE('',*,*,#18680,.T.);
#24142=ORIENTED_EDGE('',*,*,#18691,.T.);
#24143=ORIENTED_EDGE('',*,*,#18673,.T.);
#24144=ORIENTED_EDGE('',*,*,#18692,.T.);
#24145=ORIENTED_EDGE('',*,*,#18678,.T.);
#24146=ORIENTED_EDGE('',*,*,#18693,.T.);
#24147=ORIENTED_EDGE('',*,*,#17675,.T.);
#24148=ORIENTED_EDGE('',*,*,#18694,.T.);
#24149=ORIENTED_EDGE('',*,*,#18677,.T.);
#24150=ORIENTED_EDGE('',*,*,#18695,.T.);
#24151=ORIENTED_EDGE('',*,*,#18675,.T.);
#24152=ORIENTED_EDGE('',*,*,#18696,.T.);
#24153=ORIENTED_EDGE('',*,*,#18674,.T.);
#24154=ORIENTED_EDGE('',*,*,#18697,.T.);
#24155=ORIENTED_EDGE('',*,*,#17673,.T.);
#24156=ORIENTED_EDGE('',*,*,#18698,.T.);
#24157=ORIENTED_EDGE('',*,*,#18672,.T.);
#24158=ORIENTED_EDGE('',*,*,#18699,.T.);
#24159=ORIENTED_EDGE('',*,*,#18687,.F.);
#24160=ORIENTED_EDGE('',*,*,#18691,.F.);
#24161=ORIENTED_EDGE('',*,*,#18681,.F.);
#24162=ORIENTED_EDGE('',*,*,#17670,.F.);
#24163=ORIENTED_EDGE('',*,*,#18682,.F.);
#24164=ORIENTED_EDGE('',*,*,#18692,.F.);
#24165=ORIENTED_EDGE('',*,*,#18698,.F.);
#24166=ORIENTED_EDGE('',*,*,#17672,.F.);
#24167=ORIENTED_EDGE('',*,*,#18688,.F.);
#24168=ORIENTED_EDGE('',*,*,#18697,.F.);
#24169=ORIENTED_EDGE('',*,*,#18693,.F.);
#24170=ORIENTED_EDGE('',*,*,#18690,.F.);
#24171=ORIENTED_EDGE('',*,*,#18700,.T.);
#24172=ORIENTED_EDGE('',*,*,#18701,.T.);
#24173=ORIENTED_EDGE('',*,*,#17681,.T.);
#24174=ORIENTED_EDGE('',*,*,#18702,.T.);
#24175=ORIENTED_EDGE('',*,*,#18703,.T.);
#24176=ORIENTED_EDGE('',*,*,#18701,.F.);
#24177=ORIENTED_EDGE('',*,*,#18704,.F.);
#24178=ORIENTED_EDGE('',*,*,#18705,.F.);
#24179=ORIENTED_EDGE('',*,*,#17682,.F.);
#24180=ORIENTED_EDGE('',*,*,#18700,.F.);
#24181=ORIENTED_EDGE('',*,*,#18706,.F.);
#24182=ORIENTED_EDGE('',*,*,#18707,.T.);
#24183=ORIENTED_EDGE('',*,*,#18708,.T.);
#24184=ORIENTED_EDGE('',*,*,#18704,.T.);
#24185=ORIENTED_EDGE('',*,*,#18703,.F.);
#24186=ORIENTED_EDGE('',*,*,#18709,.T.);
#24187=ORIENTED_EDGE('',*,*,#18710,.T.);
#24188=ORIENTED_EDGE('',*,*,#18711,.T.);
#24189=ORIENTED_EDGE('',*,*,#18706,.T.);
#24190=ORIENTED_EDGE('',*,*,#18708,.F.);
#24191=ORIENTED_EDGE('',*,*,#18712,.F.);
#24192=ORIENTED_EDGE('',*,*,#18713,.F.);
#24193=ORIENTED_EDGE('',*,*,#18710,.F.);
#24194=ORIENTED_EDGE('',*,*,#18714,.F.);
#24195=ORIENTED_EDGE('',*,*,#18715,.F.);
#24196=ORIENTED_EDGE('',*,*,#17679,.T.);
#24197=ORIENTED_EDGE('',*,*,#18716,.T.);
#24198=ORIENTED_EDGE('',*,*,#18714,.T.);
#24199=ORIENTED_EDGE('',*,*,#18717,.T.);
#24200=ORIENTED_EDGE('',*,*,#18718,.F.);
#24201=ORIENTED_EDGE('',*,*,#18719,.F.);
#24202=ORIENTED_EDGE('',*,*,#18720,.F.);
#24203=ORIENTED_EDGE('',*,*,#17677,.T.);
#24204=ORIENTED_EDGE('',*,*,#18721,.T.);
#24205=ORIENTED_EDGE('',*,*,#18719,.T.);
#24206=ORIENTED_EDGE('',*,*,#18722,.T.);
#24207=ORIENTED_EDGE('',*,*,#18712,.T.);
#24208=ORIENTED_EDGE('',*,*,#18723,.T.);
#24209=ORIENTED_EDGE('',*,*,#18720,.T.);
#24210=ORIENTED_EDGE('',*,*,#18724,.T.);
#24211=ORIENTED_EDGE('',*,*,#18718,.T.);
#24212=ORIENTED_EDGE('',*,*,#18725,.T.);
#24213=ORIENTED_EDGE('',*,*,#18715,.T.);
#24214=ORIENTED_EDGE('',*,*,#18726,.T.);
#24215=ORIENTED_EDGE('',*,*,#17683,.T.);
#24216=ORIENTED_EDGE('',*,*,#18705,.T.);
#24217=ORIENTED_EDGE('',*,*,#18713,.T.);
#24218=ORIENTED_EDGE('',*,*,#18727,.T.);
#24219=ORIENTED_EDGE('',*,*,#18702,.F.);
#24220=ORIENTED_EDGE('',*,*,#17680,.F.);
#24221=ORIENTED_EDGE('',*,*,#18717,.F.);
#24222=ORIENTED_EDGE('',*,*,#18709,.F.);
#24223=ORIENTED_EDGE('',*,*,#18723,.F.);
#24224=ORIENTED_EDGE('',*,*,#18707,.F.);
#24225=ORIENTED_EDGE('',*,*,#18711,.F.);
#24226=ORIENTED_EDGE('',*,*,#18725,.F.);
#24227=ORIENTED_EDGE('',*,*,#18728,.F.);
#24228=ORIENTED_EDGE('',*,*,#18729,.F.);
#24229=ORIENTED_EDGE('',*,*,#18730,.F.);
#24230=ORIENTED_EDGE('',*,*,#18731,.F.);
#24231=ORIENTED_EDGE('',*,*,#18732,.F.);
#24232=ORIENTED_EDGE('',*,*,#18733,.F.);
#24233=ORIENTED_EDGE('',*,*,#18734,.F.);
#24234=ORIENTED_EDGE('',*,*,#18735,.F.);
#24235=ORIENTED_EDGE('',*,*,#18736,.F.);
#24236=ORIENTED_EDGE('',*,*,#17687,.T.);
#24237=ORIENTED_EDGE('',*,*,#18737,.T.);
#24238=ORIENTED_EDGE('',*,*,#18735,.T.);
#24239=ORIENTED_EDGE('',*,*,#18738,.T.);
#24240=ORIENTED_EDGE('',*,*,#18739,.F.);
#24241=ORIENTED_EDGE('',*,*,#18740,.F.);
#24242=ORIENTED_EDGE('',*,*,#18741,.F.);
#24243=ORIENTED_EDGE('',*,*,#17685,.T.);
#24244=ORIENTED_EDGE('',*,*,#18742,.T.);
#24245=ORIENTED_EDGE('',*,*,#18740,.T.);
#24246=ORIENTED_EDGE('',*,*,#18743,.T.);
#24247=ORIENTED_EDGE('',*,*,#18732,.T.);
#24248=ORIENTED_EDGE('',*,*,#18744,.T.);
#24249=ORIENTED_EDGE('',*,*,#18741,.T.);
#24250=ORIENTED_EDGE('',*,*,#18745,.T.);
#24251=ORIENTED_EDGE('',*,*,#18739,.T.);
#24252=ORIENTED_EDGE('',*,*,#18746,.T.);
#24253=ORIENTED_EDGE('',*,*,#18736,.T.);
#24254=ORIENTED_EDGE('',*,*,#18747,.T.);
#24255=ORIENTED_EDGE('',*,*,#18729,.T.);
#24256=ORIENTED_EDGE('',*,*,#18748,.T.);
#24257=ORIENTED_EDGE('',*,*,#18734,.T.);
#24258=ORIENTED_EDGE('',*,*,#18749,.T.);
#24259=ORIENTED_EDGE('',*,*,#17691,.T.);
#24260=ORIENTED_EDGE('',*,*,#18750,.T.);
#24261=ORIENTED_EDGE('',*,*,#18733,.T.);
#24262=ORIENTED_EDGE('',*,*,#18751,.T.);
#24263=ORIENTED_EDGE('',*,*,#18731,.T.);
#24264=ORIENTED_EDGE('',*,*,#18752,.T.);
#24265=ORIENTED_EDGE('',*,*,#18730,.T.);
#24266=ORIENTED_EDGE('',*,*,#18753,.T.);
#24267=ORIENTED_EDGE('',*,*,#17689,.T.);
#24268=ORIENTED_EDGE('',*,*,#18754,.T.);
#24269=ORIENTED_EDGE('',*,*,#18728,.T.);
#24270=ORIENTED_EDGE('',*,*,#18755,.T.);
#24271=ORIENTED_EDGE('',*,*,#18743,.F.);
#24272=ORIENTED_EDGE('',*,*,#18747,.F.);
#24273=ORIENTED_EDGE('',*,*,#18737,.F.);
#24274=ORIENTED_EDGE('',*,*,#17686,.F.);
#24275=ORIENTED_EDGE('',*,*,#18738,.F.);
#24276=ORIENTED_EDGE('',*,*,#18748,.F.);
#24277=ORIENTED_EDGE('',*,*,#18754,.F.);
#24278=ORIENTED_EDGE('',*,*,#17688,.F.);
#24279=ORIENTED_EDGE('',*,*,#18744,.F.);
#24280=ORIENTED_EDGE('',*,*,#18753,.F.);
#24281=ORIENTED_EDGE('',*,*,#18749,.F.);
#24282=ORIENTED_EDGE('',*,*,#18746,.F.);
#24283=ORIENTED_EDGE('',*,*,#18756,.F.);
#24284=ORIENTED_EDGE('',*,*,#18757,.F.);
#24285=ORIENTED_EDGE('',*,*,#18758,.F.);
#24286=ORIENTED_EDGE('',*,*,#18759,.T.);
#24287=ORIENTED_EDGE('',*,*,#18760,.T.);
#24288=ORIENTED_EDGE('',*,*,#18757,.T.);
#24289=ORIENTED_EDGE('',*,*,#18761,.T.);
#24290=ORIENTED_EDGE('',*,*,#18762,.T.);
#24291=ORIENTED_EDGE('',*,*,#17699,.T.);
#24292=ORIENTED_EDGE('',*,*,#18763,.T.);
#24293=ORIENTED_EDGE('',*,*,#18758,.T.);
#24294=ORIENTED_EDGE('',*,*,#18764,.T.);
#24295=ORIENTED_EDGE('',*,*,#18765,.F.);
#24296=ORIENTED_EDGE('',*,*,#18766,.F.);
#24297=ORIENTED_EDGE('',*,*,#18767,.F.);
#24298=ORIENTED_EDGE('',*,*,#18768,.T.);
#24299=ORIENTED_EDGE('',*,*,#18769,.T.);
#24300=ORIENTED_EDGE('',*,*,#18766,.T.);
#24301=ORIENTED_EDGE('',*,*,#18770,.T.);
#24302=ORIENTED_EDGE('',*,*,#18771,.T.);
#24303=ORIENTED_EDGE('',*,*,#18756,.T.);
#24304=ORIENTED_EDGE('',*,*,#18772,.T.);
#24305=ORIENTED_EDGE('',*,*,#18767,.T.);
#24306=ORIENTED_EDGE('',*,*,#18773,.T.);
#24307=ORIENTED_EDGE('',*,*,#17697,.T.);
#24308=ORIENTED_EDGE('',*,*,#18774,.T.);
#24309=ORIENTED_EDGE('',*,*,#18765,.T.);
#24310=ORIENTED_EDGE('',*,*,#18775,.T.);
#24311=ORIENTED_EDGE('',*,*,#18759,.F.);
#24312=ORIENTED_EDGE('',*,*,#18776,.T.);
#24313=ORIENTED_EDGE('',*,*,#18777,.T.);
#24314=ORIENTED_EDGE('',*,*,#17693,.T.);
#24315=ORIENTED_EDGE('',*,*,#18778,.T.);
#24316=ORIENTED_EDGE('',*,*,#18761,.F.);
#24317=ORIENTED_EDGE('',*,*,#18773,.F.);
#24318=ORIENTED_EDGE('',*,*,#18769,.F.);
#24319=ORIENTED_EDGE('',*,*,#18779,.F.);
#24320=ORIENTED_EDGE('',*,*,#18762,.F.);
#24321=ORIENTED_EDGE('',*,*,#18779,.T.);
#24322=ORIENTED_EDGE('',*,*,#18768,.F.);
#24323=ORIENTED_EDGE('',*,*,#18780,.F.);
#24324=ORIENTED_EDGE('',*,*,#18781,.T.);
#24325=ORIENTED_EDGE('',*,*,#18776,.F.);
#24326=ORIENTED_EDGE('',*,*,#18771,.F.);
#24327=ORIENTED_EDGE('',*,*,#18782,.T.);
#24328=ORIENTED_EDGE('',*,*,#17695,.T.);
#24329=ORIENTED_EDGE('',*,*,#18783,.T.);
#24330=ORIENTED_EDGE('',*,*,#18780,.T.);
#24331=ORIENTED_EDGE('',*,*,#18770,.F.);
#24332=ORIENTED_EDGE('',*,*,#18774,.F.);
#24333=ORIENTED_EDGE('',*,*,#17696,.F.);
#24334=ORIENTED_EDGE('',*,*,#18782,.F.);
#24335=ORIENTED_EDGE('',*,*,#18760,.F.);
#24336=ORIENTED_EDGE('',*,*,#18778,.F.);
#24337=ORIENTED_EDGE('',*,*,#17692,.F.);
#24338=ORIENTED_EDGE('',*,*,#18764,.F.);
#24339=ORIENTED_EDGE('',*,*,#18784,.F.);
#24340=ORIENTED_EDGE('',*,*,#18785,.F.);
#24341=ORIENTED_EDGE('',*,*,#18786,.F.);
#24342=ORIENTED_EDGE('',*,*,#18787,.F.);
#24343=ORIENTED_EDGE('',*,*,#18788,.F.);
#24344=ORIENTED_EDGE('',*,*,#18789,.F.);
#24345=ORIENTED_EDGE('',*,*,#18790,.F.);
#24346=ORIENTED_EDGE('',*,*,#18791,.F.);
#24347=ORIENTED_EDGE('',*,*,#18792,.F.);
#24348=ORIENTED_EDGE('',*,*,#17703,.T.);
#24349=ORIENTED_EDGE('',*,*,#18793,.T.);
#24350=ORIENTED_EDGE('',*,*,#18791,.T.);
#24351=ORIENTED_EDGE('',*,*,#18794,.T.);
#24352=ORIENTED_EDGE('',*,*,#18795,.F.);
#24353=ORIENTED_EDGE('',*,*,#18796,.F.);
#24354=ORIENTED_EDGE('',*,*,#18797,.F.);
#24355=ORIENTED_EDGE('',*,*,#17701,.T.);
#24356=ORIENTED_EDGE('',*,*,#18798,.T.);
#24357=ORIENTED_EDGE('',*,*,#18796,.T.);
#24358=ORIENTED_EDGE('',*,*,#18799,.T.);
#24359=ORIENTED_EDGE('',*,*,#18788,.T.);
#24360=ORIENTED_EDGE('',*,*,#18800,.T.);
#24361=ORIENTED_EDGE('',*,*,#18797,.T.);
#24362=ORIENTED_EDGE('',*,*,#18801,.T.);
#24363=ORIENTED_EDGE('',*,*,#18795,.T.);
#24364=ORIENTED_EDGE('',*,*,#18802,.T.);
#24365=ORIENTED_EDGE('',*,*,#18792,.T.);
#24366=ORIENTED_EDGE('',*,*,#18803,.T.);
#24367=ORIENTED_EDGE('',*,*,#18785,.T.);
#24368=ORIENTED_EDGE('',*,*,#18804,.T.);
#24369=ORIENTED_EDGE('',*,*,#18790,.T.);
#24370=ORIENTED_EDGE('',*,*,#18805,.T.);
#24371=ORIENTED_EDGE('',*,*,#17707,.T.);
#24372=ORIENTED_EDGE('',*,*,#18806,.T.);
#24373=ORIENTED_EDGE('',*,*,#18789,.T.);
#24374=ORIENTED_EDGE('',*,*,#18807,.T.);
#24375=ORIENTED_EDGE('',*,*,#18787,.T.);
#24376=ORIENTED_EDGE('',*,*,#18808,.T.);
#24377=ORIENTED_EDGE('',*,*,#18786,.T.);
#24378=ORIENTED_EDGE('',*,*,#18809,.T.);
#24379=ORIENTED_EDGE('',*,*,#17705,.T.);
#24380=ORIENTED_EDGE('',*,*,#18810,.T.);
#24381=ORIENTED_EDGE('',*,*,#18784,.T.);
#24382=ORIENTED_EDGE('',*,*,#18811,.T.);
#24383=ORIENTED_EDGE('',*,*,#18799,.F.);
#24384=ORIENTED_EDGE('',*,*,#18803,.F.);
#24385=ORIENTED_EDGE('',*,*,#18793,.F.);
#24386=ORIENTED_EDGE('',*,*,#17702,.F.);
#24387=ORIENTED_EDGE('',*,*,#18794,.F.);
#24388=ORIENTED_EDGE('',*,*,#18804,.F.);
#24389=ORIENTED_EDGE('',*,*,#18810,.F.);
#24390=ORIENTED_EDGE('',*,*,#17704,.F.);
#24391=ORIENTED_EDGE('',*,*,#18800,.F.);
#24392=ORIENTED_EDGE('',*,*,#18809,.F.);
#24393=ORIENTED_EDGE('',*,*,#18805,.F.);
#24394=ORIENTED_EDGE('',*,*,#18802,.F.);
#24395=ORIENTED_EDGE('',*,*,#18812,.F.);
#24396=ORIENTED_EDGE('',*,*,#18813,.F.);
#24397=ORIENTED_EDGE('',*,*,#18814,.F.);
#24398=ORIENTED_EDGE('',*,*,#18815,.F.);
#24399=ORIENTED_EDGE('',*,*,#18816,.F.);
#24400=ORIENTED_EDGE('',*,*,#18817,.F.);
#24401=ORIENTED_EDGE('',*,*,#18818,.F.);
#24402=ORIENTED_EDGE('',*,*,#18819,.F.);
#24403=ORIENTED_EDGE('',*,*,#18820,.F.);
#24404=ORIENTED_EDGE('',*,*,#17711,.T.);
#24405=ORIENTED_EDGE('',*,*,#18821,.T.);
#24406=ORIENTED_EDGE('',*,*,#18819,.T.);
#24407=ORIENTED_EDGE('',*,*,#18822,.T.);
#24408=ORIENTED_EDGE('',*,*,#18823,.F.);
#24409=ORIENTED_EDGE('',*,*,#18824,.F.);
#24410=ORIENTED_EDGE('',*,*,#18825,.F.);
#24411=ORIENTED_EDGE('',*,*,#17709,.T.);
#24412=ORIENTED_EDGE('',*,*,#18826,.T.);
#24413=ORIENTED_EDGE('',*,*,#18824,.T.);
#24414=ORIENTED_EDGE('',*,*,#18827,.T.);
#24415=ORIENTED_EDGE('',*,*,#18816,.T.);
#24416=ORIENTED_EDGE('',*,*,#18828,.T.);
#24417=ORIENTED_EDGE('',*,*,#18825,.T.);
#24418=ORIENTED_EDGE('',*,*,#18829,.T.);
#24419=ORIENTED_EDGE('',*,*,#18823,.T.);
#24420=ORIENTED_EDGE('',*,*,#18830,.T.);
#24421=ORIENTED_EDGE('',*,*,#18820,.T.);
#24422=ORIENTED_EDGE('',*,*,#18831,.T.);
#24423=ORIENTED_EDGE('',*,*,#18813,.T.);
#24424=ORIENTED_EDGE('',*,*,#18832,.T.);
#24425=ORIENTED_EDGE('',*,*,#18818,.T.);
#24426=ORIENTED_EDGE('',*,*,#18833,.T.);
#24427=ORIENTED_EDGE('',*,*,#17715,.T.);
#24428=ORIENTED_EDGE('',*,*,#18834,.T.);
#24429=ORIENTED_EDGE('',*,*,#18817,.T.);
#24430=ORIENTED_EDGE('',*,*,#18835,.T.);
#24431=ORIENTED_EDGE('',*,*,#18815,.T.);
#24432=ORIENTED_EDGE('',*,*,#18836,.T.);
#24433=ORIENTED_EDGE('',*,*,#18814,.T.);
#24434=ORIENTED_EDGE('',*,*,#18837,.T.);
#24435=ORIENTED_EDGE('',*,*,#17713,.T.);
#24436=ORIENTED_EDGE('',*,*,#18838,.T.);
#24437=ORIENTED_EDGE('',*,*,#18812,.T.);
#24438=ORIENTED_EDGE('',*,*,#18839,.T.);
#24439=ORIENTED_EDGE('',*,*,#18827,.F.);
#24440=ORIENTED_EDGE('',*,*,#18831,.F.);
#24441=ORIENTED_EDGE('',*,*,#18821,.F.);
#24442=ORIENTED_EDGE('',*,*,#17710,.F.);
#24443=ORIENTED_EDGE('',*,*,#18822,.F.);
#24444=ORIENTED_EDGE('',*,*,#18832,.F.);
#24445=ORIENTED_EDGE('',*,*,#18838,.F.);
#24446=ORIENTED_EDGE('',*,*,#17712,.F.);
#24447=ORIENTED_EDGE('',*,*,#18828,.F.);
#24448=ORIENTED_EDGE('',*,*,#18837,.F.);
#24449=ORIENTED_EDGE('',*,*,#18833,.F.);
#24450=ORIENTED_EDGE('',*,*,#18830,.F.);
#24451=ORIENTED_EDGE('',*,*,#18840,.T.);
#24452=ORIENTED_EDGE('',*,*,#18841,.T.);
#24453=ORIENTED_EDGE('',*,*,#17721,.T.);
#24454=ORIENTED_EDGE('',*,*,#18842,.T.);
#24455=ORIENTED_EDGE('',*,*,#18843,.T.);
#24456=ORIENTED_EDGE('',*,*,#18841,.F.);
#24457=ORIENTED_EDGE('',*,*,#18844,.F.);
#24458=ORIENTED_EDGE('',*,*,#18845,.F.);
#24459=ORIENTED_EDGE('',*,*,#17722,.F.);
#24460=ORIENTED_EDGE('',*,*,#18840,.F.);
#24461=ORIENTED_EDGE('',*,*,#18846,.F.);
#24462=ORIENTED_EDGE('',*,*,#18847,.T.);
#24463=ORIENTED_EDGE('',*,*,#18848,.T.);
#24464=ORIENTED_EDGE('',*,*,#18844,.T.);
#24465=ORIENTED_EDGE('',*,*,#18843,.F.);
#24466=ORIENTED_EDGE('',*,*,#18849,.T.);
#24467=ORIENTED_EDGE('',*,*,#18850,.T.);
#24468=ORIENTED_EDGE('',*,*,#18851,.T.);
#24469=ORIENTED_EDGE('',*,*,#18846,.T.);
#24470=ORIENTED_EDGE('',*,*,#18848,.F.);
#24471=ORIENTED_EDGE('',*,*,#18852,.F.);
#24472=ORIENTED_EDGE('',*,*,#18853,.F.);
#24473=ORIENTED_EDGE('',*,*,#18850,.F.);
#24474=ORIENTED_EDGE('',*,*,#18854,.F.);
#24475=ORIENTED_EDGE('',*,*,#18855,.F.);
#24476=ORIENTED_EDGE('',*,*,#17719,.T.);
#24477=ORIENTED_EDGE('',*,*,#18856,.T.);
#24478=ORIENTED_EDGE('',*,*,#18854,.T.);
#24479=ORIENTED_EDGE('',*,*,#18857,.T.);
#24480=ORIENTED_EDGE('',*,*,#18858,.F.);
#24481=ORIENTED_EDGE('',*,*,#18859,.F.);
#24482=ORIENTED_EDGE('',*,*,#18860,.F.);
#24483=ORIENTED_EDGE('',*,*,#17717,.T.);
#24484=ORIENTED_EDGE('',*,*,#18861,.T.);
#24485=ORIENTED_EDGE('',*,*,#18859,.T.);
#24486=ORIENTED_EDGE('',*,*,#18862,.T.);
#24487=ORIENTED_EDGE('',*,*,#18852,.T.);
#24488=ORIENTED_EDGE('',*,*,#18863,.T.);
#24489=ORIENTED_EDGE('',*,*,#18860,.T.);
#24490=ORIENTED_EDGE('',*,*,#18864,.T.);
#24491=ORIENTED_EDGE('',*,*,#18858,.T.);
#24492=ORIENTED_EDGE('',*,*,#18865,.T.);
#24493=ORIENTED_EDGE('',*,*,#18855,.T.);
#24494=ORIENTED_EDGE('',*,*,#18866,.T.);
#24495=ORIENTED_EDGE('',*,*,#17723,.T.);
#24496=ORIENTED_EDGE('',*,*,#18845,.T.);
#24497=ORIENTED_EDGE('',*,*,#18853,.T.);
#24498=ORIENTED_EDGE('',*,*,#18867,.T.);
#24499=ORIENTED_EDGE('',*,*,#18842,.F.);
#24500=ORIENTED_EDGE('',*,*,#17720,.F.);
#24501=ORIENTED_EDGE('',*,*,#18857,.F.);
#24502=ORIENTED_EDGE('',*,*,#18849,.F.);
#24503=ORIENTED_EDGE('',*,*,#18863,.F.);
#24504=ORIENTED_EDGE('',*,*,#18847,.F.);
#24505=ORIENTED_EDGE('',*,*,#18851,.F.);
#24506=ORIENTED_EDGE('',*,*,#18865,.F.);
#24507=ORIENTED_EDGE('',*,*,#18868,.F.);
#24508=ORIENTED_EDGE('',*,*,#18869,.F.);
#24509=ORIENTED_EDGE('',*,*,#18870,.F.);
#24510=ORIENTED_EDGE('',*,*,#18871,.F.);
#24511=ORIENTED_EDGE('',*,*,#18872,.F.);
#24512=ORIENTED_EDGE('',*,*,#18873,.F.);
#24513=ORIENTED_EDGE('',*,*,#18874,.F.);
#24514=ORIENTED_EDGE('',*,*,#18875,.F.);
#24515=ORIENTED_EDGE('',*,*,#18876,.F.);
#24516=ORIENTED_EDGE('',*,*,#17727,.T.);
#24517=ORIENTED_EDGE('',*,*,#18877,.T.);
#24518=ORIENTED_EDGE('',*,*,#18875,.T.);
#24519=ORIENTED_EDGE('',*,*,#18878,.T.);
#24520=ORIENTED_EDGE('',*,*,#18879,.F.);
#24521=ORIENTED_EDGE('',*,*,#18880,.F.);
#24522=ORIENTED_EDGE('',*,*,#18881,.F.);
#24523=ORIENTED_EDGE('',*,*,#17725,.T.);
#24524=ORIENTED_EDGE('',*,*,#18882,.T.);
#24525=ORIENTED_EDGE('',*,*,#18880,.T.);
#24526=ORIENTED_EDGE('',*,*,#18883,.T.);
#24527=ORIENTED_EDGE('',*,*,#18872,.T.);
#24528=ORIENTED_EDGE('',*,*,#18884,.T.);
#24529=ORIENTED_EDGE('',*,*,#18881,.T.);
#24530=ORIENTED_EDGE('',*,*,#18885,.T.);
#24531=ORIENTED_EDGE('',*,*,#18879,.T.);
#24532=ORIENTED_EDGE('',*,*,#18886,.T.);
#24533=ORIENTED_EDGE('',*,*,#18876,.T.);
#24534=ORIENTED_EDGE('',*,*,#18887,.T.);
#24535=ORIENTED_EDGE('',*,*,#18869,.T.);
#24536=ORIENTED_EDGE('',*,*,#18888,.T.);
#24537=ORIENTED_EDGE('',*,*,#18874,.T.);
#24538=ORIENTED_EDGE('',*,*,#18889,.T.);
#24539=ORIENTED_EDGE('',*,*,#17731,.T.);
#24540=ORIENTED_EDGE('',*,*,#18890,.T.);
#24541=ORIENTED_EDGE('',*,*,#18873,.T.);
#24542=ORIENTED_EDGE('',*,*,#18891,.T.);
#24543=ORIENTED_EDGE('',*,*,#18871,.T.);
#24544=ORIENTED_EDGE('',*,*,#18892,.T.);
#24545=ORIENTED_EDGE('',*,*,#18870,.T.);
#24546=ORIENTED_EDGE('',*,*,#18893,.T.);
#24547=ORIENTED_EDGE('',*,*,#17729,.T.);
#24548=ORIENTED_EDGE('',*,*,#18894,.T.);
#24549=ORIENTED_EDGE('',*,*,#18868,.T.);
#24550=ORIENTED_EDGE('',*,*,#18895,.T.);
#24551=ORIENTED_EDGE('',*,*,#18883,.F.);
#24552=ORIENTED_EDGE('',*,*,#18887,.F.);
#24553=ORIENTED_EDGE('',*,*,#18877,.F.);
#24554=ORIENTED_EDGE('',*,*,#17726,.F.);
#24555=ORIENTED_EDGE('',*,*,#18878,.F.);
#24556=ORIENTED_EDGE('',*,*,#18888,.F.);
#24557=ORIENTED_EDGE('',*,*,#18894,.F.);
#24558=ORIENTED_EDGE('',*,*,#17728,.F.);
#24559=ORIENTED_EDGE('',*,*,#18884,.F.);
#24560=ORIENTED_EDGE('',*,*,#18893,.F.);
#24561=ORIENTED_EDGE('',*,*,#18889,.F.);
#24562=ORIENTED_EDGE('',*,*,#18886,.F.);
#24563=ORIENTED_EDGE('',*,*,#18896,.F.);
#24564=ORIENTED_EDGE('',*,*,#18897,.F.);
#24565=ORIENTED_EDGE('',*,*,#18898,.F.);
#24566=ORIENTED_EDGE('',*,*,#18899,.T.);
#24567=ORIENTED_EDGE('',*,*,#18900,.T.);
#24568=ORIENTED_EDGE('',*,*,#18897,.T.);
#24569=ORIENTED_EDGE('',*,*,#18901,.T.);
#24570=ORIENTED_EDGE('',*,*,#18902,.T.);
#24571=ORIENTED_EDGE('',*,*,#17739,.T.);
#24572=ORIENTED_EDGE('',*,*,#18903,.T.);
#24573=ORIENTED_EDGE('',*,*,#18898,.T.);
#24574=ORIENTED_EDGE('',*,*,#18904,.T.);
#24575=ORIENTED_EDGE('',*,*,#18905,.F.);
#24576=ORIENTED_EDGE('',*,*,#18906,.F.);
#24577=ORIENTED_EDGE('',*,*,#18907,.F.);
#24578=ORIENTED_EDGE('',*,*,#18908,.T.);
#24579=ORIENTED_EDGE('',*,*,#18909,.T.);
#24580=ORIENTED_EDGE('',*,*,#18906,.T.);
#24581=ORIENTED_EDGE('',*,*,#18910,.T.);
#24582=ORIENTED_EDGE('',*,*,#18911,.T.);
#24583=ORIENTED_EDGE('',*,*,#18896,.T.);
#24584=ORIENTED_EDGE('',*,*,#18912,.T.);
#24585=ORIENTED_EDGE('',*,*,#18907,.T.);
#24586=ORIENTED_EDGE('',*,*,#18913,.T.);
#24587=ORIENTED_EDGE('',*,*,#17737,.T.);
#24588=ORIENTED_EDGE('',*,*,#18914,.T.);
#24589=ORIENTED_EDGE('',*,*,#18905,.T.);
#24590=ORIENTED_EDGE('',*,*,#18915,.T.);
#24591=ORIENTED_EDGE('',*,*,#18899,.F.);
#24592=ORIENTED_EDGE('',*,*,#18916,.T.);
#24593=ORIENTED_EDGE('',*,*,#18917,.T.);
#24594=ORIENTED_EDGE('',*,*,#17733,.T.);
#24595=ORIENTED_EDGE('',*,*,#18918,.T.);
#24596=ORIENTED_EDGE('',*,*,#18901,.F.);
#24597=ORIENTED_EDGE('',*,*,#18913,.F.);
#24598=ORIENTED_EDGE('',*,*,#18909,.F.);
#24599=ORIENTED_EDGE('',*,*,#18919,.F.);
#24600=ORIENTED_EDGE('',*,*,#18902,.F.);
#24601=ORIENTED_EDGE('',*,*,#18919,.T.);
#24602=ORIENTED_EDGE('',*,*,#18908,.F.);
#24603=ORIENTED_EDGE('',*,*,#18920,.F.);
#24604=ORIENTED_EDGE('',*,*,#18921,.T.);
#24605=ORIENTED_EDGE('',*,*,#18916,.F.);
#24606=ORIENTED_EDGE('',*,*,#18911,.F.);
#24607=ORIENTED_EDGE('',*,*,#18922,.T.);
#24608=ORIENTED_EDGE('',*,*,#17735,.T.);
#24609=ORIENTED_EDGE('',*,*,#18923,.T.);
#24610=ORIENTED_EDGE('',*,*,#18920,.T.);
#24611=ORIENTED_EDGE('',*,*,#18910,.F.);
#24612=ORIENTED_EDGE('',*,*,#18914,.F.);
#24613=ORIENTED_EDGE('',*,*,#17736,.F.);
#24614=ORIENTED_EDGE('',*,*,#18922,.F.);
#24615=ORIENTED_EDGE('',*,*,#18900,.F.);
#24616=ORIENTED_EDGE('',*,*,#18918,.F.);
#24617=ORIENTED_EDGE('',*,*,#17732,.F.);
#24618=ORIENTED_EDGE('',*,*,#18904,.F.);
#24619=ORIENTED_EDGE('',*,*,#18924,.F.);
#24620=ORIENTED_EDGE('',*,*,#18925,.F.);
#24621=ORIENTED_EDGE('',*,*,#18926,.F.);
#24622=ORIENTED_EDGE('',*,*,#18927,.F.);
#24623=ORIENTED_EDGE('',*,*,#18928,.F.);
#24624=ORIENTED_EDGE('',*,*,#18929,.F.);
#24625=ORIENTED_EDGE('',*,*,#18930,.F.);
#24626=ORIENTED_EDGE('',*,*,#18931,.F.);
#24627=ORIENTED_EDGE('',*,*,#18932,.F.);
#24628=ORIENTED_EDGE('',*,*,#17743,.T.);
#24629=ORIENTED_EDGE('',*,*,#18933,.T.);
#24630=ORIENTED_EDGE('',*,*,#18931,.T.);
#24631=ORIENTED_EDGE('',*,*,#18934,.T.);
#24632=ORIENTED_EDGE('',*,*,#18935,.F.);
#24633=ORIENTED_EDGE('',*,*,#18936,.F.);
#24634=ORIENTED_EDGE('',*,*,#18937,.F.);
#24635=ORIENTED_EDGE('',*,*,#17741,.T.);
#24636=ORIENTED_EDGE('',*,*,#18938,.T.);
#24637=ORIENTED_EDGE('',*,*,#18936,.T.);
#24638=ORIENTED_EDGE('',*,*,#18939,.T.);
#24639=ORIENTED_EDGE('',*,*,#18928,.T.);
#24640=ORIENTED_EDGE('',*,*,#18940,.T.);
#24641=ORIENTED_EDGE('',*,*,#18937,.T.);
#24642=ORIENTED_EDGE('',*,*,#18941,.T.);
#24643=ORIENTED_EDGE('',*,*,#18935,.T.);
#24644=ORIENTED_EDGE('',*,*,#18942,.T.);
#24645=ORIENTED_EDGE('',*,*,#18932,.T.);
#24646=ORIENTED_EDGE('',*,*,#18943,.T.);
#24647=ORIENTED_EDGE('',*,*,#18925,.T.);
#24648=ORIENTED_EDGE('',*,*,#18944,.T.);
#24649=ORIENTED_EDGE('',*,*,#18930,.T.);
#24650=ORIENTED_EDGE('',*,*,#18945,.T.);
#24651=ORIENTED_EDGE('',*,*,#17747,.T.);
#24652=ORIENTED_EDGE('',*,*,#18946,.T.);
#24653=ORIENTED_EDGE('',*,*,#18929,.T.);
#24654=ORIENTED_EDGE('',*,*,#18947,.T.);
#24655=ORIENTED_EDGE('',*,*,#18927,.T.);
#24656=ORIENTED_EDGE('',*,*,#18948,.T.);
#24657=ORIENTED_EDGE('',*,*,#18926,.T.);
#24658=ORIENTED_EDGE('',*,*,#18949,.T.);
#24659=ORIENTED_EDGE('',*,*,#17745,.T.);
#24660=ORIENTED_EDGE('',*,*,#18950,.T.);
#24661=ORIENTED_EDGE('',*,*,#18924,.T.);
#24662=ORIENTED_EDGE('',*,*,#18951,.T.);
#24663=ORIENTED_EDGE('',*,*,#18939,.F.);
#24664=ORIENTED_EDGE('',*,*,#18943,.F.);
#24665=ORIENTED_EDGE('',*,*,#18933,.F.);
#24666=ORIENTED_EDGE('',*,*,#17742,.F.);
#24667=ORIENTED_EDGE('',*,*,#18934,.F.);
#24668=ORIENTED_EDGE('',*,*,#18944,.F.);
#24669=ORIENTED_EDGE('',*,*,#18950,.F.);
#24670=ORIENTED_EDGE('',*,*,#17744,.F.);
#24671=ORIENTED_EDGE('',*,*,#18940,.F.);
#24672=ORIENTED_EDGE('',*,*,#18949,.F.);
#24673=ORIENTED_EDGE('',*,*,#18945,.F.);
#24674=ORIENTED_EDGE('',*,*,#18942,.F.);
#24675=ORIENTED_EDGE('',*,*,#18952,.F.);
#24676=ORIENTED_EDGE('',*,*,#18953,.F.);
#24677=ORIENTED_EDGE('',*,*,#18954,.F.);
#24678=ORIENTED_EDGE('',*,*,#18955,.F.);
#24679=ORIENTED_EDGE('',*,*,#18956,.F.);
#24680=ORIENTED_EDGE('',*,*,#18957,.F.);
#24681=ORIENTED_EDGE('',*,*,#18958,.F.);
#24682=ORIENTED_EDGE('',*,*,#18959,.F.);
#24683=ORIENTED_EDGE('',*,*,#18960,.F.);
#24684=ORIENTED_EDGE('',*,*,#17751,.T.);
#24685=ORIENTED_EDGE('',*,*,#18961,.T.);
#24686=ORIENTED_EDGE('',*,*,#18959,.T.);
#24687=ORIENTED_EDGE('',*,*,#18962,.T.);
#24688=ORIENTED_EDGE('',*,*,#18963,.F.);
#24689=ORIENTED_EDGE('',*,*,#18964,.F.);
#24690=ORIENTED_EDGE('',*,*,#18965,.F.);
#24691=ORIENTED_EDGE('',*,*,#17749,.T.);
#24692=ORIENTED_EDGE('',*,*,#18966,.T.);
#24693=ORIENTED_EDGE('',*,*,#18964,.T.);
#24694=ORIENTED_EDGE('',*,*,#18967,.T.);
#24695=ORIENTED_EDGE('',*,*,#18956,.T.);
#24696=ORIENTED_EDGE('',*,*,#18968,.T.);
#24697=ORIENTED_EDGE('',*,*,#18965,.T.);
#24698=ORIENTED_EDGE('',*,*,#18969,.T.);
#24699=ORIENTED_EDGE('',*,*,#18963,.T.);
#24700=ORIENTED_EDGE('',*,*,#18970,.T.);
#24701=ORIENTED_EDGE('',*,*,#18960,.T.);
#24702=ORIENTED_EDGE('',*,*,#18971,.T.);
#24703=ORIENTED_EDGE('',*,*,#18953,.T.);
#24704=ORIENTED_EDGE('',*,*,#18972,.T.);
#24705=ORIENTED_EDGE('',*,*,#18958,.T.);
#24706=ORIENTED_EDGE('',*,*,#18973,.T.);
#24707=ORIENTED_EDGE('',*,*,#17755,.T.);
#24708=ORIENTED_EDGE('',*,*,#18974,.T.);
#24709=ORIENTED_EDGE('',*,*,#18957,.T.);
#24710=ORIENTED_EDGE('',*,*,#18975,.T.);
#24711=ORIENTED_EDGE('',*,*,#18955,.T.);
#24712=ORIENTED_EDGE('',*,*,#18976,.T.);
#24713=ORIENTED_EDGE('',*,*,#18954,.T.);
#24714=ORIENTED_EDGE('',*,*,#18977,.T.);
#24715=ORIENTED_EDGE('',*,*,#17753,.T.);
#24716=ORIENTED_EDGE('',*,*,#18978,.T.);
#24717=ORIENTED_EDGE('',*,*,#18952,.T.);
#24718=ORIENTED_EDGE('',*,*,#18979,.T.);
#24719=ORIENTED_EDGE('',*,*,#18967,.F.);
#24720=ORIENTED_EDGE('',*,*,#18971,.F.);
#24721=ORIENTED_EDGE('',*,*,#18961,.F.);
#24722=ORIENTED_EDGE('',*,*,#17750,.F.);
#24723=ORIENTED_EDGE('',*,*,#18962,.F.);
#24724=ORIENTED_EDGE('',*,*,#18972,.F.);
#24725=ORIENTED_EDGE('',*,*,#18978,.F.);
#24726=ORIENTED_EDGE('',*,*,#17752,.F.);
#24727=ORIENTED_EDGE('',*,*,#18968,.F.);
#24728=ORIENTED_EDGE('',*,*,#18977,.F.);
#24729=ORIENTED_EDGE('',*,*,#18973,.F.);
#24730=ORIENTED_EDGE('',*,*,#18970,.F.);
#24731=ORIENTED_EDGE('',*,*,#18980,.T.);
#24732=ORIENTED_EDGE('',*,*,#18981,.T.);
#24733=ORIENTED_EDGE('',*,*,#17761,.T.);
#24734=ORIENTED_EDGE('',*,*,#18982,.T.);
#24735=ORIENTED_EDGE('',*,*,#18983,.T.);
#24736=ORIENTED_EDGE('',*,*,#18981,.F.);
#24737=ORIENTED_EDGE('',*,*,#18984,.F.);
#24738=ORIENTED_EDGE('',*,*,#18985,.F.);
#24739=ORIENTED_EDGE('',*,*,#17762,.F.);
#24740=ORIENTED_EDGE('',*,*,#18980,.F.);
#24741=ORIENTED_EDGE('',*,*,#18986,.F.);
#24742=ORIENTED_EDGE('',*,*,#18987,.T.);
#24743=ORIENTED_EDGE('',*,*,#18988,.T.);
#24744=ORIENTED_EDGE('',*,*,#18984,.T.);
#24745=ORIENTED_EDGE('',*,*,#18983,.F.);
#24746=ORIENTED_EDGE('',*,*,#18989,.T.);
#24747=ORIENTED_EDGE('',*,*,#18990,.T.);
#24748=ORIENTED_EDGE('',*,*,#18991,.T.);
#24749=ORIENTED_EDGE('',*,*,#18986,.T.);
#24750=ORIENTED_EDGE('',*,*,#18988,.F.);
#24751=ORIENTED_EDGE('',*,*,#18992,.F.);
#24752=ORIENTED_EDGE('',*,*,#18993,.F.);
#24753=ORIENTED_EDGE('',*,*,#18990,.F.);
#24754=ORIENTED_EDGE('',*,*,#18994,.F.);
#24755=ORIENTED_EDGE('',*,*,#18995,.F.);
#24756=ORIENTED_EDGE('',*,*,#17759,.T.);
#24757=ORIENTED_EDGE('',*,*,#18996,.T.);
#24758=ORIENTED_EDGE('',*,*,#18994,.T.);
#24759=ORIENTED_EDGE('',*,*,#18997,.T.);
#24760=ORIENTED_EDGE('',*,*,#18998,.F.);
#24761=ORIENTED_EDGE('',*,*,#18999,.F.);
#24762=ORIENTED_EDGE('',*,*,#19000,.F.);
#24763=ORIENTED_EDGE('',*,*,#17757,.T.);
#24764=ORIENTED_EDGE('',*,*,#19001,.T.);
#24765=ORIENTED_EDGE('',*,*,#18999,.T.);
#24766=ORIENTED_EDGE('',*,*,#19002,.T.);
#24767=ORIENTED_EDGE('',*,*,#18992,.T.);
#24768=ORIENTED_EDGE('',*,*,#19003,.T.);
#24769=ORIENTED_EDGE('',*,*,#19000,.T.);
#24770=ORIENTED_EDGE('',*,*,#19004,.T.);
#24771=ORIENTED_EDGE('',*,*,#18998,.T.);
#24772=ORIENTED_EDGE('',*,*,#19005,.T.);
#24773=ORIENTED_EDGE('',*,*,#18995,.T.);
#24774=ORIENTED_EDGE('',*,*,#19006,.T.);
#24775=ORIENTED_EDGE('',*,*,#17763,.T.);
#24776=ORIENTED_EDGE('',*,*,#18985,.T.);
#24777=ORIENTED_EDGE('',*,*,#18993,.T.);
#24778=ORIENTED_EDGE('',*,*,#19007,.T.);
#24779=ORIENTED_EDGE('',*,*,#18982,.F.);
#24780=ORIENTED_EDGE('',*,*,#17760,.F.);
#24781=ORIENTED_EDGE('',*,*,#18997,.F.);
#24782=ORIENTED_EDGE('',*,*,#18989,.F.);
#24783=ORIENTED_EDGE('',*,*,#19003,.F.);
#24784=ORIENTED_EDGE('',*,*,#18987,.F.);
#24785=ORIENTED_EDGE('',*,*,#18991,.F.);
#24786=ORIENTED_EDGE('',*,*,#19005,.F.);
#24787=ORIENTED_EDGE('',*,*,#19008,.F.);
#24788=ORIENTED_EDGE('',*,*,#19009,.F.);
#24789=ORIENTED_EDGE('',*,*,#19010,.F.);
#24790=ORIENTED_EDGE('',*,*,#19011,.F.);
#24791=ORIENTED_EDGE('',*,*,#19012,.F.);
#24792=ORIENTED_EDGE('',*,*,#19013,.F.);
#24793=ORIENTED_EDGE('',*,*,#19014,.F.);
#24794=ORIENTED_EDGE('',*,*,#19015,.F.);
#24795=ORIENTED_EDGE('',*,*,#19016,.F.);
#24796=ORIENTED_EDGE('',*,*,#17767,.T.);
#24797=ORIENTED_EDGE('',*,*,#19017,.T.);
#24798=ORIENTED_EDGE('',*,*,#19015,.T.);
#24799=ORIENTED_EDGE('',*,*,#19018,.T.);
#24800=ORIENTED_EDGE('',*,*,#19019,.F.);
#24801=ORIENTED_EDGE('',*,*,#19020,.F.);
#24802=ORIENTED_EDGE('',*,*,#19021,.F.);
#24803=ORIENTED_EDGE('',*,*,#17765,.T.);
#24804=ORIENTED_EDGE('',*,*,#19022,.T.);
#24805=ORIENTED_EDGE('',*,*,#19020,.T.);
#24806=ORIENTED_EDGE('',*,*,#19023,.T.);
#24807=ORIENTED_EDGE('',*,*,#19012,.T.);
#24808=ORIENTED_EDGE('',*,*,#19024,.T.);
#24809=ORIENTED_EDGE('',*,*,#19021,.T.);
#24810=ORIENTED_EDGE('',*,*,#19025,.T.);
#24811=ORIENTED_EDGE('',*,*,#19019,.T.);
#24812=ORIENTED_EDGE('',*,*,#19026,.T.);
#24813=ORIENTED_EDGE('',*,*,#19016,.T.);
#24814=ORIENTED_EDGE('',*,*,#19027,.T.);
#24815=ORIENTED_EDGE('',*,*,#19009,.T.);
#24816=ORIENTED_EDGE('',*,*,#19028,.T.);
#24817=ORIENTED_EDGE('',*,*,#19014,.T.);
#24818=ORIENTED_EDGE('',*,*,#19029,.T.);
#24819=ORIENTED_EDGE('',*,*,#17771,.T.);
#24820=ORIENTED_EDGE('',*,*,#19030,.T.);
#24821=ORIENTED_EDGE('',*,*,#19013,.T.);
#24822=ORIENTED_EDGE('',*,*,#19031,.T.);
#24823=ORIENTED_EDGE('',*,*,#19011,.T.);
#24824=ORIENTED_EDGE('',*,*,#19032,.T.);
#24825=ORIENTED_EDGE('',*,*,#19010,.T.);
#24826=ORIENTED_EDGE('',*,*,#19033,.T.);
#24827=ORIENTED_EDGE('',*,*,#17769,.T.);
#24828=ORIENTED_EDGE('',*,*,#19034,.T.);
#24829=ORIENTED_EDGE('',*,*,#19008,.T.);
#24830=ORIENTED_EDGE('',*,*,#19035,.T.);
#24831=ORIENTED_EDGE('',*,*,#19023,.F.);
#24832=ORIENTED_EDGE('',*,*,#19027,.F.);
#24833=ORIENTED_EDGE('',*,*,#19017,.F.);
#24834=ORIENTED_EDGE('',*,*,#17766,.F.);
#24835=ORIENTED_EDGE('',*,*,#19018,.F.);
#24836=ORIENTED_EDGE('',*,*,#19028,.F.);
#24837=ORIENTED_EDGE('',*,*,#19034,.F.);
#24838=ORIENTED_EDGE('',*,*,#17768,.F.);
#24839=ORIENTED_EDGE('',*,*,#19024,.F.);
#24840=ORIENTED_EDGE('',*,*,#19033,.F.);
#24841=ORIENTED_EDGE('',*,*,#19029,.F.);
#24842=ORIENTED_EDGE('',*,*,#19026,.F.);
#24843=ORIENTED_EDGE('',*,*,#19036,.F.);
#24844=ORIENTED_EDGE('',*,*,#19037,.F.);
#24845=ORIENTED_EDGE('',*,*,#19038,.F.);
#24846=ORIENTED_EDGE('',*,*,#19039,.T.);
#24847=ORIENTED_EDGE('',*,*,#19040,.T.);
#24848=ORIENTED_EDGE('',*,*,#19037,.T.);
#24849=ORIENTED_EDGE('',*,*,#19041,.T.);
#24850=ORIENTED_EDGE('',*,*,#19042,.T.);
#24851=ORIENTED_EDGE('',*,*,#17779,.T.);
#24852=ORIENTED_EDGE('',*,*,#19043,.T.);
#24853=ORIENTED_EDGE('',*,*,#19038,.T.);
#24854=ORIENTED_EDGE('',*,*,#19044,.T.);
#24855=ORIENTED_EDGE('',*,*,#19045,.F.);
#24856=ORIENTED_EDGE('',*,*,#19046,.F.);
#24857=ORIENTED_EDGE('',*,*,#19047,.F.);
#24858=ORIENTED_EDGE('',*,*,#19048,.T.);
#24859=ORIENTED_EDGE('',*,*,#19049,.T.);
#24860=ORIENTED_EDGE('',*,*,#19046,.T.);
#24861=ORIENTED_EDGE('',*,*,#19050,.T.);
#24862=ORIENTED_EDGE('',*,*,#19051,.T.);
#24863=ORIENTED_EDGE('',*,*,#19036,.T.);
#24864=ORIENTED_EDGE('',*,*,#19052,.T.);
#24865=ORIENTED_EDGE('',*,*,#19047,.T.);
#24866=ORIENTED_EDGE('',*,*,#19053,.T.);
#24867=ORIENTED_EDGE('',*,*,#17777,.T.);
#24868=ORIENTED_EDGE('',*,*,#19054,.T.);
#24869=ORIENTED_EDGE('',*,*,#19045,.T.);
#24870=ORIENTED_EDGE('',*,*,#19055,.T.);
#24871=ORIENTED_EDGE('',*,*,#19039,.F.);
#24872=ORIENTED_EDGE('',*,*,#19056,.T.);
#24873=ORIENTED_EDGE('',*,*,#19057,.T.);
#24874=ORIENTED_EDGE('',*,*,#17773,.T.);
#24875=ORIENTED_EDGE('',*,*,#19058,.T.);
#24876=ORIENTED_EDGE('',*,*,#19041,.F.);
#24877=ORIENTED_EDGE('',*,*,#19053,.F.);
#24878=ORIENTED_EDGE('',*,*,#19049,.F.);
#24879=ORIENTED_EDGE('',*,*,#19059,.F.);
#24880=ORIENTED_EDGE('',*,*,#19042,.F.);
#24881=ORIENTED_EDGE('',*,*,#19059,.T.);
#24882=ORIENTED_EDGE('',*,*,#19048,.F.);
#24883=ORIENTED_EDGE('',*,*,#19060,.F.);
#24884=ORIENTED_EDGE('',*,*,#19061,.T.);
#24885=ORIENTED_EDGE('',*,*,#19056,.F.);
#24886=ORIENTED_EDGE('',*,*,#19051,.F.);
#24887=ORIENTED_EDGE('',*,*,#19062,.T.);
#24888=ORIENTED_EDGE('',*,*,#17775,.T.);
#24889=ORIENTED_EDGE('',*,*,#19063,.T.);
#24890=ORIENTED_EDGE('',*,*,#19060,.T.);
#24891=ORIENTED_EDGE('',*,*,#19050,.F.);
#24892=ORIENTED_EDGE('',*,*,#19054,.F.);
#24893=ORIENTED_EDGE('',*,*,#17776,.F.);
#24894=ORIENTED_EDGE('',*,*,#19062,.F.);
#24895=ORIENTED_EDGE('',*,*,#19040,.F.);
#24896=ORIENTED_EDGE('',*,*,#19058,.F.);
#24897=ORIENTED_EDGE('',*,*,#17772,.F.);
#24898=ORIENTED_EDGE('',*,*,#19044,.F.);
#24899=ORIENTED_EDGE('',*,*,#19064,.F.);
#24900=ORIENTED_EDGE('',*,*,#19065,.F.);
#24901=ORIENTED_EDGE('',*,*,#19066,.F.);
#24902=ORIENTED_EDGE('',*,*,#19067,.F.);
#24903=ORIENTED_EDGE('',*,*,#19068,.F.);
#24904=ORIENTED_EDGE('',*,*,#19069,.F.);
#24905=ORIENTED_EDGE('',*,*,#19070,.F.);
#24906=ORIENTED_EDGE('',*,*,#19071,.F.);
#24907=ORIENTED_EDGE('',*,*,#19072,.F.);
#24908=ORIENTED_EDGE('',*,*,#17783,.T.);
#24909=ORIENTED_EDGE('',*,*,#19073,.T.);
#24910=ORIENTED_EDGE('',*,*,#19071,.T.);
#24911=ORIENTED_EDGE('',*,*,#19074,.T.);
#24912=ORIENTED_EDGE('',*,*,#19075,.F.);
#24913=ORIENTED_EDGE('',*,*,#19076,.F.);
#24914=ORIENTED_EDGE('',*,*,#19077,.F.);
#24915=ORIENTED_EDGE('',*,*,#17781,.T.);
#24916=ORIENTED_EDGE('',*,*,#19078,.T.);
#24917=ORIENTED_EDGE('',*,*,#19076,.T.);
#24918=ORIENTED_EDGE('',*,*,#19079,.T.);
#24919=ORIENTED_EDGE('',*,*,#19068,.T.);
#24920=ORIENTED_EDGE('',*,*,#19080,.T.);
#24921=ORIENTED_EDGE('',*,*,#19077,.T.);
#24922=ORIENTED_EDGE('',*,*,#19081,.T.);
#24923=ORIENTED_EDGE('',*,*,#19075,.T.);
#24924=ORIENTED_EDGE('',*,*,#19082,.T.);
#24925=ORIENTED_EDGE('',*,*,#19072,.T.);
#24926=ORIENTED_EDGE('',*,*,#19083,.T.);
#24927=ORIENTED_EDGE('',*,*,#19065,.T.);
#24928=ORIENTED_EDGE('',*,*,#19084,.T.);
#24929=ORIENTED_EDGE('',*,*,#19070,.T.);
#24930=ORIENTED_EDGE('',*,*,#19085,.T.);
#24931=ORIENTED_EDGE('',*,*,#17787,.T.);
#24932=ORIENTED_EDGE('',*,*,#19086,.T.);
#24933=ORIENTED_EDGE('',*,*,#19069,.T.);
#24934=ORIENTED_EDGE('',*,*,#19087,.T.);
#24935=ORIENTED_EDGE('',*,*,#19067,.T.);
#24936=ORIENTED_EDGE('',*,*,#19088,.T.);
#24937=ORIENTED_EDGE('',*,*,#19066,.T.);
#24938=ORIENTED_EDGE('',*,*,#19089,.T.);
#24939=ORIENTED_EDGE('',*,*,#17785,.T.);
#24940=ORIENTED_EDGE('',*,*,#19090,.T.);
#24941=ORIENTED_EDGE('',*,*,#19064,.T.);
#24942=ORIENTED_EDGE('',*,*,#19091,.T.);
#24943=ORIENTED_EDGE('',*,*,#19079,.F.);
#24944=ORIENTED_EDGE('',*,*,#19083,.F.);
#24945=ORIENTED_EDGE('',*,*,#19073,.F.);
#24946=ORIENTED_EDGE('',*,*,#17782,.F.);
#24947=ORIENTED_EDGE('',*,*,#19074,.F.);
#24948=ORIENTED_EDGE('',*,*,#19084,.F.);
#24949=ORIENTED_EDGE('',*,*,#19090,.F.);
#24950=ORIENTED_EDGE('',*,*,#17784,.F.);
#24951=ORIENTED_EDGE('',*,*,#19080,.F.);
#24952=ORIENTED_EDGE('',*,*,#19089,.F.);
#24953=ORIENTED_EDGE('',*,*,#19085,.F.);
#24954=ORIENTED_EDGE('',*,*,#19082,.F.);
#24955=ORIENTED_EDGE('',*,*,#19092,.F.);
#24956=ORIENTED_EDGE('',*,*,#19093,.F.);
#24957=ORIENTED_EDGE('',*,*,#19094,.F.);
#24958=ORIENTED_EDGE('',*,*,#19095,.F.);
#24959=ORIENTED_EDGE('',*,*,#19096,.F.);
#24960=ORIENTED_EDGE('',*,*,#19097,.F.);
#24961=ORIENTED_EDGE('',*,*,#19098,.F.);
#24962=ORIENTED_EDGE('',*,*,#19099,.F.);
#24963=ORIENTED_EDGE('',*,*,#19100,.F.);
#24964=ORIENTED_EDGE('',*,*,#17791,.T.);
#24965=ORIENTED_EDGE('',*,*,#19101,.T.);
#24966=ORIENTED_EDGE('',*,*,#19099,.T.);
#24967=ORIENTED_EDGE('',*,*,#19102,.T.);
#24968=ORIENTED_EDGE('',*,*,#19103,.F.);
#24969=ORIENTED_EDGE('',*,*,#19104,.F.);
#24970=ORIENTED_EDGE('',*,*,#19105,.F.);
#24971=ORIENTED_EDGE('',*,*,#17789,.T.);
#24972=ORIENTED_EDGE('',*,*,#19106,.T.);
#24973=ORIENTED_EDGE('',*,*,#19104,.T.);
#24974=ORIENTED_EDGE('',*,*,#19107,.T.);
#24975=ORIENTED_EDGE('',*,*,#19096,.T.);
#24976=ORIENTED_EDGE('',*,*,#19108,.T.);
#24977=ORIENTED_EDGE('',*,*,#19105,.T.);
#24978=ORIENTED_EDGE('',*,*,#19109,.T.);
#24979=ORIENTED_EDGE('',*,*,#19103,.T.);
#24980=ORIENTED_EDGE('',*,*,#19110,.T.);
#24981=ORIENTED_EDGE('',*,*,#19100,.T.);
#24982=ORIENTED_EDGE('',*,*,#19111,.T.);
#24983=ORIENTED_EDGE('',*,*,#19093,.T.);
#24984=ORIENTED_EDGE('',*,*,#19112,.T.);
#24985=ORIENTED_EDGE('',*,*,#19098,.T.);
#24986=ORIENTED_EDGE('',*,*,#19113,.T.);
#24987=ORIENTED_EDGE('',*,*,#17795,.T.);
#24988=ORIENTED_EDGE('',*,*,#19114,.T.);
#24989=ORIENTED_EDGE('',*,*,#19097,.T.);
#24990=ORIENTED_EDGE('',*,*,#19115,.T.);
#24991=ORIENTED_EDGE('',*,*,#19095,.T.);
#24992=ORIENTED_EDGE('',*,*,#19116,.T.);
#24993=ORIENTED_EDGE('',*,*,#19094,.T.);
#24994=ORIENTED_EDGE('',*,*,#19117,.T.);
#24995=ORIENTED_EDGE('',*,*,#17793,.T.);
#24996=ORIENTED_EDGE('',*,*,#19118,.T.);
#24997=ORIENTED_EDGE('',*,*,#19092,.T.);
#24998=ORIENTED_EDGE('',*,*,#19119,.T.);
#24999=ORIENTED_EDGE('',*,*,#19107,.F.);
#25000=ORIENTED_EDGE('',*,*,#19111,.F.);
#25001=ORIENTED_EDGE('',*,*,#19101,.F.);
#25002=ORIENTED_EDGE('',*,*,#17790,.F.);
#25003=ORIENTED_EDGE('',*,*,#19102,.F.);
#25004=ORIENTED_EDGE('',*,*,#19112,.F.);
#25005=ORIENTED_EDGE('',*,*,#19118,.F.);
#25006=ORIENTED_EDGE('',*,*,#17792,.F.);
#25007=ORIENTED_EDGE('',*,*,#19108,.F.);
#25008=ORIENTED_EDGE('',*,*,#19117,.F.);
#25009=ORIENTED_EDGE('',*,*,#19113,.F.);
#25010=ORIENTED_EDGE('',*,*,#19110,.F.);
#25011=ORIENTED_EDGE('',*,*,#19120,.T.);
#25012=ORIENTED_EDGE('',*,*,#19121,.T.);
#25013=ORIENTED_EDGE('',*,*,#17801,.T.);
#25014=ORIENTED_EDGE('',*,*,#19122,.T.);
#25015=ORIENTED_EDGE('',*,*,#19123,.T.);
#25016=ORIENTED_EDGE('',*,*,#19121,.F.);
#25017=ORIENTED_EDGE('',*,*,#19124,.F.);
#25018=ORIENTED_EDGE('',*,*,#19125,.F.);
#25019=ORIENTED_EDGE('',*,*,#17802,.F.);
#25020=ORIENTED_EDGE('',*,*,#19120,.F.);
#25021=ORIENTED_EDGE('',*,*,#19126,.F.);
#25022=ORIENTED_EDGE('',*,*,#19127,.T.);
#25023=ORIENTED_EDGE('',*,*,#19128,.T.);
#25024=ORIENTED_EDGE('',*,*,#19124,.T.);
#25025=ORIENTED_EDGE('',*,*,#19123,.F.);
#25026=ORIENTED_EDGE('',*,*,#19129,.T.);
#25027=ORIENTED_EDGE('',*,*,#19130,.T.);
#25028=ORIENTED_EDGE('',*,*,#19131,.T.);
#25029=ORIENTED_EDGE('',*,*,#19126,.T.);
#25030=ORIENTED_EDGE('',*,*,#19128,.F.);
#25031=ORIENTED_EDGE('',*,*,#19132,.F.);
#25032=ORIENTED_EDGE('',*,*,#19133,.F.);
#25033=ORIENTED_EDGE('',*,*,#19130,.F.);
#25034=ORIENTED_EDGE('',*,*,#19134,.F.);
#25035=ORIENTED_EDGE('',*,*,#19135,.F.);
#25036=ORIENTED_EDGE('',*,*,#17799,.T.);
#25037=ORIENTED_EDGE('',*,*,#19136,.T.);
#25038=ORIENTED_EDGE('',*,*,#19134,.T.);
#25039=ORIENTED_EDGE('',*,*,#19137,.T.);
#25040=ORIENTED_EDGE('',*,*,#19138,.F.);
#25041=ORIENTED_EDGE('',*,*,#19139,.F.);
#25042=ORIENTED_EDGE('',*,*,#19140,.F.);
#25043=ORIENTED_EDGE('',*,*,#17797,.T.);
#25044=ORIENTED_EDGE('',*,*,#19141,.T.);
#25045=ORIENTED_EDGE('',*,*,#19139,.T.);
#25046=ORIENTED_EDGE('',*,*,#19142,.T.);
#25047=ORIENTED_EDGE('',*,*,#19132,.T.);
#25048=ORIENTED_EDGE('',*,*,#19143,.T.);
#25049=ORIENTED_EDGE('',*,*,#19140,.T.);
#25050=ORIENTED_EDGE('',*,*,#19144,.T.);
#25051=ORIENTED_EDGE('',*,*,#19138,.T.);
#25052=ORIENTED_EDGE('',*,*,#19145,.T.);
#25053=ORIENTED_EDGE('',*,*,#19135,.T.);
#25054=ORIENTED_EDGE('',*,*,#19146,.T.);
#25055=ORIENTED_EDGE('',*,*,#17803,.T.);
#25056=ORIENTED_EDGE('',*,*,#19125,.T.);
#25057=ORIENTED_EDGE('',*,*,#19133,.T.);
#25058=ORIENTED_EDGE('',*,*,#19147,.T.);
#25059=ORIENTED_EDGE('',*,*,#19122,.F.);
#25060=ORIENTED_EDGE('',*,*,#17800,.F.);
#25061=ORIENTED_EDGE('',*,*,#19137,.F.);
#25062=ORIENTED_EDGE('',*,*,#19129,.F.);
#25063=ORIENTED_EDGE('',*,*,#19143,.F.);
#25064=ORIENTED_EDGE('',*,*,#19127,.F.);
#25065=ORIENTED_EDGE('',*,*,#19131,.F.);
#25066=ORIENTED_EDGE('',*,*,#19145,.F.);
#25067=ORIENTED_EDGE('',*,*,#19148,.F.);
#25068=ORIENTED_EDGE('',*,*,#19149,.F.);
#25069=ORIENTED_EDGE('',*,*,#19150,.F.);
#25070=ORIENTED_EDGE('',*,*,#19151,.F.);
#25071=ORIENTED_EDGE('',*,*,#19152,.F.);
#25072=ORIENTED_EDGE('',*,*,#19153,.F.);
#25073=ORIENTED_EDGE('',*,*,#19154,.F.);
#25074=ORIENTED_EDGE('',*,*,#19155,.F.);
#25075=ORIENTED_EDGE('',*,*,#19156,.F.);
#25076=ORIENTED_EDGE('',*,*,#17807,.T.);
#25077=ORIENTED_EDGE('',*,*,#19157,.T.);
#25078=ORIENTED_EDGE('',*,*,#19155,.T.);
#25079=ORIENTED_EDGE('',*,*,#19158,.T.);
#25080=ORIENTED_EDGE('',*,*,#19159,.F.);
#25081=ORIENTED_EDGE('',*,*,#19160,.F.);
#25082=ORIENTED_EDGE('',*,*,#19161,.F.);
#25083=ORIENTED_EDGE('',*,*,#17805,.T.);
#25084=ORIENTED_EDGE('',*,*,#19162,.T.);
#25085=ORIENTED_EDGE('',*,*,#19160,.T.);
#25086=ORIENTED_EDGE('',*,*,#19163,.T.);
#25087=ORIENTED_EDGE('',*,*,#19152,.T.);
#25088=ORIENTED_EDGE('',*,*,#19164,.T.);
#25089=ORIENTED_EDGE('',*,*,#19161,.T.);
#25090=ORIENTED_EDGE('',*,*,#19165,.T.);
#25091=ORIENTED_EDGE('',*,*,#19159,.T.);
#25092=ORIENTED_EDGE('',*,*,#19166,.T.);
#25093=ORIENTED_EDGE('',*,*,#19156,.T.);
#25094=ORIENTED_EDGE('',*,*,#19167,.T.);
#25095=ORIENTED_EDGE('',*,*,#19149,.T.);
#25096=ORIENTED_EDGE('',*,*,#19168,.T.);
#25097=ORIENTED_EDGE('',*,*,#19154,.T.);
#25098=ORIENTED_EDGE('',*,*,#19169,.T.);
#25099=ORIENTED_EDGE('',*,*,#17811,.T.);
#25100=ORIENTED_EDGE('',*,*,#19170,.T.);
#25101=ORIENTED_EDGE('',*,*,#19153,.T.);
#25102=ORIENTED_EDGE('',*,*,#19171,.T.);
#25103=ORIENTED_EDGE('',*,*,#19151,.T.);
#25104=ORIENTED_EDGE('',*,*,#19172,.T.);
#25105=ORIENTED_EDGE('',*,*,#19150,.T.);
#25106=ORIENTED_EDGE('',*,*,#19173,.T.);
#25107=ORIENTED_EDGE('',*,*,#17809,.T.);
#25108=ORIENTED_EDGE('',*,*,#19174,.T.);
#25109=ORIENTED_EDGE('',*,*,#19148,.T.);
#25110=ORIENTED_EDGE('',*,*,#19175,.T.);
#25111=ORIENTED_EDGE('',*,*,#19163,.F.);
#25112=ORIENTED_EDGE('',*,*,#19167,.F.);
#25113=ORIENTED_EDGE('',*,*,#19157,.F.);
#25114=ORIENTED_EDGE('',*,*,#17806,.F.);
#25115=ORIENTED_EDGE('',*,*,#19158,.F.);
#25116=ORIENTED_EDGE('',*,*,#19168,.F.);
#25117=ORIENTED_EDGE('',*,*,#19174,.F.);
#25118=ORIENTED_EDGE('',*,*,#17808,.F.);
#25119=ORIENTED_EDGE('',*,*,#19164,.F.);
#25120=ORIENTED_EDGE('',*,*,#19173,.F.);
#25121=ORIENTED_EDGE('',*,*,#19169,.F.);
#25122=ORIENTED_EDGE('',*,*,#19166,.F.);
#25123=ORIENTED_EDGE('',*,*,#19176,.F.);
#25124=ORIENTED_EDGE('',*,*,#19177,.F.);
#25125=ORIENTED_EDGE('',*,*,#19178,.F.);
#25126=ORIENTED_EDGE('',*,*,#19179,.T.);
#25127=ORIENTED_EDGE('',*,*,#19180,.T.);
#25128=ORIENTED_EDGE('',*,*,#19177,.T.);
#25129=ORIENTED_EDGE('',*,*,#19181,.T.);
#25130=ORIENTED_EDGE('',*,*,#19182,.T.);
#25131=ORIENTED_EDGE('',*,*,#17819,.T.);
#25132=ORIENTED_EDGE('',*,*,#19183,.T.);
#25133=ORIENTED_EDGE('',*,*,#19178,.T.);
#25134=ORIENTED_EDGE('',*,*,#19184,.T.);
#25135=ORIENTED_EDGE('',*,*,#19185,.F.);
#25136=ORIENTED_EDGE('',*,*,#19186,.F.);
#25137=ORIENTED_EDGE('',*,*,#19187,.F.);
#25138=ORIENTED_EDGE('',*,*,#19188,.T.);
#25139=ORIENTED_EDGE('',*,*,#19189,.T.);
#25140=ORIENTED_EDGE('',*,*,#19186,.T.);
#25141=ORIENTED_EDGE('',*,*,#19190,.T.);
#25142=ORIENTED_EDGE('',*,*,#19191,.T.);
#25143=ORIENTED_EDGE('',*,*,#19176,.T.);
#25144=ORIENTED_EDGE('',*,*,#19192,.T.);
#25145=ORIENTED_EDGE('',*,*,#19187,.T.);
#25146=ORIENTED_EDGE('',*,*,#19193,.T.);
#25147=ORIENTED_EDGE('',*,*,#17817,.T.);
#25148=ORIENTED_EDGE('',*,*,#19194,.T.);
#25149=ORIENTED_EDGE('',*,*,#19185,.T.);
#25150=ORIENTED_EDGE('',*,*,#19195,.T.);
#25151=ORIENTED_EDGE('',*,*,#19179,.F.);
#25152=ORIENTED_EDGE('',*,*,#19196,.T.);
#25153=ORIENTED_EDGE('',*,*,#19197,.T.);
#25154=ORIENTED_EDGE('',*,*,#17813,.T.);
#25155=ORIENTED_EDGE('',*,*,#19198,.T.);
#25156=ORIENTED_EDGE('',*,*,#19181,.F.);
#25157=ORIENTED_EDGE('',*,*,#19193,.F.);
#25158=ORIENTED_EDGE('',*,*,#19189,.F.);
#25159=ORIENTED_EDGE('',*,*,#19199,.F.);
#25160=ORIENTED_EDGE('',*,*,#19182,.F.);
#25161=ORIENTED_EDGE('',*,*,#19199,.T.);
#25162=ORIENTED_EDGE('',*,*,#19188,.F.);
#25163=ORIENTED_EDGE('',*,*,#19200,.F.);
#25164=ORIENTED_EDGE('',*,*,#19201,.T.);
#25165=ORIENTED_EDGE('',*,*,#19196,.F.);
#25166=ORIENTED_EDGE('',*,*,#19191,.F.);
#25167=ORIENTED_EDGE('',*,*,#19202,.T.);
#25168=ORIENTED_EDGE('',*,*,#17815,.T.);
#25169=ORIENTED_EDGE('',*,*,#19203,.T.);
#25170=ORIENTED_EDGE('',*,*,#19200,.T.);
#25171=ORIENTED_EDGE('',*,*,#19190,.F.);
#25172=ORIENTED_EDGE('',*,*,#19194,.F.);
#25173=ORIENTED_EDGE('',*,*,#17816,.F.);
#25174=ORIENTED_EDGE('',*,*,#19202,.F.);
#25175=ORIENTED_EDGE('',*,*,#19180,.F.);
#25176=ORIENTED_EDGE('',*,*,#19198,.F.);
#25177=ORIENTED_EDGE('',*,*,#17812,.F.);
#25178=ORIENTED_EDGE('',*,*,#19184,.F.);
#25179=ORIENTED_EDGE('',*,*,#19204,.F.);
#25180=ORIENTED_EDGE('',*,*,#19205,.F.);
#25181=ORIENTED_EDGE('',*,*,#19206,.F.);
#25182=ORIENTED_EDGE('',*,*,#19207,.F.);
#25183=ORIENTED_EDGE('',*,*,#19208,.F.);
#25184=ORIENTED_EDGE('',*,*,#19209,.F.);
#25185=ORIENTED_EDGE('',*,*,#19210,.F.);
#25186=ORIENTED_EDGE('',*,*,#19211,.F.);
#25187=ORIENTED_EDGE('',*,*,#19212,.F.);
#25188=ORIENTED_EDGE('',*,*,#17823,.T.);
#25189=ORIENTED_EDGE('',*,*,#19213,.T.);
#25190=ORIENTED_EDGE('',*,*,#19211,.T.);
#25191=ORIENTED_EDGE('',*,*,#19214,.T.);
#25192=ORIENTED_EDGE('',*,*,#19215,.F.);
#25193=ORIENTED_EDGE('',*,*,#19216,.F.);
#25194=ORIENTED_EDGE('',*,*,#19217,.F.);
#25195=ORIENTED_EDGE('',*,*,#17821,.T.);
#25196=ORIENTED_EDGE('',*,*,#19218,.T.);
#25197=ORIENTED_EDGE('',*,*,#19216,.T.);
#25198=ORIENTED_EDGE('',*,*,#19219,.T.);
#25199=ORIENTED_EDGE('',*,*,#19208,.T.);
#25200=ORIENTED_EDGE('',*,*,#19220,.T.);
#25201=ORIENTED_EDGE('',*,*,#19217,.T.);
#25202=ORIENTED_EDGE('',*,*,#19221,.T.);
#25203=ORIENTED_EDGE('',*,*,#19215,.T.);
#25204=ORIENTED_EDGE('',*,*,#19222,.T.);
#25205=ORIENTED_EDGE('',*,*,#19212,.T.);
#25206=ORIENTED_EDGE('',*,*,#19223,.T.);
#25207=ORIENTED_EDGE('',*,*,#19205,.T.);
#25208=ORIENTED_EDGE('',*,*,#19224,.T.);
#25209=ORIENTED_EDGE('',*,*,#19210,.T.);
#25210=ORIENTED_EDGE('',*,*,#19225,.T.);
#25211=ORIENTED_EDGE('',*,*,#17827,.T.);
#25212=ORIENTED_EDGE('',*,*,#19226,.T.);
#25213=ORIENTED_EDGE('',*,*,#19209,.T.);
#25214=ORIENTED_EDGE('',*,*,#19227,.T.);
#25215=ORIENTED_EDGE('',*,*,#19207,.T.);
#25216=ORIENTED_EDGE('',*,*,#19228,.T.);
#25217=ORIENTED_EDGE('',*,*,#19206,.T.);
#25218=ORIENTED_EDGE('',*,*,#19229,.T.);
#25219=ORIENTED_EDGE('',*,*,#17825,.T.);
#25220=ORIENTED_EDGE('',*,*,#19230,.T.);
#25221=ORIENTED_EDGE('',*,*,#19204,.T.);
#25222=ORIENTED_EDGE('',*,*,#19231,.T.);
#25223=ORIENTED_EDGE('',*,*,#19219,.F.);
#25224=ORIENTED_EDGE('',*,*,#19223,.F.);
#25225=ORIENTED_EDGE('',*,*,#19213,.F.);
#25226=ORIENTED_EDGE('',*,*,#17822,.F.);
#25227=ORIENTED_EDGE('',*,*,#19214,.F.);
#25228=ORIENTED_EDGE('',*,*,#19224,.F.);
#25229=ORIENTED_EDGE('',*,*,#19230,.F.);
#25230=ORIENTED_EDGE('',*,*,#17824,.F.);
#25231=ORIENTED_EDGE('',*,*,#19220,.F.);
#25232=ORIENTED_EDGE('',*,*,#19229,.F.);
#25233=ORIENTED_EDGE('',*,*,#19225,.F.);
#25234=ORIENTED_EDGE('',*,*,#19222,.F.);
#25235=ORIENTED_EDGE('',*,*,#19232,.F.);
#25236=ORIENTED_EDGE('',*,*,#19233,.F.);
#25237=ORIENTED_EDGE('',*,*,#19234,.F.);
#25238=ORIENTED_EDGE('',*,*,#19235,.F.);
#25239=ORIENTED_EDGE('',*,*,#19236,.F.);
#25240=ORIENTED_EDGE('',*,*,#19237,.F.);
#25241=ORIENTED_EDGE('',*,*,#19238,.F.);
#25242=ORIENTED_EDGE('',*,*,#19239,.F.);
#25243=ORIENTED_EDGE('',*,*,#19240,.F.);
#25244=ORIENTED_EDGE('',*,*,#17831,.T.);
#25245=ORIENTED_EDGE('',*,*,#19241,.T.);
#25246=ORIENTED_EDGE('',*,*,#19239,.T.);
#25247=ORIENTED_EDGE('',*,*,#19242,.T.);
#25248=ORIENTED_EDGE('',*,*,#19243,.F.);
#25249=ORIENTED_EDGE('',*,*,#19244,.F.);
#25250=ORIENTED_EDGE('',*,*,#19245,.F.);
#25251=ORIENTED_EDGE('',*,*,#17829,.T.);
#25252=ORIENTED_EDGE('',*,*,#19246,.T.);
#25253=ORIENTED_EDGE('',*,*,#19244,.T.);
#25254=ORIENTED_EDGE('',*,*,#19247,.T.);
#25255=ORIENTED_EDGE('',*,*,#19236,.T.);
#25256=ORIENTED_EDGE('',*,*,#19248,.T.);
#25257=ORIENTED_EDGE('',*,*,#19245,.T.);
#25258=ORIENTED_EDGE('',*,*,#19249,.T.);
#25259=ORIENTED_EDGE('',*,*,#19243,.T.);
#25260=ORIENTED_EDGE('',*,*,#19250,.T.);
#25261=ORIENTED_EDGE('',*,*,#19240,.T.);
#25262=ORIENTED_EDGE('',*,*,#19251,.T.);
#25263=ORIENTED_EDGE('',*,*,#19233,.T.);
#25264=ORIENTED_EDGE('',*,*,#19252,.T.);
#25265=ORIENTED_EDGE('',*,*,#19238,.T.);
#25266=ORIENTED_EDGE('',*,*,#19253,.T.);
#25267=ORIENTED_EDGE('',*,*,#17835,.T.);
#25268=ORIENTED_EDGE('',*,*,#19254,.T.);
#25269=ORIENTED_EDGE('',*,*,#19237,.T.);
#25270=ORIENTED_EDGE('',*,*,#19255,.T.);
#25271=ORIENTED_EDGE('',*,*,#19235,.T.);
#25272=ORIENTED_EDGE('',*,*,#19256,.T.);
#25273=ORIENTED_EDGE('',*,*,#19234,.T.);
#25274=ORIENTED_EDGE('',*,*,#19257,.T.);
#25275=ORIENTED_EDGE('',*,*,#17833,.T.);
#25276=ORIENTED_EDGE('',*,*,#19258,.T.);
#25277=ORIENTED_EDGE('',*,*,#19232,.T.);
#25278=ORIENTED_EDGE('',*,*,#19259,.T.);
#25279=ORIENTED_EDGE('',*,*,#19247,.F.);
#25280=ORIENTED_EDGE('',*,*,#19251,.F.);
#25281=ORIENTED_EDGE('',*,*,#19241,.F.);
#25282=ORIENTED_EDGE('',*,*,#17830,.F.);
#25283=ORIENTED_EDGE('',*,*,#19242,.F.);
#25284=ORIENTED_EDGE('',*,*,#19252,.F.);
#25285=ORIENTED_EDGE('',*,*,#19258,.F.);
#25286=ORIENTED_EDGE('',*,*,#17832,.F.);
#25287=ORIENTED_EDGE('',*,*,#19248,.F.);
#25288=ORIENTED_EDGE('',*,*,#19257,.F.);
#25289=ORIENTED_EDGE('',*,*,#19253,.F.);
#25290=ORIENTED_EDGE('',*,*,#19250,.F.);
#25291=ORIENTED_EDGE('',*,*,#19260,.T.);
#25292=ORIENTED_EDGE('',*,*,#19261,.T.);
#25293=ORIENTED_EDGE('',*,*,#17841,.T.);
#25294=ORIENTED_EDGE('',*,*,#19262,.T.);
#25295=ORIENTED_EDGE('',*,*,#19263,.T.);
#25296=ORIENTED_EDGE('',*,*,#19261,.F.);
#25297=ORIENTED_EDGE('',*,*,#19264,.F.);
#25298=ORIENTED_EDGE('',*,*,#19265,.F.);
#25299=ORIENTED_EDGE('',*,*,#17842,.F.);
#25300=ORIENTED_EDGE('',*,*,#19260,.F.);
#25301=ORIENTED_EDGE('',*,*,#19266,.F.);
#25302=ORIENTED_EDGE('',*,*,#19267,.T.);
#25303=ORIENTED_EDGE('',*,*,#19268,.T.);
#25304=ORIENTED_EDGE('',*,*,#19264,.T.);
#25305=ORIENTED_EDGE('',*,*,#19263,.F.);
#25306=ORIENTED_EDGE('',*,*,#19269,.T.);
#25307=ORIENTED_EDGE('',*,*,#19270,.T.);
#25308=ORIENTED_EDGE('',*,*,#19271,.T.);
#25309=ORIENTED_EDGE('',*,*,#19266,.T.);
#25310=ORIENTED_EDGE('',*,*,#19268,.F.);
#25311=ORIENTED_EDGE('',*,*,#19272,.F.);
#25312=ORIENTED_EDGE('',*,*,#19273,.F.);
#25313=ORIENTED_EDGE('',*,*,#19270,.F.);
#25314=ORIENTED_EDGE('',*,*,#19274,.F.);
#25315=ORIENTED_EDGE('',*,*,#19275,.F.);
#25316=ORIENTED_EDGE('',*,*,#17839,.T.);
#25317=ORIENTED_EDGE('',*,*,#19276,.T.);
#25318=ORIENTED_EDGE('',*,*,#19274,.T.);
#25319=ORIENTED_EDGE('',*,*,#19277,.T.);
#25320=ORIENTED_EDGE('',*,*,#19278,.F.);
#25321=ORIENTED_EDGE('',*,*,#19279,.F.);
#25322=ORIENTED_EDGE('',*,*,#19280,.F.);
#25323=ORIENTED_EDGE('',*,*,#17837,.T.);
#25324=ORIENTED_EDGE('',*,*,#19281,.T.);
#25325=ORIENTED_EDGE('',*,*,#19279,.T.);
#25326=ORIENTED_EDGE('',*,*,#19282,.T.);
#25327=ORIENTED_EDGE('',*,*,#19272,.T.);
#25328=ORIENTED_EDGE('',*,*,#19283,.T.);
#25329=ORIENTED_EDGE('',*,*,#19280,.T.);
#25330=ORIENTED_EDGE('',*,*,#19284,.T.);
#25331=ORIENTED_EDGE('',*,*,#19278,.T.);
#25332=ORIENTED_EDGE('',*,*,#19285,.T.);
#25333=ORIENTED_EDGE('',*,*,#19275,.T.);
#25334=ORIENTED_EDGE('',*,*,#19286,.T.);
#25335=ORIENTED_EDGE('',*,*,#17843,.T.);
#25336=ORIENTED_EDGE('',*,*,#19265,.T.);
#25337=ORIENTED_EDGE('',*,*,#19273,.T.);
#25338=ORIENTED_EDGE('',*,*,#19287,.T.);
#25339=ORIENTED_EDGE('',*,*,#19262,.F.);
#25340=ORIENTED_EDGE('',*,*,#17840,.F.);
#25341=ORIENTED_EDGE('',*,*,#19277,.F.);
#25342=ORIENTED_EDGE('',*,*,#19269,.F.);
#25343=ORIENTED_EDGE('',*,*,#19283,.F.);
#25344=ORIENTED_EDGE('',*,*,#19267,.F.);
#25345=ORIENTED_EDGE('',*,*,#19271,.F.);
#25346=ORIENTED_EDGE('',*,*,#19285,.F.);
#25347=ORIENTED_EDGE('',*,*,#19288,.F.);
#25348=ORIENTED_EDGE('',*,*,#19289,.F.);
#25349=ORIENTED_EDGE('',*,*,#19290,.F.);
#25350=ORIENTED_EDGE('',*,*,#19291,.F.);
#25351=ORIENTED_EDGE('',*,*,#19292,.F.);
#25352=ORIENTED_EDGE('',*,*,#19293,.F.);
#25353=ORIENTED_EDGE('',*,*,#19294,.F.);
#25354=ORIENTED_EDGE('',*,*,#19295,.F.);
#25355=ORIENTED_EDGE('',*,*,#19296,.F.);
#25356=ORIENTED_EDGE('',*,*,#17847,.T.);
#25357=ORIENTED_EDGE('',*,*,#19297,.T.);
#25358=ORIENTED_EDGE('',*,*,#19295,.T.);
#25359=ORIENTED_EDGE('',*,*,#19298,.T.);
#25360=ORIENTED_EDGE('',*,*,#19299,.F.);
#25361=ORIENTED_EDGE('',*,*,#19300,.F.);
#25362=ORIENTED_EDGE('',*,*,#19301,.F.);
#25363=ORIENTED_EDGE('',*,*,#17845,.T.);
#25364=ORIENTED_EDGE('',*,*,#19302,.T.);
#25365=ORIENTED_EDGE('',*,*,#19300,.T.);
#25366=ORIENTED_EDGE('',*,*,#19303,.T.);
#25367=ORIENTED_EDGE('',*,*,#19292,.T.);
#25368=ORIENTED_EDGE('',*,*,#19304,.T.);
#25369=ORIENTED_EDGE('',*,*,#19301,.T.);
#25370=ORIENTED_EDGE('',*,*,#19305,.T.);
#25371=ORIENTED_EDGE('',*,*,#19299,.T.);
#25372=ORIENTED_EDGE('',*,*,#19306,.T.);
#25373=ORIENTED_EDGE('',*,*,#19296,.T.);
#25374=ORIENTED_EDGE('',*,*,#19307,.T.);
#25375=ORIENTED_EDGE('',*,*,#19289,.T.);
#25376=ORIENTED_EDGE('',*,*,#19308,.T.);
#25377=ORIENTED_EDGE('',*,*,#19294,.T.);
#25378=ORIENTED_EDGE('',*,*,#19309,.T.);
#25379=ORIENTED_EDGE('',*,*,#17851,.T.);
#25380=ORIENTED_EDGE('',*,*,#19310,.T.);
#25381=ORIENTED_EDGE('',*,*,#19293,.T.);
#25382=ORIENTED_EDGE('',*,*,#19311,.T.);
#25383=ORIENTED_EDGE('',*,*,#19291,.T.);
#25384=ORIENTED_EDGE('',*,*,#19312,.T.);
#25385=ORIENTED_EDGE('',*,*,#19290,.T.);
#25386=ORIENTED_EDGE('',*,*,#19313,.T.);
#25387=ORIENTED_EDGE('',*,*,#17849,.T.);
#25388=ORIENTED_EDGE('',*,*,#19314,.T.);
#25389=ORIENTED_EDGE('',*,*,#19288,.T.);
#25390=ORIENTED_EDGE('',*,*,#19315,.T.);
#25391=ORIENTED_EDGE('',*,*,#19303,.F.);
#25392=ORIENTED_EDGE('',*,*,#19307,.F.);
#25393=ORIENTED_EDGE('',*,*,#19297,.F.);
#25394=ORIENTED_EDGE('',*,*,#17846,.F.);
#25395=ORIENTED_EDGE('',*,*,#19298,.F.);
#25396=ORIENTED_EDGE('',*,*,#19308,.F.);
#25397=ORIENTED_EDGE('',*,*,#19314,.F.);
#25398=ORIENTED_EDGE('',*,*,#17848,.F.);
#25399=ORIENTED_EDGE('',*,*,#19304,.F.);
#25400=ORIENTED_EDGE('',*,*,#19313,.F.);
#25401=ORIENTED_EDGE('',*,*,#19309,.F.);
#25402=ORIENTED_EDGE('',*,*,#19306,.F.);
#25403=ORIENTED_EDGE('',*,*,#19316,.F.);
#25404=ORIENTED_EDGE('',*,*,#19317,.F.);
#25405=ORIENTED_EDGE('',*,*,#19318,.F.);
#25406=ORIENTED_EDGE('',*,*,#19319,.T.);
#25407=ORIENTED_EDGE('',*,*,#19320,.T.);
#25408=ORIENTED_EDGE('',*,*,#19317,.T.);
#25409=ORIENTED_EDGE('',*,*,#19321,.T.);
#25410=ORIENTED_EDGE('',*,*,#19322,.T.);
#25411=ORIENTED_EDGE('',*,*,#17859,.T.);
#25412=ORIENTED_EDGE('',*,*,#19323,.T.);
#25413=ORIENTED_EDGE('',*,*,#19318,.T.);
#25414=ORIENTED_EDGE('',*,*,#19324,.T.);
#25415=ORIENTED_EDGE('',*,*,#19325,.F.);
#25416=ORIENTED_EDGE('',*,*,#19326,.F.);
#25417=ORIENTED_EDGE('',*,*,#19327,.F.);
#25418=ORIENTED_EDGE('',*,*,#19328,.T.);
#25419=ORIENTED_EDGE('',*,*,#19329,.T.);
#25420=ORIENTED_EDGE('',*,*,#19326,.T.);
#25421=ORIENTED_EDGE('',*,*,#19330,.T.);
#25422=ORIENTED_EDGE('',*,*,#19331,.T.);
#25423=ORIENTED_EDGE('',*,*,#19316,.T.);
#25424=ORIENTED_EDGE('',*,*,#19332,.T.);
#25425=ORIENTED_EDGE('',*,*,#19327,.T.);
#25426=ORIENTED_EDGE('',*,*,#19333,.T.);
#25427=ORIENTED_EDGE('',*,*,#17857,.T.);
#25428=ORIENTED_EDGE('',*,*,#19334,.T.);
#25429=ORIENTED_EDGE('',*,*,#19325,.T.);
#25430=ORIENTED_EDGE('',*,*,#19335,.T.);
#25431=ORIENTED_EDGE('',*,*,#19319,.F.);
#25432=ORIENTED_EDGE('',*,*,#19336,.T.);
#25433=ORIENTED_EDGE('',*,*,#19337,.T.);
#25434=ORIENTED_EDGE('',*,*,#17853,.T.);
#25435=ORIENTED_EDGE('',*,*,#19338,.T.);
#25436=ORIENTED_EDGE('',*,*,#19321,.F.);
#25437=ORIENTED_EDGE('',*,*,#19333,.F.);
#25438=ORIENTED_EDGE('',*,*,#19329,.F.);
#25439=ORIENTED_EDGE('',*,*,#19339,.F.);
#25440=ORIENTED_EDGE('',*,*,#19322,.F.);
#25441=ORIENTED_EDGE('',*,*,#19339,.T.);
#25442=ORIENTED_EDGE('',*,*,#19328,.F.);
#25443=ORIENTED_EDGE('',*,*,#19340,.F.);
#25444=ORIENTED_EDGE('',*,*,#19341,.T.);
#25445=ORIENTED_EDGE('',*,*,#19336,.F.);
#25446=ORIENTED_EDGE('',*,*,#19331,.F.);
#25447=ORIENTED_EDGE('',*,*,#19342,.T.);
#25448=ORIENTED_EDGE('',*,*,#17855,.T.);
#25449=ORIENTED_EDGE('',*,*,#19343,.T.);
#25450=ORIENTED_EDGE('',*,*,#19340,.T.);
#25451=ORIENTED_EDGE('',*,*,#19330,.F.);
#25452=ORIENTED_EDGE('',*,*,#19334,.F.);
#25453=ORIENTED_EDGE('',*,*,#17856,.F.);
#25454=ORIENTED_EDGE('',*,*,#19342,.F.);
#25455=ORIENTED_EDGE('',*,*,#19320,.F.);
#25456=ORIENTED_EDGE('',*,*,#19338,.F.);
#25457=ORIENTED_EDGE('',*,*,#17852,.F.);
#25458=ORIENTED_EDGE('',*,*,#19324,.F.);
#25459=ORIENTED_EDGE('',*,*,#19344,.F.);
#25460=ORIENTED_EDGE('',*,*,#19345,.F.);
#25461=ORIENTED_EDGE('',*,*,#19346,.F.);
#25462=ORIENTED_EDGE('',*,*,#19347,.F.);
#25463=ORIENTED_EDGE('',*,*,#19348,.F.);
#25464=ORIENTED_EDGE('',*,*,#19349,.F.);
#25465=ORIENTED_EDGE('',*,*,#19350,.F.);
#25466=ORIENTED_EDGE('',*,*,#19351,.F.);
#25467=ORIENTED_EDGE('',*,*,#19352,.F.);
#25468=ORIENTED_EDGE('',*,*,#17863,.T.);
#25469=ORIENTED_EDGE('',*,*,#19353,.T.);
#25470=ORIENTED_EDGE('',*,*,#19351,.T.);
#25471=ORIENTED_EDGE('',*,*,#19354,.T.);
#25472=ORIENTED_EDGE('',*,*,#19355,.F.);
#25473=ORIENTED_EDGE('',*,*,#19356,.F.);
#25474=ORIENTED_EDGE('',*,*,#19357,.F.);
#25475=ORIENTED_EDGE('',*,*,#17861,.T.);
#25476=ORIENTED_EDGE('',*,*,#19358,.T.);
#25477=ORIENTED_EDGE('',*,*,#19356,.T.);
#25478=ORIENTED_EDGE('',*,*,#19359,.T.);
#25479=ORIENTED_EDGE('',*,*,#19348,.T.);
#25480=ORIENTED_EDGE('',*,*,#19360,.T.);
#25481=ORIENTED_EDGE('',*,*,#19357,.T.);
#25482=ORIENTED_EDGE('',*,*,#19361,.T.);
#25483=ORIENTED_EDGE('',*,*,#19355,.T.);
#25484=ORIENTED_EDGE('',*,*,#19362,.T.);
#25485=ORIENTED_EDGE('',*,*,#19352,.T.);
#25486=ORIENTED_EDGE('',*,*,#19363,.T.);
#25487=ORIENTED_EDGE('',*,*,#19345,.T.);
#25488=ORIENTED_EDGE('',*,*,#19364,.T.);
#25489=ORIENTED_EDGE('',*,*,#19350,.T.);
#25490=ORIENTED_EDGE('',*,*,#19365,.T.);
#25491=ORIENTED_EDGE('',*,*,#17867,.T.);
#25492=ORIENTED_EDGE('',*,*,#19366,.T.);
#25493=ORIENTED_EDGE('',*,*,#19349,.T.);
#25494=ORIENTED_EDGE('',*,*,#19367,.T.);
#25495=ORIENTED_EDGE('',*,*,#19347,.T.);
#25496=ORIENTED_EDGE('',*,*,#19368,.T.);
#25497=ORIENTED_EDGE('',*,*,#19346,.T.);
#25498=ORIENTED_EDGE('',*,*,#19369,.T.);
#25499=ORIENTED_EDGE('',*,*,#17865,.T.);
#25500=ORIENTED_EDGE('',*,*,#19370,.T.);
#25501=ORIENTED_EDGE('',*,*,#19344,.T.);
#25502=ORIENTED_EDGE('',*,*,#19371,.T.);
#25503=ORIENTED_EDGE('',*,*,#19359,.F.);
#25504=ORIENTED_EDGE('',*,*,#19363,.F.);
#25505=ORIENTED_EDGE('',*,*,#19353,.F.);
#25506=ORIENTED_EDGE('',*,*,#17862,.F.);
#25507=ORIENTED_EDGE('',*,*,#19354,.F.);
#25508=ORIENTED_EDGE('',*,*,#19364,.F.);
#25509=ORIENTED_EDGE('',*,*,#19370,.F.);
#25510=ORIENTED_EDGE('',*,*,#17864,.F.);
#25511=ORIENTED_EDGE('',*,*,#19360,.F.);
#25512=ORIENTED_EDGE('',*,*,#19369,.F.);
#25513=ORIENTED_EDGE('',*,*,#19365,.F.);
#25514=ORIENTED_EDGE('',*,*,#19362,.F.);
#25515=ORIENTED_EDGE('',*,*,#19372,.F.);
#25516=ORIENTED_EDGE('',*,*,#19373,.F.);
#25517=ORIENTED_EDGE('',*,*,#19374,.F.);
#25518=ORIENTED_EDGE('',*,*,#19375,.F.);
#25519=ORIENTED_EDGE('',*,*,#19376,.F.);
#25520=ORIENTED_EDGE('',*,*,#19377,.F.);
#25521=ORIENTED_EDGE('',*,*,#19378,.F.);
#25522=ORIENTED_EDGE('',*,*,#19379,.F.);
#25523=ORIENTED_EDGE('',*,*,#19380,.F.);
#25524=ORIENTED_EDGE('',*,*,#17871,.T.);
#25525=ORIENTED_EDGE('',*,*,#19381,.T.);
#25526=ORIENTED_EDGE('',*,*,#19379,.T.);
#25527=ORIENTED_EDGE('',*,*,#19382,.T.);
#25528=ORIENTED_EDGE('',*,*,#19383,.F.);
#25529=ORIENTED_EDGE('',*,*,#19384,.F.);
#25530=ORIENTED_EDGE('',*,*,#19385,.F.);
#25531=ORIENTED_EDGE('',*,*,#17869,.T.);
#25532=ORIENTED_EDGE('',*,*,#19386,.T.);
#25533=ORIENTED_EDGE('',*,*,#19384,.T.);
#25534=ORIENTED_EDGE('',*,*,#19387,.T.);
#25535=ORIENTED_EDGE('',*,*,#19376,.T.);
#25536=ORIENTED_EDGE('',*,*,#19388,.T.);
#25537=ORIENTED_EDGE('',*,*,#19385,.T.);
#25538=ORIENTED_EDGE('',*,*,#19389,.T.);
#25539=ORIENTED_EDGE('',*,*,#19383,.T.);
#25540=ORIENTED_EDGE('',*,*,#19390,.T.);
#25541=ORIENTED_EDGE('',*,*,#19380,.T.);
#25542=ORIENTED_EDGE('',*,*,#19391,.T.);
#25543=ORIENTED_EDGE('',*,*,#19373,.T.);
#25544=ORIENTED_EDGE('',*,*,#19392,.T.);
#25545=ORIENTED_EDGE('',*,*,#19378,.T.);
#25546=ORIENTED_EDGE('',*,*,#19393,.T.);
#25547=ORIENTED_EDGE('',*,*,#17875,.T.);
#25548=ORIENTED_EDGE('',*,*,#19394,.T.);
#25549=ORIENTED_EDGE('',*,*,#19377,.T.);
#25550=ORIENTED_EDGE('',*,*,#19395,.T.);
#25551=ORIENTED_EDGE('',*,*,#19375,.T.);
#25552=ORIENTED_EDGE('',*,*,#19396,.T.);
#25553=ORIENTED_EDGE('',*,*,#19374,.T.);
#25554=ORIENTED_EDGE('',*,*,#19397,.T.);
#25555=ORIENTED_EDGE('',*,*,#17873,.T.);
#25556=ORIENTED_EDGE('',*,*,#19398,.T.);
#25557=ORIENTED_EDGE('',*,*,#19372,.T.);
#25558=ORIENTED_EDGE('',*,*,#19399,.T.);
#25559=ORIENTED_EDGE('',*,*,#19387,.F.);
#25560=ORIENTED_EDGE('',*,*,#19391,.F.);
#25561=ORIENTED_EDGE('',*,*,#19381,.F.);
#25562=ORIENTED_EDGE('',*,*,#17870,.F.);
#25563=ORIENTED_EDGE('',*,*,#19382,.F.);
#25564=ORIENTED_EDGE('',*,*,#19392,.F.);
#25565=ORIENTED_EDGE('',*,*,#19398,.F.);
#25566=ORIENTED_EDGE('',*,*,#17872,.F.);
#25567=ORIENTED_EDGE('',*,*,#19388,.F.);
#25568=ORIENTED_EDGE('',*,*,#19397,.F.);
#25569=ORIENTED_EDGE('',*,*,#19393,.F.);
#25570=ORIENTED_EDGE('',*,*,#19390,.F.);
#25571=ORIENTED_EDGE('',*,*,#19400,.T.);
#25572=ORIENTED_EDGE('',*,*,#19401,.T.);
#25573=ORIENTED_EDGE('',*,*,#17881,.T.);
#25574=ORIENTED_EDGE('',*,*,#19402,.T.);
#25575=ORIENTED_EDGE('',*,*,#19403,.T.);
#25576=ORIENTED_EDGE('',*,*,#19401,.F.);
#25577=ORIENTED_EDGE('',*,*,#19404,.F.);
#25578=ORIENTED_EDGE('',*,*,#19405,.F.);
#25579=ORIENTED_EDGE('',*,*,#17882,.F.);
#25580=ORIENTED_EDGE('',*,*,#19400,.F.);
#25581=ORIENTED_EDGE('',*,*,#19406,.F.);
#25582=ORIENTED_EDGE('',*,*,#19407,.T.);
#25583=ORIENTED_EDGE('',*,*,#19408,.T.);
#25584=ORIENTED_EDGE('',*,*,#19404,.T.);
#25585=ORIENTED_EDGE('',*,*,#19403,.F.);
#25586=ORIENTED_EDGE('',*,*,#19409,.T.);
#25587=ORIENTED_EDGE('',*,*,#19410,.T.);
#25588=ORIENTED_EDGE('',*,*,#19411,.T.);
#25589=ORIENTED_EDGE('',*,*,#19406,.T.);
#25590=ORIENTED_EDGE('',*,*,#19408,.F.);
#25591=ORIENTED_EDGE('',*,*,#19412,.F.);
#25592=ORIENTED_EDGE('',*,*,#19413,.F.);
#25593=ORIENTED_EDGE('',*,*,#19410,.F.);
#25594=ORIENTED_EDGE('',*,*,#19414,.F.);
#25595=ORIENTED_EDGE('',*,*,#19415,.F.);
#25596=ORIENTED_EDGE('',*,*,#17879,.T.);
#25597=ORIENTED_EDGE('',*,*,#19416,.T.);
#25598=ORIENTED_EDGE('',*,*,#19414,.T.);
#25599=ORIENTED_EDGE('',*,*,#19417,.T.);
#25600=ORIENTED_EDGE('',*,*,#19418,.F.);
#25601=ORIENTED_EDGE('',*,*,#19419,.F.);
#25602=ORIENTED_EDGE('',*,*,#19420,.F.);
#25603=ORIENTED_EDGE('',*,*,#17877,.T.);
#25604=ORIENTED_EDGE('',*,*,#19421,.T.);
#25605=ORIENTED_EDGE('',*,*,#19419,.T.);
#25606=ORIENTED_EDGE('',*,*,#19422,.T.);
#25607=ORIENTED_EDGE('',*,*,#19412,.T.);
#25608=ORIENTED_EDGE('',*,*,#19423,.T.);
#25609=ORIENTED_EDGE('',*,*,#19420,.T.);
#25610=ORIENTED_EDGE('',*,*,#19424,.T.);
#25611=ORIENTED_EDGE('',*,*,#19418,.T.);
#25612=ORIENTED_EDGE('',*,*,#19425,.T.);
#25613=ORIENTED_EDGE('',*,*,#19415,.T.);
#25614=ORIENTED_EDGE('',*,*,#19426,.T.);
#25615=ORIENTED_EDGE('',*,*,#17883,.T.);
#25616=ORIENTED_EDGE('',*,*,#19405,.T.);
#25617=ORIENTED_EDGE('',*,*,#19413,.T.);
#25618=ORIENTED_EDGE('',*,*,#19427,.T.);
#25619=ORIENTED_EDGE('',*,*,#19402,.F.);
#25620=ORIENTED_EDGE('',*,*,#17880,.F.);
#25621=ORIENTED_EDGE('',*,*,#19417,.F.);
#25622=ORIENTED_EDGE('',*,*,#19409,.F.);
#25623=ORIENTED_EDGE('',*,*,#19423,.F.);
#25624=ORIENTED_EDGE('',*,*,#19407,.F.);
#25625=ORIENTED_EDGE('',*,*,#19411,.F.);
#25626=ORIENTED_EDGE('',*,*,#19425,.F.);
#25627=ORIENTED_EDGE('',*,*,#19428,.F.);
#25628=ORIENTED_EDGE('',*,*,#19429,.F.);
#25629=ORIENTED_EDGE('',*,*,#19430,.F.);
#25630=ORIENTED_EDGE('',*,*,#19431,.F.);
#25631=ORIENTED_EDGE('',*,*,#19432,.F.);
#25632=ORIENTED_EDGE('',*,*,#19433,.F.);
#25633=ORIENTED_EDGE('',*,*,#19434,.F.);
#25634=ORIENTED_EDGE('',*,*,#19435,.F.);
#25635=ORIENTED_EDGE('',*,*,#19436,.F.);
#25636=ORIENTED_EDGE('',*,*,#17887,.T.);
#25637=ORIENTED_EDGE('',*,*,#19437,.T.);
#25638=ORIENTED_EDGE('',*,*,#19435,.T.);
#25639=ORIENTED_EDGE('',*,*,#19438,.T.);
#25640=ORIENTED_EDGE('',*,*,#19439,.F.);
#25641=ORIENTED_EDGE('',*,*,#19440,.F.);
#25642=ORIENTED_EDGE('',*,*,#19441,.F.);
#25643=ORIENTED_EDGE('',*,*,#17885,.T.);
#25644=ORIENTED_EDGE('',*,*,#19442,.T.);
#25645=ORIENTED_EDGE('',*,*,#19440,.T.);
#25646=ORIENTED_EDGE('',*,*,#19443,.T.);
#25647=ORIENTED_EDGE('',*,*,#19432,.T.);
#25648=ORIENTED_EDGE('',*,*,#19444,.T.);
#25649=ORIENTED_EDGE('',*,*,#19441,.T.);
#25650=ORIENTED_EDGE('',*,*,#19445,.T.);
#25651=ORIENTED_EDGE('',*,*,#19439,.T.);
#25652=ORIENTED_EDGE('',*,*,#19446,.T.);
#25653=ORIENTED_EDGE('',*,*,#19436,.T.);
#25654=ORIENTED_EDGE('',*,*,#19447,.T.);
#25655=ORIENTED_EDGE('',*,*,#19429,.T.);
#25656=ORIENTED_EDGE('',*,*,#19448,.T.);
#25657=ORIENTED_EDGE('',*,*,#19434,.T.);
#25658=ORIENTED_EDGE('',*,*,#19449,.T.);
#25659=ORIENTED_EDGE('',*,*,#17891,.T.);
#25660=ORIENTED_EDGE('',*,*,#19450,.T.);
#25661=ORIENTED_EDGE('',*,*,#19433,.T.);
#25662=ORIENTED_EDGE('',*,*,#19451,.T.);
#25663=ORIENTED_EDGE('',*,*,#19431,.T.);
#25664=ORIENTED_EDGE('',*,*,#19452,.T.);
#25665=ORIENTED_EDGE('',*,*,#19430,.T.);
#25666=ORIENTED_EDGE('',*,*,#19453,.T.);
#25667=ORIENTED_EDGE('',*,*,#17889,.T.);
#25668=ORIENTED_EDGE('',*,*,#19454,.T.);
#25669=ORIENTED_EDGE('',*,*,#19428,.T.);
#25670=ORIENTED_EDGE('',*,*,#19455,.T.);
#25671=ORIENTED_EDGE('',*,*,#19443,.F.);
#25672=ORIENTED_EDGE('',*,*,#19447,.F.);
#25673=ORIENTED_EDGE('',*,*,#19437,.F.);
#25674=ORIENTED_EDGE('',*,*,#17886,.F.);
#25675=ORIENTED_EDGE('',*,*,#19438,.F.);
#25676=ORIENTED_EDGE('',*,*,#19448,.F.);
#25677=ORIENTED_EDGE('',*,*,#19454,.F.);
#25678=ORIENTED_EDGE('',*,*,#17888,.F.);
#25679=ORIENTED_EDGE('',*,*,#19444,.F.);
#25680=ORIENTED_EDGE('',*,*,#19453,.F.);
#25681=ORIENTED_EDGE('',*,*,#19449,.F.);
#25682=ORIENTED_EDGE('',*,*,#19446,.F.);
#25683=ORIENTED_EDGE('',*,*,#19456,.F.);
#25684=ORIENTED_EDGE('',*,*,#19457,.F.);
#25685=ORIENTED_EDGE('',*,*,#19458,.F.);
#25686=ORIENTED_EDGE('',*,*,#19459,.T.);
#25687=ORIENTED_EDGE('',*,*,#19460,.T.);
#25688=ORIENTED_EDGE('',*,*,#19457,.T.);
#25689=ORIENTED_EDGE('',*,*,#19461,.T.);
#25690=ORIENTED_EDGE('',*,*,#19462,.T.);
#25691=ORIENTED_EDGE('',*,*,#17899,.T.);
#25692=ORIENTED_EDGE('',*,*,#19463,.T.);
#25693=ORIENTED_EDGE('',*,*,#19458,.T.);
#25694=ORIENTED_EDGE('',*,*,#19464,.T.);
#25695=ORIENTED_EDGE('',*,*,#19465,.F.);
#25696=ORIENTED_EDGE('',*,*,#19466,.F.);
#25697=ORIENTED_EDGE('',*,*,#19467,.F.);
#25698=ORIENTED_EDGE('',*,*,#19468,.T.);
#25699=ORIENTED_EDGE('',*,*,#19469,.T.);
#25700=ORIENTED_EDGE('',*,*,#19466,.T.);
#25701=ORIENTED_EDGE('',*,*,#19470,.T.);
#25702=ORIENTED_EDGE('',*,*,#19471,.T.);
#25703=ORIENTED_EDGE('',*,*,#19456,.T.);
#25704=ORIENTED_EDGE('',*,*,#19472,.T.);
#25705=ORIENTED_EDGE('',*,*,#19467,.T.);
#25706=ORIENTED_EDGE('',*,*,#19473,.T.);
#25707=ORIENTED_EDGE('',*,*,#17897,.T.);
#25708=ORIENTED_EDGE('',*,*,#19474,.T.);
#25709=ORIENTED_EDGE('',*,*,#19465,.T.);
#25710=ORIENTED_EDGE('',*,*,#19475,.T.);
#25711=ORIENTED_EDGE('',*,*,#19459,.F.);
#25712=ORIENTED_EDGE('',*,*,#19476,.T.);
#25713=ORIENTED_EDGE('',*,*,#19477,.T.);
#25714=ORIENTED_EDGE('',*,*,#17893,.T.);
#25715=ORIENTED_EDGE('',*,*,#19478,.T.);
#25716=ORIENTED_EDGE('',*,*,#19461,.F.);
#25717=ORIENTED_EDGE('',*,*,#19473,.F.);
#25718=ORIENTED_EDGE('',*,*,#19469,.F.);
#25719=ORIENTED_EDGE('',*,*,#19479,.F.);
#25720=ORIENTED_EDGE('',*,*,#19462,.F.);
#25721=ORIENTED_EDGE('',*,*,#19479,.T.);
#25722=ORIENTED_EDGE('',*,*,#19468,.F.);
#25723=ORIENTED_EDGE('',*,*,#19480,.F.);
#25724=ORIENTED_EDGE('',*,*,#19481,.T.);
#25725=ORIENTED_EDGE('',*,*,#19476,.F.);
#25726=ORIENTED_EDGE('',*,*,#19471,.F.);
#25727=ORIENTED_EDGE('',*,*,#19482,.T.);
#25728=ORIENTED_EDGE('',*,*,#17895,.T.);
#25729=ORIENTED_EDGE('',*,*,#19483,.T.);
#25730=ORIENTED_EDGE('',*,*,#19480,.T.);
#25731=ORIENTED_EDGE('',*,*,#19470,.F.);
#25732=ORIENTED_EDGE('',*,*,#19474,.F.);
#25733=ORIENTED_EDGE('',*,*,#17896,.F.);
#25734=ORIENTED_EDGE('',*,*,#19482,.F.);
#25735=ORIENTED_EDGE('',*,*,#19460,.F.);
#25736=ORIENTED_EDGE('',*,*,#19478,.F.);
#25737=ORIENTED_EDGE('',*,*,#17892,.F.);
#25738=ORIENTED_EDGE('',*,*,#19464,.F.);
#25739=ORIENTED_EDGE('',*,*,#19484,.F.);
#25740=ORIENTED_EDGE('',*,*,#19485,.F.);
#25741=ORIENTED_EDGE('',*,*,#19486,.F.);
#25742=ORIENTED_EDGE('',*,*,#19487,.F.);
#25743=ORIENTED_EDGE('',*,*,#19488,.F.);
#25744=ORIENTED_EDGE('',*,*,#19489,.F.);
#25745=ORIENTED_EDGE('',*,*,#19490,.F.);
#25746=ORIENTED_EDGE('',*,*,#19491,.F.);
#25747=ORIENTED_EDGE('',*,*,#19492,.F.);
#25748=ORIENTED_EDGE('',*,*,#17903,.T.);
#25749=ORIENTED_EDGE('',*,*,#19493,.T.);
#25750=ORIENTED_EDGE('',*,*,#19491,.T.);
#25751=ORIENTED_EDGE('',*,*,#19494,.T.);
#25752=ORIENTED_EDGE('',*,*,#19495,.F.);
#25753=ORIENTED_EDGE('',*,*,#19496,.F.);
#25754=ORIENTED_EDGE('',*,*,#19497,.F.);
#25755=ORIENTED_EDGE('',*,*,#17901,.T.);
#25756=ORIENTED_EDGE('',*,*,#19498,.T.);
#25757=ORIENTED_EDGE('',*,*,#19496,.T.);
#25758=ORIENTED_EDGE('',*,*,#19499,.T.);
#25759=ORIENTED_EDGE('',*,*,#19488,.T.);
#25760=ORIENTED_EDGE('',*,*,#19500,.T.);
#25761=ORIENTED_EDGE('',*,*,#19497,.T.);
#25762=ORIENTED_EDGE('',*,*,#19501,.T.);
#25763=ORIENTED_EDGE('',*,*,#19495,.T.);
#25764=ORIENTED_EDGE('',*,*,#19502,.T.);
#25765=ORIENTED_EDGE('',*,*,#19492,.T.);
#25766=ORIENTED_EDGE('',*,*,#19503,.T.);
#25767=ORIENTED_EDGE('',*,*,#19485,.T.);
#25768=ORIENTED_EDGE('',*,*,#19504,.T.);
#25769=ORIENTED_EDGE('',*,*,#19490,.T.);
#25770=ORIENTED_EDGE('',*,*,#19505,.T.);
#25771=ORIENTED_EDGE('',*,*,#17907,.T.);
#25772=ORIENTED_EDGE('',*,*,#19506,.T.);
#25773=ORIENTED_EDGE('',*,*,#19489,.T.);
#25774=ORIENTED_EDGE('',*,*,#19507,.T.);
#25775=ORIENTED_EDGE('',*,*,#19487,.T.);
#25776=ORIENTED_EDGE('',*,*,#19508,.T.);
#25777=ORIENTED_EDGE('',*,*,#19486,.T.);
#25778=ORIENTED_EDGE('',*,*,#19509,.T.);
#25779=ORIENTED_EDGE('',*,*,#17905,.T.);
#25780=ORIENTED_EDGE('',*,*,#19510,.T.);
#25781=ORIENTED_EDGE('',*,*,#19484,.T.);
#25782=ORIENTED_EDGE('',*,*,#19511,.T.);
#25783=ORIENTED_EDGE('',*,*,#19499,.F.);
#25784=ORIENTED_EDGE('',*,*,#19503,.F.);
#25785=ORIENTED_EDGE('',*,*,#19493,.F.);
#25786=ORIENTED_EDGE('',*,*,#17902,.F.);
#25787=ORIENTED_EDGE('',*,*,#19494,.F.);
#25788=ORIENTED_EDGE('',*,*,#19504,.F.);
#25789=ORIENTED_EDGE('',*,*,#19510,.F.);
#25790=ORIENTED_EDGE('',*,*,#17904,.F.);
#25791=ORIENTED_EDGE('',*,*,#19500,.F.);
#25792=ORIENTED_EDGE('',*,*,#19509,.F.);
#25793=ORIENTED_EDGE('',*,*,#19505,.F.);
#25794=ORIENTED_EDGE('',*,*,#19502,.F.);
#25795=ORIENTED_EDGE('',*,*,#19512,.F.);
#25796=ORIENTED_EDGE('',*,*,#19513,.F.);
#25797=ORIENTED_EDGE('',*,*,#19514,.F.);
#25798=ORIENTED_EDGE('',*,*,#19515,.F.);
#25799=ORIENTED_EDGE('',*,*,#19516,.F.);
#25800=ORIENTED_EDGE('',*,*,#19517,.F.);
#25801=ORIENTED_EDGE('',*,*,#19518,.F.);
#25802=ORIENTED_EDGE('',*,*,#19519,.F.);
#25803=ORIENTED_EDGE('',*,*,#19520,.F.);
#25804=ORIENTED_EDGE('',*,*,#17911,.T.);
#25805=ORIENTED_EDGE('',*,*,#19521,.T.);
#25806=ORIENTED_EDGE('',*,*,#19519,.T.);
#25807=ORIENTED_EDGE('',*,*,#19522,.T.);
#25808=ORIENTED_EDGE('',*,*,#19523,.F.);
#25809=ORIENTED_EDGE('',*,*,#19524,.F.);
#25810=ORIENTED_EDGE('',*,*,#19525,.F.);
#25811=ORIENTED_EDGE('',*,*,#17909,.T.);
#25812=ORIENTED_EDGE('',*,*,#19526,.T.);
#25813=ORIENTED_EDGE('',*,*,#19524,.T.);
#25814=ORIENTED_EDGE('',*,*,#19527,.T.);
#25815=ORIENTED_EDGE('',*,*,#19516,.T.);
#25816=ORIENTED_EDGE('',*,*,#19528,.T.);
#25817=ORIENTED_EDGE('',*,*,#19525,.T.);
#25818=ORIENTED_EDGE('',*,*,#19529,.T.);
#25819=ORIENTED_EDGE('',*,*,#19523,.T.);
#25820=ORIENTED_EDGE('',*,*,#19530,.T.);
#25821=ORIENTED_EDGE('',*,*,#19520,.T.);
#25822=ORIENTED_EDGE('',*,*,#19531,.T.);
#25823=ORIENTED_EDGE('',*,*,#19513,.T.);
#25824=ORIENTED_EDGE('',*,*,#19532,.T.);
#25825=ORIENTED_EDGE('',*,*,#19518,.T.);
#25826=ORIENTED_EDGE('',*,*,#19533,.T.);
#25827=ORIENTED_EDGE('',*,*,#17915,.T.);
#25828=ORIENTED_EDGE('',*,*,#19534,.T.);
#25829=ORIENTED_EDGE('',*,*,#19517,.T.);
#25830=ORIENTED_EDGE('',*,*,#19535,.T.);
#25831=ORIENTED_EDGE('',*,*,#19515,.T.);
#25832=ORIENTED_EDGE('',*,*,#19536,.T.);
#25833=ORIENTED_EDGE('',*,*,#19514,.T.);
#25834=ORIENTED_EDGE('',*,*,#19537,.T.);
#25835=ORIENTED_EDGE('',*,*,#17913,.T.);
#25836=ORIENTED_EDGE('',*,*,#19538,.T.);
#25837=ORIENTED_EDGE('',*,*,#19512,.T.);
#25838=ORIENTED_EDGE('',*,*,#19539,.T.);
#25839=ORIENTED_EDGE('',*,*,#19527,.F.);
#25840=ORIENTED_EDGE('',*,*,#19531,.F.);
#25841=ORIENTED_EDGE('',*,*,#19521,.F.);
#25842=ORIENTED_EDGE('',*,*,#17910,.F.);
#25843=ORIENTED_EDGE('',*,*,#19522,.F.);
#25844=ORIENTED_EDGE('',*,*,#19532,.F.);
#25845=ORIENTED_EDGE('',*,*,#19538,.F.);
#25846=ORIENTED_EDGE('',*,*,#17912,.F.);
#25847=ORIENTED_EDGE('',*,*,#19528,.F.);
#25848=ORIENTED_EDGE('',*,*,#19537,.F.);
#25849=ORIENTED_EDGE('',*,*,#19533,.F.);
#25850=ORIENTED_EDGE('',*,*,#19530,.F.);
#25851=ORIENTED_EDGE('',*,*,#19540,.T.);
#25852=ORIENTED_EDGE('',*,*,#19541,.T.);
#25853=ORIENTED_EDGE('',*,*,#17921,.T.);
#25854=ORIENTED_EDGE('',*,*,#19542,.T.);
#25855=ORIENTED_EDGE('',*,*,#19543,.T.);
#25856=ORIENTED_EDGE('',*,*,#19541,.F.);
#25857=ORIENTED_EDGE('',*,*,#19544,.F.);
#25858=ORIENTED_EDGE('',*,*,#19545,.F.);
#25859=ORIENTED_EDGE('',*,*,#17922,.F.);
#25860=ORIENTED_EDGE('',*,*,#19540,.F.);
#25861=ORIENTED_EDGE('',*,*,#19546,.F.);
#25862=ORIENTED_EDGE('',*,*,#19547,.T.);
#25863=ORIENTED_EDGE('',*,*,#19548,.T.);
#25864=ORIENTED_EDGE('',*,*,#19544,.T.);
#25865=ORIENTED_EDGE('',*,*,#19543,.F.);
#25866=ORIENTED_EDGE('',*,*,#19549,.T.);
#25867=ORIENTED_EDGE('',*,*,#19550,.T.);
#25868=ORIENTED_EDGE('',*,*,#19551,.T.);
#25869=ORIENTED_EDGE('',*,*,#19546,.T.);
#25870=ORIENTED_EDGE('',*,*,#19548,.F.);
#25871=ORIENTED_EDGE('',*,*,#19552,.F.);
#25872=ORIENTED_EDGE('',*,*,#19553,.F.);
#25873=ORIENTED_EDGE('',*,*,#19550,.F.);
#25874=ORIENTED_EDGE('',*,*,#19554,.F.);
#25875=ORIENTED_EDGE('',*,*,#19555,.F.);
#25876=ORIENTED_EDGE('',*,*,#17919,.T.);
#25877=ORIENTED_EDGE('',*,*,#19556,.T.);
#25878=ORIENTED_EDGE('',*,*,#19554,.T.);
#25879=ORIENTED_EDGE('',*,*,#19557,.T.);
#25880=ORIENTED_EDGE('',*,*,#19558,.F.);
#25881=ORIENTED_EDGE('',*,*,#19559,.F.);
#25882=ORIENTED_EDGE('',*,*,#19560,.F.);
#25883=ORIENTED_EDGE('',*,*,#17917,.T.);
#25884=ORIENTED_EDGE('',*,*,#19561,.T.);
#25885=ORIENTED_EDGE('',*,*,#19559,.T.);
#25886=ORIENTED_EDGE('',*,*,#19562,.T.);
#25887=ORIENTED_EDGE('',*,*,#19552,.T.);
#25888=ORIENTED_EDGE('',*,*,#19563,.T.);
#25889=ORIENTED_EDGE('',*,*,#19560,.T.);
#25890=ORIENTED_EDGE('',*,*,#19564,.T.);
#25891=ORIENTED_EDGE('',*,*,#19558,.T.);
#25892=ORIENTED_EDGE('',*,*,#19565,.T.);
#25893=ORIENTED_EDGE('',*,*,#19555,.T.);
#25894=ORIENTED_EDGE('',*,*,#19566,.T.);
#25895=ORIENTED_EDGE('',*,*,#17923,.T.);
#25896=ORIENTED_EDGE('',*,*,#19545,.T.);
#25897=ORIENTED_EDGE('',*,*,#19553,.T.);
#25898=ORIENTED_EDGE('',*,*,#19567,.T.);
#25899=ORIENTED_EDGE('',*,*,#19542,.F.);
#25900=ORIENTED_EDGE('',*,*,#17920,.F.);
#25901=ORIENTED_EDGE('',*,*,#19557,.F.);
#25902=ORIENTED_EDGE('',*,*,#19549,.F.);
#25903=ORIENTED_EDGE('',*,*,#19563,.F.);
#25904=ORIENTED_EDGE('',*,*,#19547,.F.);
#25905=ORIENTED_EDGE('',*,*,#19551,.F.);
#25906=ORIENTED_EDGE('',*,*,#19565,.F.);
#25907=ORIENTED_EDGE('',*,*,#19568,.F.);
#25908=ORIENTED_EDGE('',*,*,#19569,.F.);
#25909=ORIENTED_EDGE('',*,*,#19570,.F.);
#25910=ORIENTED_EDGE('',*,*,#19571,.F.);
#25911=ORIENTED_EDGE('',*,*,#19572,.F.);
#25912=ORIENTED_EDGE('',*,*,#19573,.F.);
#25913=ORIENTED_EDGE('',*,*,#19574,.F.);
#25914=ORIENTED_EDGE('',*,*,#19575,.F.);
#25915=ORIENTED_EDGE('',*,*,#19576,.F.);
#25916=ORIENTED_EDGE('',*,*,#17927,.T.);
#25917=ORIENTED_EDGE('',*,*,#19577,.T.);
#25918=ORIENTED_EDGE('',*,*,#19575,.T.);
#25919=ORIENTED_EDGE('',*,*,#19578,.T.);
#25920=ORIENTED_EDGE('',*,*,#19579,.F.);
#25921=ORIENTED_EDGE('',*,*,#19580,.F.);
#25922=ORIENTED_EDGE('',*,*,#19581,.F.);
#25923=ORIENTED_EDGE('',*,*,#17925,.T.);
#25924=ORIENTED_EDGE('',*,*,#19582,.T.);
#25925=ORIENTED_EDGE('',*,*,#19580,.T.);
#25926=ORIENTED_EDGE('',*,*,#19583,.T.);
#25927=ORIENTED_EDGE('',*,*,#19572,.T.);
#25928=ORIENTED_EDGE('',*,*,#19584,.T.);
#25929=ORIENTED_EDGE('',*,*,#19581,.T.);
#25930=ORIENTED_EDGE('',*,*,#19585,.T.);
#25931=ORIENTED_EDGE('',*,*,#19579,.T.);
#25932=ORIENTED_EDGE('',*,*,#19586,.T.);
#25933=ORIENTED_EDGE('',*,*,#19576,.T.);
#25934=ORIENTED_EDGE('',*,*,#19587,.T.);
#25935=ORIENTED_EDGE('',*,*,#19569,.T.);
#25936=ORIENTED_EDGE('',*,*,#19588,.T.);
#25937=ORIENTED_EDGE('',*,*,#19574,.T.);
#25938=ORIENTED_EDGE('',*,*,#19589,.T.);
#25939=ORIENTED_EDGE('',*,*,#17931,.T.);
#25940=ORIENTED_EDGE('',*,*,#19590,.T.);
#25941=ORIENTED_EDGE('',*,*,#19573,.T.);
#25942=ORIENTED_EDGE('',*,*,#19591,.T.);
#25943=ORIENTED_EDGE('',*,*,#19571,.T.);
#25944=ORIENTED_EDGE('',*,*,#19592,.T.);
#25945=ORIENTED_EDGE('',*,*,#19570,.T.);
#25946=ORIENTED_EDGE('',*,*,#19593,.T.);
#25947=ORIENTED_EDGE('',*,*,#17929,.T.);
#25948=ORIENTED_EDGE('',*,*,#19594,.T.);
#25949=ORIENTED_EDGE('',*,*,#19568,.T.);
#25950=ORIENTED_EDGE('',*,*,#19595,.T.);
#25951=ORIENTED_EDGE('',*,*,#19583,.F.);
#25952=ORIENTED_EDGE('',*,*,#19587,.F.);
#25953=ORIENTED_EDGE('',*,*,#19577,.F.);
#25954=ORIENTED_EDGE('',*,*,#17926,.F.);
#25955=ORIENTED_EDGE('',*,*,#19578,.F.);
#25956=ORIENTED_EDGE('',*,*,#19588,.F.);
#25957=ORIENTED_EDGE('',*,*,#19594,.F.);
#25958=ORIENTED_EDGE('',*,*,#17928,.F.);
#25959=ORIENTED_EDGE('',*,*,#19584,.F.);
#25960=ORIENTED_EDGE('',*,*,#19593,.F.);
#25961=ORIENTED_EDGE('',*,*,#19589,.F.);
#25962=ORIENTED_EDGE('',*,*,#19586,.F.);
#25963=ORIENTED_EDGE('',*,*,#19596,.F.);
#25964=ORIENTED_EDGE('',*,*,#19597,.F.);
#25965=ORIENTED_EDGE('',*,*,#19598,.F.);
#25966=ORIENTED_EDGE('',*,*,#19599,.T.);
#25967=ORIENTED_EDGE('',*,*,#19600,.T.);
#25968=ORIENTED_EDGE('',*,*,#19597,.T.);
#25969=ORIENTED_EDGE('',*,*,#19601,.T.);
#25970=ORIENTED_EDGE('',*,*,#19602,.T.);
#25971=ORIENTED_EDGE('',*,*,#17939,.T.);
#25972=ORIENTED_EDGE('',*,*,#19603,.T.);
#25973=ORIENTED_EDGE('',*,*,#19598,.T.);
#25974=ORIENTED_EDGE('',*,*,#19604,.T.);
#25975=ORIENTED_EDGE('',*,*,#19605,.F.);
#25976=ORIENTED_EDGE('',*,*,#19606,.F.);
#25977=ORIENTED_EDGE('',*,*,#19607,.F.);
#25978=ORIENTED_EDGE('',*,*,#19608,.T.);
#25979=ORIENTED_EDGE('',*,*,#19609,.T.);
#25980=ORIENTED_EDGE('',*,*,#19606,.T.);
#25981=ORIENTED_EDGE('',*,*,#19610,.T.);
#25982=ORIENTED_EDGE('',*,*,#19611,.T.);
#25983=ORIENTED_EDGE('',*,*,#19596,.T.);
#25984=ORIENTED_EDGE('',*,*,#19612,.T.);
#25985=ORIENTED_EDGE('',*,*,#19607,.T.);
#25986=ORIENTED_EDGE('',*,*,#19613,.T.);
#25987=ORIENTED_EDGE('',*,*,#17937,.T.);
#25988=ORIENTED_EDGE('',*,*,#19614,.T.);
#25989=ORIENTED_EDGE('',*,*,#19605,.T.);
#25990=ORIENTED_EDGE('',*,*,#19615,.T.);
#25991=ORIENTED_EDGE('',*,*,#19599,.F.);
#25992=ORIENTED_EDGE('',*,*,#19616,.T.);
#25993=ORIENTED_EDGE('',*,*,#19617,.T.);
#25994=ORIENTED_EDGE('',*,*,#17933,.T.);
#25995=ORIENTED_EDGE('',*,*,#19618,.T.);
#25996=ORIENTED_EDGE('',*,*,#19601,.F.);
#25997=ORIENTED_EDGE('',*,*,#19613,.F.);
#25998=ORIENTED_EDGE('',*,*,#19609,.F.);
#25999=ORIENTED_EDGE('',*,*,#19619,.F.);
#26000=ORIENTED_EDGE('',*,*,#19602,.F.);
#26001=ORIENTED_EDGE('',*,*,#19619,.T.);
#26002=ORIENTED_EDGE('',*,*,#19608,.F.);
#26003=ORIENTED_EDGE('',*,*,#19620,.F.);
#26004=ORIENTED_EDGE('',*,*,#19621,.T.);
#26005=ORIENTED_EDGE('',*,*,#19616,.F.);
#26006=ORIENTED_EDGE('',*,*,#19611,.F.);
#26007=ORIENTED_EDGE('',*,*,#19622,.T.);
#26008=ORIENTED_EDGE('',*,*,#17935,.T.);
#26009=ORIENTED_EDGE('',*,*,#19623,.T.);
#26010=ORIENTED_EDGE('',*,*,#19620,.T.);
#26011=ORIENTED_EDGE('',*,*,#19610,.F.);
#26012=ORIENTED_EDGE('',*,*,#19614,.F.);
#26013=ORIENTED_EDGE('',*,*,#17936,.F.);
#26014=ORIENTED_EDGE('',*,*,#19622,.F.);
#26015=ORIENTED_EDGE('',*,*,#19600,.F.);
#26016=ORIENTED_EDGE('',*,*,#19618,.F.);
#26017=ORIENTED_EDGE('',*,*,#17932,.F.);
#26018=ORIENTED_EDGE('',*,*,#19604,.F.);
#26019=ORIENTED_EDGE('',*,*,#19624,.F.);
#26020=ORIENTED_EDGE('',*,*,#19625,.F.);
#26021=ORIENTED_EDGE('',*,*,#19626,.F.);
#26022=ORIENTED_EDGE('',*,*,#19627,.F.);
#26023=ORIENTED_EDGE('',*,*,#19628,.F.);
#26024=ORIENTED_EDGE('',*,*,#19629,.F.);
#26025=ORIENTED_EDGE('',*,*,#19630,.F.);
#26026=ORIENTED_EDGE('',*,*,#19631,.F.);
#26027=ORIENTED_EDGE('',*,*,#19632,.F.);
#26028=ORIENTED_EDGE('',*,*,#17943,.T.);
#26029=ORIENTED_EDGE('',*,*,#19633,.T.);
#26030=ORIENTED_EDGE('',*,*,#19631,.T.);
#26031=ORIENTED_EDGE('',*,*,#19634,.T.);
#26032=ORIENTED_EDGE('',*,*,#19635,.F.);
#26033=ORIENTED_EDGE('',*,*,#19636,.F.);
#26034=ORIENTED_EDGE('',*,*,#19637,.F.);
#26035=ORIENTED_EDGE('',*,*,#17941,.T.);
#26036=ORIENTED_EDGE('',*,*,#19638,.T.);
#26037=ORIENTED_EDGE('',*,*,#19636,.T.);
#26038=ORIENTED_EDGE('',*,*,#19639,.T.);
#26039=ORIENTED_EDGE('',*,*,#19628,.T.);
#26040=ORIENTED_EDGE('',*,*,#19640,.T.);
#26041=ORIENTED_EDGE('',*,*,#19637,.T.);
#26042=ORIENTED_EDGE('',*,*,#19641,.T.);
#26043=ORIENTED_EDGE('',*,*,#19635,.T.);
#26044=ORIENTED_EDGE('',*,*,#19642,.T.);
#26045=ORIENTED_EDGE('',*,*,#19632,.T.);
#26046=ORIENTED_EDGE('',*,*,#19643,.T.);
#26047=ORIENTED_EDGE('',*,*,#19625,.T.);
#26048=ORIENTED_EDGE('',*,*,#19644,.T.);
#26049=ORIENTED_EDGE('',*,*,#19630,.T.);
#26050=ORIENTED_EDGE('',*,*,#19645,.T.);
#26051=ORIENTED_EDGE('',*,*,#17947,.T.);
#26052=ORIENTED_EDGE('',*,*,#19646,.T.);
#26053=ORIENTED_EDGE('',*,*,#19629,.T.);
#26054=ORIENTED_EDGE('',*,*,#19647,.T.);
#26055=ORIENTED_EDGE('',*,*,#19627,.T.);
#26056=ORIENTED_EDGE('',*,*,#19648,.T.);
#26057=ORIENTED_EDGE('',*,*,#19626,.T.);
#26058=ORIENTED_EDGE('',*,*,#19649,.T.);
#26059=ORIENTED_EDGE('',*,*,#17945,.T.);
#26060=ORIENTED_EDGE('',*,*,#19650,.T.);
#26061=ORIENTED_EDGE('',*,*,#19624,.T.);
#26062=ORIENTED_EDGE('',*,*,#19651,.T.);
#26063=ORIENTED_EDGE('',*,*,#19639,.F.);
#26064=ORIENTED_EDGE('',*,*,#19643,.F.);
#26065=ORIENTED_EDGE('',*,*,#19633,.F.);
#26066=ORIENTED_EDGE('',*,*,#17942,.F.);
#26067=ORIENTED_EDGE('',*,*,#19634,.F.);
#26068=ORIENTED_EDGE('',*,*,#19644,.F.);
#26069=ORIENTED_EDGE('',*,*,#19650,.F.);
#26070=ORIENTED_EDGE('',*,*,#17944,.F.);
#26071=ORIENTED_EDGE('',*,*,#19640,.F.);
#26072=ORIENTED_EDGE('',*,*,#19649,.F.);
#26073=ORIENTED_EDGE('',*,*,#19645,.F.);
#26074=ORIENTED_EDGE('',*,*,#19642,.F.);
#26075=ORIENTED_EDGE('',*,*,#19652,.F.);
#26076=ORIENTED_EDGE('',*,*,#19653,.F.);
#26077=ORIENTED_EDGE('',*,*,#19654,.F.);
#26078=ORIENTED_EDGE('',*,*,#19655,.F.);
#26079=ORIENTED_EDGE('',*,*,#19656,.F.);
#26080=ORIENTED_EDGE('',*,*,#19657,.F.);
#26081=ORIENTED_EDGE('',*,*,#19658,.F.);
#26082=ORIENTED_EDGE('',*,*,#19659,.F.);
#26083=ORIENTED_EDGE('',*,*,#19660,.F.);
#26084=ORIENTED_EDGE('',*,*,#17951,.T.);
#26085=ORIENTED_EDGE('',*,*,#19661,.T.);
#26086=ORIENTED_EDGE('',*,*,#19659,.T.);
#26087=ORIENTED_EDGE('',*,*,#19662,.T.);
#26088=ORIENTED_EDGE('',*,*,#19663,.F.);
#26089=ORIENTED_EDGE('',*,*,#19664,.F.);
#26090=ORIENTED_EDGE('',*,*,#19665,.F.);
#26091=ORIENTED_EDGE('',*,*,#17949,.T.);
#26092=ORIENTED_EDGE('',*,*,#19666,.T.);
#26093=ORIENTED_EDGE('',*,*,#19664,.T.);
#26094=ORIENTED_EDGE('',*,*,#19667,.T.);
#26095=ORIENTED_EDGE('',*,*,#19656,.T.);
#26096=ORIENTED_EDGE('',*,*,#19668,.T.);
#26097=ORIENTED_EDGE('',*,*,#19665,.T.);
#26098=ORIENTED_EDGE('',*,*,#19669,.T.);
#26099=ORIENTED_EDGE('',*,*,#19663,.T.);
#26100=ORIENTED_EDGE('',*,*,#19670,.T.);
#26101=ORIENTED_EDGE('',*,*,#19660,.T.);
#26102=ORIENTED_EDGE('',*,*,#19671,.T.);
#26103=ORIENTED_EDGE('',*,*,#19653,.T.);
#26104=ORIENTED_EDGE('',*,*,#19672,.T.);
#26105=ORIENTED_EDGE('',*,*,#19658,.T.);
#26106=ORIENTED_EDGE('',*,*,#19673,.T.);
#26107=ORIENTED_EDGE('',*,*,#17955,.T.);
#26108=ORIENTED_EDGE('',*,*,#19674,.T.);
#26109=ORIENTED_EDGE('',*,*,#19657,.T.);
#26110=ORIENTED_EDGE('',*,*,#19675,.T.);
#26111=ORIENTED_EDGE('',*,*,#19655,.T.);
#26112=ORIENTED_EDGE('',*,*,#19676,.T.);
#26113=ORIENTED_EDGE('',*,*,#19654,.T.);
#26114=ORIENTED_EDGE('',*,*,#19677,.T.);
#26115=ORIENTED_EDGE('',*,*,#17953,.T.);
#26116=ORIENTED_EDGE('',*,*,#19678,.T.);
#26117=ORIENTED_EDGE('',*,*,#19652,.T.);
#26118=ORIENTED_EDGE('',*,*,#19679,.T.);
#26119=ORIENTED_EDGE('',*,*,#19667,.F.);
#26120=ORIENTED_EDGE('',*,*,#19671,.F.);
#26121=ORIENTED_EDGE('',*,*,#19661,.F.);
#26122=ORIENTED_EDGE('',*,*,#17950,.F.);
#26123=ORIENTED_EDGE('',*,*,#19662,.F.);
#26124=ORIENTED_EDGE('',*,*,#19672,.F.);
#26125=ORIENTED_EDGE('',*,*,#19678,.F.);
#26126=ORIENTED_EDGE('',*,*,#17952,.F.);
#26127=ORIENTED_EDGE('',*,*,#19668,.F.);
#26128=ORIENTED_EDGE('',*,*,#19677,.F.);
#26129=ORIENTED_EDGE('',*,*,#19673,.F.);
#26130=ORIENTED_EDGE('',*,*,#19670,.F.);
#26131=ORIENTED_EDGE('',*,*,#19680,.T.);
#26132=ORIENTED_EDGE('',*,*,#19681,.T.);
#26133=ORIENTED_EDGE('',*,*,#17961,.T.);
#26134=ORIENTED_EDGE('',*,*,#19682,.T.);
#26135=ORIENTED_EDGE('',*,*,#19683,.T.);
#26136=ORIENTED_EDGE('',*,*,#19681,.F.);
#26137=ORIENTED_EDGE('',*,*,#19684,.F.);
#26138=ORIENTED_EDGE('',*,*,#19685,.F.);
#26139=ORIENTED_EDGE('',*,*,#17962,.F.);
#26140=ORIENTED_EDGE('',*,*,#19680,.F.);
#26141=ORIENTED_EDGE('',*,*,#19686,.F.);
#26142=ORIENTED_EDGE('',*,*,#19687,.T.);
#26143=ORIENTED_EDGE('',*,*,#19688,.T.);
#26144=ORIENTED_EDGE('',*,*,#19684,.T.);
#26145=ORIENTED_EDGE('',*,*,#19683,.F.);
#26146=ORIENTED_EDGE('',*,*,#19689,.T.);
#26147=ORIENTED_EDGE('',*,*,#19690,.T.);
#26148=ORIENTED_EDGE('',*,*,#19691,.T.);
#26149=ORIENTED_EDGE('',*,*,#19686,.T.);
#26150=ORIENTED_EDGE('',*,*,#19688,.F.);
#26151=ORIENTED_EDGE('',*,*,#19692,.F.);
#26152=ORIENTED_EDGE('',*,*,#19693,.F.);
#26153=ORIENTED_EDGE('',*,*,#19690,.F.);
#26154=ORIENTED_EDGE('',*,*,#19694,.F.);
#26155=ORIENTED_EDGE('',*,*,#19695,.F.);
#26156=ORIENTED_EDGE('',*,*,#17959,.T.);
#26157=ORIENTED_EDGE('',*,*,#19696,.T.);
#26158=ORIENTED_EDGE('',*,*,#19694,.T.);
#26159=ORIENTED_EDGE('',*,*,#19697,.T.);
#26160=ORIENTED_EDGE('',*,*,#19698,.F.);
#26161=ORIENTED_EDGE('',*,*,#19699,.F.);
#26162=ORIENTED_EDGE('',*,*,#19700,.F.);
#26163=ORIENTED_EDGE('',*,*,#17957,.T.);
#26164=ORIENTED_EDGE('',*,*,#19701,.T.);
#26165=ORIENTED_EDGE('',*,*,#19699,.T.);
#26166=ORIENTED_EDGE('',*,*,#19702,.T.);
#26167=ORIENTED_EDGE('',*,*,#19692,.T.);
#26168=ORIENTED_EDGE('',*,*,#19703,.T.);
#26169=ORIENTED_EDGE('',*,*,#19700,.T.);
#26170=ORIENTED_EDGE('',*,*,#19704,.T.);
#26171=ORIENTED_EDGE('',*,*,#19698,.T.);
#26172=ORIENTED_EDGE('',*,*,#19705,.T.);
#26173=ORIENTED_EDGE('',*,*,#19695,.T.);
#26174=ORIENTED_EDGE('',*,*,#19706,.T.);
#26175=ORIENTED_EDGE('',*,*,#17963,.T.);
#26176=ORIENTED_EDGE('',*,*,#19685,.T.);
#26177=ORIENTED_EDGE('',*,*,#19693,.T.);
#26178=ORIENTED_EDGE('',*,*,#19707,.T.);
#26179=ORIENTED_EDGE('',*,*,#19682,.F.);
#26180=ORIENTED_EDGE('',*,*,#17960,.F.);
#26181=ORIENTED_EDGE('',*,*,#19697,.F.);
#26182=ORIENTED_EDGE('',*,*,#19689,.F.);
#26183=ORIENTED_EDGE('',*,*,#19703,.F.);
#26184=ORIENTED_EDGE('',*,*,#19687,.F.);
#26185=ORIENTED_EDGE('',*,*,#19691,.F.);
#26186=ORIENTED_EDGE('',*,*,#19705,.F.);
#26187=ORIENTED_EDGE('',*,*,#19708,.F.);
#26188=ORIENTED_EDGE('',*,*,#19709,.F.);
#26189=ORIENTED_EDGE('',*,*,#19710,.F.);
#26190=ORIENTED_EDGE('',*,*,#19711,.F.);
#26191=ORIENTED_EDGE('',*,*,#19712,.F.);
#26192=ORIENTED_EDGE('',*,*,#19713,.F.);
#26193=ORIENTED_EDGE('',*,*,#19714,.F.);
#26194=ORIENTED_EDGE('',*,*,#19715,.F.);
#26195=ORIENTED_EDGE('',*,*,#19716,.F.);
#26196=ORIENTED_EDGE('',*,*,#17967,.T.);
#26197=ORIENTED_EDGE('',*,*,#19717,.T.);
#26198=ORIENTED_EDGE('',*,*,#19715,.T.);
#26199=ORIENTED_EDGE('',*,*,#19718,.T.);
#26200=ORIENTED_EDGE('',*,*,#19719,.F.);
#26201=ORIENTED_EDGE('',*,*,#19720,.F.);
#26202=ORIENTED_EDGE('',*,*,#19721,.F.);
#26203=ORIENTED_EDGE('',*,*,#17965,.T.);
#26204=ORIENTED_EDGE('',*,*,#19722,.T.);
#26205=ORIENTED_EDGE('',*,*,#19720,.T.);
#26206=ORIENTED_EDGE('',*,*,#19723,.T.);
#26207=ORIENTED_EDGE('',*,*,#19712,.T.);
#26208=ORIENTED_EDGE('',*,*,#19724,.T.);
#26209=ORIENTED_EDGE('',*,*,#19721,.T.);
#26210=ORIENTED_EDGE('',*,*,#19725,.T.);
#26211=ORIENTED_EDGE('',*,*,#19719,.T.);
#26212=ORIENTED_EDGE('',*,*,#19726,.T.);
#26213=ORIENTED_EDGE('',*,*,#19716,.T.);
#26214=ORIENTED_EDGE('',*,*,#19727,.T.);
#26215=ORIENTED_EDGE('',*,*,#19709,.T.);
#26216=ORIENTED_EDGE('',*,*,#19728,.T.);
#26217=ORIENTED_EDGE('',*,*,#19714,.T.);
#26218=ORIENTED_EDGE('',*,*,#19729,.T.);
#26219=ORIENTED_EDGE('',*,*,#17971,.T.);
#26220=ORIENTED_EDGE('',*,*,#19730,.T.);
#26221=ORIENTED_EDGE('',*,*,#19713,.T.);
#26222=ORIENTED_EDGE('',*,*,#19731,.T.);
#26223=ORIENTED_EDGE('',*,*,#19711,.T.);
#26224=ORIENTED_EDGE('',*,*,#19732,.T.);
#26225=ORIENTED_EDGE('',*,*,#19710,.T.);
#26226=ORIENTED_EDGE('',*,*,#19733,.T.);
#26227=ORIENTED_EDGE('',*,*,#17969,.T.);
#26228=ORIENTED_EDGE('',*,*,#19734,.T.);
#26229=ORIENTED_EDGE('',*,*,#19708,.T.);
#26230=ORIENTED_EDGE('',*,*,#19735,.T.);
#26231=ORIENTED_EDGE('',*,*,#19723,.F.);
#26232=ORIENTED_EDGE('',*,*,#19727,.F.);
#26233=ORIENTED_EDGE('',*,*,#19717,.F.);
#26234=ORIENTED_EDGE('',*,*,#17966,.F.);
#26235=ORIENTED_EDGE('',*,*,#19718,.F.);
#26236=ORIENTED_EDGE('',*,*,#19728,.F.);
#26237=ORIENTED_EDGE('',*,*,#19734,.F.);
#26238=ORIENTED_EDGE('',*,*,#17968,.F.);
#26239=ORIENTED_EDGE('',*,*,#19724,.F.);
#26240=ORIENTED_EDGE('',*,*,#19733,.F.);
#26241=ORIENTED_EDGE('',*,*,#19729,.F.);
#26242=ORIENTED_EDGE('',*,*,#19726,.F.);
#26243=ORIENTED_EDGE('',*,*,#19736,.F.);
#26244=ORIENTED_EDGE('',*,*,#19737,.F.);
#26245=ORIENTED_EDGE('',*,*,#19738,.F.);
#26246=ORIENTED_EDGE('',*,*,#19739,.T.);
#26247=ORIENTED_EDGE('',*,*,#19740,.T.);
#26248=ORIENTED_EDGE('',*,*,#19737,.T.);
#26249=ORIENTED_EDGE('',*,*,#19741,.T.);
#26250=ORIENTED_EDGE('',*,*,#19742,.T.);
#26251=ORIENTED_EDGE('',*,*,#17979,.T.);
#26252=ORIENTED_EDGE('',*,*,#19743,.T.);
#26253=ORIENTED_EDGE('',*,*,#19738,.T.);
#26254=ORIENTED_EDGE('',*,*,#19744,.T.);
#26255=ORIENTED_EDGE('',*,*,#19745,.F.);
#26256=ORIENTED_EDGE('',*,*,#19746,.F.);
#26257=ORIENTED_EDGE('',*,*,#19747,.F.);
#26258=ORIENTED_EDGE('',*,*,#19748,.T.);
#26259=ORIENTED_EDGE('',*,*,#19749,.T.);
#26260=ORIENTED_EDGE('',*,*,#19746,.T.);
#26261=ORIENTED_EDGE('',*,*,#19750,.T.);
#26262=ORIENTED_EDGE('',*,*,#19751,.T.);
#26263=ORIENTED_EDGE('',*,*,#19736,.T.);
#26264=ORIENTED_EDGE('',*,*,#19752,.T.);
#26265=ORIENTED_EDGE('',*,*,#19747,.T.);
#26266=ORIENTED_EDGE('',*,*,#19753,.T.);
#26267=ORIENTED_EDGE('',*,*,#17977,.T.);
#26268=ORIENTED_EDGE('',*,*,#19754,.T.);
#26269=ORIENTED_EDGE('',*,*,#19745,.T.);
#26270=ORIENTED_EDGE('',*,*,#19755,.T.);
#26271=ORIENTED_EDGE('',*,*,#19739,.F.);
#26272=ORIENTED_EDGE('',*,*,#19756,.T.);
#26273=ORIENTED_EDGE('',*,*,#19757,.T.);
#26274=ORIENTED_EDGE('',*,*,#17973,.T.);
#26275=ORIENTED_EDGE('',*,*,#19758,.T.);
#26276=ORIENTED_EDGE('',*,*,#19741,.F.);
#26277=ORIENTED_EDGE('',*,*,#19753,.F.);
#26278=ORIENTED_EDGE('',*,*,#19749,.F.);
#26279=ORIENTED_EDGE('',*,*,#19759,.F.);
#26280=ORIENTED_EDGE('',*,*,#19742,.F.);
#26281=ORIENTED_EDGE('',*,*,#19759,.T.);
#26282=ORIENTED_EDGE('',*,*,#19748,.F.);
#26283=ORIENTED_EDGE('',*,*,#19760,.F.);
#26284=ORIENTED_EDGE('',*,*,#19761,.T.);
#26285=ORIENTED_EDGE('',*,*,#19756,.F.);
#26286=ORIENTED_EDGE('',*,*,#19751,.F.);
#26287=ORIENTED_EDGE('',*,*,#19762,.T.);
#26288=ORIENTED_EDGE('',*,*,#17975,.T.);
#26289=ORIENTED_EDGE('',*,*,#19763,.T.);
#26290=ORIENTED_EDGE('',*,*,#19760,.T.);
#26291=ORIENTED_EDGE('',*,*,#19750,.F.);
#26292=ORIENTED_EDGE('',*,*,#19754,.F.);
#26293=ORIENTED_EDGE('',*,*,#17976,.F.);
#26294=ORIENTED_EDGE('',*,*,#19762,.F.);
#26295=ORIENTED_EDGE('',*,*,#19740,.F.);
#26296=ORIENTED_EDGE('',*,*,#19758,.F.);
#26297=ORIENTED_EDGE('',*,*,#17972,.F.);
#26298=ORIENTED_EDGE('',*,*,#19744,.F.);
#26299=ORIENTED_EDGE('',*,*,#19764,.F.);
#26300=ORIENTED_EDGE('',*,*,#19765,.F.);
#26301=ORIENTED_EDGE('',*,*,#19766,.F.);
#26302=ORIENTED_EDGE('',*,*,#19767,.F.);
#26303=ORIENTED_EDGE('',*,*,#19768,.F.);
#26304=ORIENTED_EDGE('',*,*,#19769,.F.);
#26305=ORIENTED_EDGE('',*,*,#19770,.F.);
#26306=ORIENTED_EDGE('',*,*,#19771,.F.);
#26307=ORIENTED_EDGE('',*,*,#19772,.F.);
#26308=ORIENTED_EDGE('',*,*,#17983,.T.);
#26309=ORIENTED_EDGE('',*,*,#19773,.T.);
#26310=ORIENTED_EDGE('',*,*,#19771,.T.);
#26311=ORIENTED_EDGE('',*,*,#19774,.T.);
#26312=ORIENTED_EDGE('',*,*,#19775,.F.);
#26313=ORIENTED_EDGE('',*,*,#19776,.F.);
#26314=ORIENTED_EDGE('',*,*,#19777,.F.);
#26315=ORIENTED_EDGE('',*,*,#17981,.T.);
#26316=ORIENTED_EDGE('',*,*,#19778,.T.);
#26317=ORIENTED_EDGE('',*,*,#19776,.T.);
#26318=ORIENTED_EDGE('',*,*,#19779,.T.);
#26319=ORIENTED_EDGE('',*,*,#19768,.T.);
#26320=ORIENTED_EDGE('',*,*,#19780,.T.);
#26321=ORIENTED_EDGE('',*,*,#19777,.T.);
#26322=ORIENTED_EDGE('',*,*,#19781,.T.);
#26323=ORIENTED_EDGE('',*,*,#19775,.T.);
#26324=ORIENTED_EDGE('',*,*,#19782,.T.);
#26325=ORIENTED_EDGE('',*,*,#19772,.T.);
#26326=ORIENTED_EDGE('',*,*,#19783,.T.);
#26327=ORIENTED_EDGE('',*,*,#19765,.T.);
#26328=ORIENTED_EDGE('',*,*,#19784,.T.);
#26329=ORIENTED_EDGE('',*,*,#19770,.T.);
#26330=ORIENTED_EDGE('',*,*,#19785,.T.);
#26331=ORIENTED_EDGE('',*,*,#17987,.T.);
#26332=ORIENTED_EDGE('',*,*,#19786,.T.);
#26333=ORIENTED_EDGE('',*,*,#19769,.T.);
#26334=ORIENTED_EDGE('',*,*,#19787,.T.);
#26335=ORIENTED_EDGE('',*,*,#19767,.T.);
#26336=ORIENTED_EDGE('',*,*,#19788,.T.);
#26337=ORIENTED_EDGE('',*,*,#19766,.T.);
#26338=ORIENTED_EDGE('',*,*,#19789,.T.);
#26339=ORIENTED_EDGE('',*,*,#17985,.T.);
#26340=ORIENTED_EDGE('',*,*,#19790,.T.);
#26341=ORIENTED_EDGE('',*,*,#19764,.T.);
#26342=ORIENTED_EDGE('',*,*,#19791,.T.);
#26343=ORIENTED_EDGE('',*,*,#19779,.F.);
#26344=ORIENTED_EDGE('',*,*,#19783,.F.);
#26345=ORIENTED_EDGE('',*,*,#19773,.F.);
#26346=ORIENTED_EDGE('',*,*,#17982,.F.);
#26347=ORIENTED_EDGE('',*,*,#19774,.F.);
#26348=ORIENTED_EDGE('',*,*,#19784,.F.);
#26349=ORIENTED_EDGE('',*,*,#19790,.F.);
#26350=ORIENTED_EDGE('',*,*,#17984,.F.);
#26351=ORIENTED_EDGE('',*,*,#19780,.F.);
#26352=ORIENTED_EDGE('',*,*,#19789,.F.);
#26353=ORIENTED_EDGE('',*,*,#19785,.F.);
#26354=ORIENTED_EDGE('',*,*,#19782,.F.);
#26355=ORIENTED_EDGE('',*,*,#19792,.F.);
#26356=ORIENTED_EDGE('',*,*,#19793,.F.);
#26357=ORIENTED_EDGE('',*,*,#19794,.F.);
#26358=ORIENTED_EDGE('',*,*,#19795,.F.);
#26359=ORIENTED_EDGE('',*,*,#19796,.F.);
#26360=ORIENTED_EDGE('',*,*,#19797,.F.);
#26361=ORIENTED_EDGE('',*,*,#19798,.F.);
#26362=ORIENTED_EDGE('',*,*,#19799,.F.);
#26363=ORIENTED_EDGE('',*,*,#19800,.F.);
#26364=ORIENTED_EDGE('',*,*,#17991,.T.);
#26365=ORIENTED_EDGE('',*,*,#19801,.T.);
#26366=ORIENTED_EDGE('',*,*,#19799,.T.);
#26367=ORIENTED_EDGE('',*,*,#19802,.T.);
#26368=ORIENTED_EDGE('',*,*,#19803,.F.);
#26369=ORIENTED_EDGE('',*,*,#19804,.F.);
#26370=ORIENTED_EDGE('',*,*,#19805,.F.);
#26371=ORIENTED_EDGE('',*,*,#17989,.T.);
#26372=ORIENTED_EDGE('',*,*,#19806,.T.);
#26373=ORIENTED_EDGE('',*,*,#19804,.T.);
#26374=ORIENTED_EDGE('',*,*,#19807,.T.);
#26375=ORIENTED_EDGE('',*,*,#19796,.T.);
#26376=ORIENTED_EDGE('',*,*,#19808,.T.);
#26377=ORIENTED_EDGE('',*,*,#19805,.T.);
#26378=ORIENTED_EDGE('',*,*,#19809,.T.);
#26379=ORIENTED_EDGE('',*,*,#19803,.T.);
#26380=ORIENTED_EDGE('',*,*,#19810,.T.);
#26381=ORIENTED_EDGE('',*,*,#19800,.T.);
#26382=ORIENTED_EDGE('',*,*,#19811,.T.);
#26383=ORIENTED_EDGE('',*,*,#19793,.T.);
#26384=ORIENTED_EDGE('',*,*,#19812,.T.);
#26385=ORIENTED_EDGE('',*,*,#19798,.T.);
#26386=ORIENTED_EDGE('',*,*,#19813,.T.);
#26387=ORIENTED_EDGE('',*,*,#17995,.T.);
#26388=ORIENTED_EDGE('',*,*,#19814,.T.);
#26389=ORIENTED_EDGE('',*,*,#19797,.T.);
#26390=ORIENTED_EDGE('',*,*,#19815,.T.);
#26391=ORIENTED_EDGE('',*,*,#19795,.T.);
#26392=ORIENTED_EDGE('',*,*,#19816,.T.);
#26393=ORIENTED_EDGE('',*,*,#19794,.T.);
#26394=ORIENTED_EDGE('',*,*,#19817,.T.);
#26395=ORIENTED_EDGE('',*,*,#17993,.T.);
#26396=ORIENTED_EDGE('',*,*,#19818,.T.);
#26397=ORIENTED_EDGE('',*,*,#19792,.T.);
#26398=ORIENTED_EDGE('',*,*,#19819,.T.);
#26399=ORIENTED_EDGE('',*,*,#19807,.F.);
#26400=ORIENTED_EDGE('',*,*,#19811,.F.);
#26401=ORIENTED_EDGE('',*,*,#19801,.F.);
#26402=ORIENTED_EDGE('',*,*,#17990,.F.);
#26403=ORIENTED_EDGE('',*,*,#19802,.F.);
#26404=ORIENTED_EDGE('',*,*,#19812,.F.);
#26405=ORIENTED_EDGE('',*,*,#19818,.F.);
#26406=ORIENTED_EDGE('',*,*,#17992,.F.);
#26407=ORIENTED_EDGE('',*,*,#19808,.F.);
#26408=ORIENTED_EDGE('',*,*,#19817,.F.);
#26409=ORIENTED_EDGE('',*,*,#19813,.F.);
#26410=ORIENTED_EDGE('',*,*,#19810,.F.);
#26411=ORIENTED_EDGE('',*,*,#19820,.T.);
#26412=ORIENTED_EDGE('',*,*,#19821,.T.);
#26413=ORIENTED_EDGE('',*,*,#18001,.T.);
#26414=ORIENTED_EDGE('',*,*,#19822,.T.);
#26415=ORIENTED_EDGE('',*,*,#19823,.T.);
#26416=ORIENTED_EDGE('',*,*,#19821,.F.);
#26417=ORIENTED_EDGE('',*,*,#19824,.F.);
#26418=ORIENTED_EDGE('',*,*,#19825,.F.);
#26419=ORIENTED_EDGE('',*,*,#18002,.F.);
#26420=ORIENTED_EDGE('',*,*,#19820,.F.);
#26421=ORIENTED_EDGE('',*,*,#19826,.F.);
#26422=ORIENTED_EDGE('',*,*,#19827,.T.);
#26423=ORIENTED_EDGE('',*,*,#19828,.T.);
#26424=ORIENTED_EDGE('',*,*,#19824,.T.);
#26425=ORIENTED_EDGE('',*,*,#19823,.F.);
#26426=ORIENTED_EDGE('',*,*,#19829,.T.);
#26427=ORIENTED_EDGE('',*,*,#19830,.T.);
#26428=ORIENTED_EDGE('',*,*,#19831,.T.);
#26429=ORIENTED_EDGE('',*,*,#19826,.T.);
#26430=ORIENTED_EDGE('',*,*,#19828,.F.);
#26431=ORIENTED_EDGE('',*,*,#19832,.F.);
#26432=ORIENTED_EDGE('',*,*,#19833,.F.);
#26433=ORIENTED_EDGE('',*,*,#19830,.F.);
#26434=ORIENTED_EDGE('',*,*,#19834,.F.);
#26435=ORIENTED_EDGE('',*,*,#19835,.F.);
#26436=ORIENTED_EDGE('',*,*,#17999,.T.);
#26437=ORIENTED_EDGE('',*,*,#19836,.T.);
#26438=ORIENTED_EDGE('',*,*,#19834,.T.);
#26439=ORIENTED_EDGE('',*,*,#19837,.T.);
#26440=ORIENTED_EDGE('',*,*,#19838,.F.);
#26441=ORIENTED_EDGE('',*,*,#19839,.F.);
#26442=ORIENTED_EDGE('',*,*,#19840,.F.);
#26443=ORIENTED_EDGE('',*,*,#17997,.T.);
#26444=ORIENTED_EDGE('',*,*,#19841,.T.);
#26445=ORIENTED_EDGE('',*,*,#19839,.T.);
#26446=ORIENTED_EDGE('',*,*,#19842,.T.);
#26447=ORIENTED_EDGE('',*,*,#19832,.T.);
#26448=ORIENTED_EDGE('',*,*,#19843,.T.);
#26449=ORIENTED_EDGE('',*,*,#19840,.T.);
#26450=ORIENTED_EDGE('',*,*,#19844,.T.);
#26451=ORIENTED_EDGE('',*,*,#19838,.T.);
#26452=ORIENTED_EDGE('',*,*,#19845,.T.);
#26453=ORIENTED_EDGE('',*,*,#19835,.T.);
#26454=ORIENTED_EDGE('',*,*,#19846,.T.);
#26455=ORIENTED_EDGE('',*,*,#18003,.T.);
#26456=ORIENTED_EDGE('',*,*,#19825,.T.);
#26457=ORIENTED_EDGE('',*,*,#19833,.T.);
#26458=ORIENTED_EDGE('',*,*,#19847,.T.);
#26459=ORIENTED_EDGE('',*,*,#19822,.F.);
#26460=ORIENTED_EDGE('',*,*,#18000,.F.);
#26461=ORIENTED_EDGE('',*,*,#19837,.F.);
#26462=ORIENTED_EDGE('',*,*,#19829,.F.);
#26463=ORIENTED_EDGE('',*,*,#19843,.F.);
#26464=ORIENTED_EDGE('',*,*,#19827,.F.);
#26465=ORIENTED_EDGE('',*,*,#19831,.F.);
#26466=ORIENTED_EDGE('',*,*,#19845,.F.);
#26467=ORIENTED_EDGE('',*,*,#19848,.F.);
#26468=ORIENTED_EDGE('',*,*,#19849,.F.);
#26469=ORIENTED_EDGE('',*,*,#19850,.F.);
#26470=ORIENTED_EDGE('',*,*,#19851,.F.);
#26471=ORIENTED_EDGE('',*,*,#19852,.F.);
#26472=ORIENTED_EDGE('',*,*,#19853,.F.);
#26473=ORIENTED_EDGE('',*,*,#19854,.F.);
#26474=ORIENTED_EDGE('',*,*,#19855,.F.);
#26475=ORIENTED_EDGE('',*,*,#19856,.F.);
#26476=ORIENTED_EDGE('',*,*,#18007,.T.);
#26477=ORIENTED_EDGE('',*,*,#19857,.T.);
#26478=ORIENTED_EDGE('',*,*,#19855,.T.);
#26479=ORIENTED_EDGE('',*,*,#19858,.T.);
#26480=ORIENTED_EDGE('',*,*,#19859,.F.);
#26481=ORIENTED_EDGE('',*,*,#19860,.F.);
#26482=ORIENTED_EDGE('',*,*,#19861,.F.);
#26483=ORIENTED_EDGE('',*,*,#18005,.T.);
#26484=ORIENTED_EDGE('',*,*,#19862,.T.);
#26485=ORIENTED_EDGE('',*,*,#19860,.T.);
#26486=ORIENTED_EDGE('',*,*,#19863,.T.);
#26487=ORIENTED_EDGE('',*,*,#19852,.T.);
#26488=ORIENTED_EDGE('',*,*,#19864,.T.);
#26489=ORIENTED_EDGE('',*,*,#19861,.T.);
#26490=ORIENTED_EDGE('',*,*,#19865,.T.);
#26491=ORIENTED_EDGE('',*,*,#19859,.T.);
#26492=ORIENTED_EDGE('',*,*,#19866,.T.);
#26493=ORIENTED_EDGE('',*,*,#19856,.T.);
#26494=ORIENTED_EDGE('',*,*,#19867,.T.);
#26495=ORIENTED_EDGE('',*,*,#19849,.T.);
#26496=ORIENTED_EDGE('',*,*,#19868,.T.);
#26497=ORIENTED_EDGE('',*,*,#19854,.T.);
#26498=ORIENTED_EDGE('',*,*,#19869,.T.);
#26499=ORIENTED_EDGE('',*,*,#18011,.T.);
#26500=ORIENTED_EDGE('',*,*,#19870,.T.);
#26501=ORIENTED_EDGE('',*,*,#19853,.T.);
#26502=ORIENTED_EDGE('',*,*,#19871,.T.);
#26503=ORIENTED_EDGE('',*,*,#19851,.T.);
#26504=ORIENTED_EDGE('',*,*,#19872,.T.);
#26505=ORIENTED_EDGE('',*,*,#19850,.T.);
#26506=ORIENTED_EDGE('',*,*,#19873,.T.);
#26507=ORIENTED_EDGE('',*,*,#18009,.T.);
#26508=ORIENTED_EDGE('',*,*,#19874,.T.);
#26509=ORIENTED_EDGE('',*,*,#19848,.T.);
#26510=ORIENTED_EDGE('',*,*,#19875,.T.);
#26511=ORIENTED_EDGE('',*,*,#19863,.F.);
#26512=ORIENTED_EDGE('',*,*,#19867,.F.);
#26513=ORIENTED_EDGE('',*,*,#19857,.F.);
#26514=ORIENTED_EDGE('',*,*,#18006,.F.);
#26515=ORIENTED_EDGE('',*,*,#19858,.F.);
#26516=ORIENTED_EDGE('',*,*,#19868,.F.);
#26517=ORIENTED_EDGE('',*,*,#19874,.F.);
#26518=ORIENTED_EDGE('',*,*,#18008,.F.);
#26519=ORIENTED_EDGE('',*,*,#19864,.F.);
#26520=ORIENTED_EDGE('',*,*,#19873,.F.);
#26521=ORIENTED_EDGE('',*,*,#19869,.F.);
#26522=ORIENTED_EDGE('',*,*,#19866,.F.);
#26523=ORIENTED_EDGE('',*,*,#19876,.F.);
#26524=ORIENTED_EDGE('',*,*,#19877,.F.);
#26525=ORIENTED_EDGE('',*,*,#19878,.F.);
#26526=ORIENTED_EDGE('',*,*,#19879,.T.);
#26527=ORIENTED_EDGE('',*,*,#19880,.T.);
#26528=ORIENTED_EDGE('',*,*,#19877,.T.);
#26529=ORIENTED_EDGE('',*,*,#19881,.T.);
#26530=ORIENTED_EDGE('',*,*,#19882,.T.);
#26531=ORIENTED_EDGE('',*,*,#18019,.T.);
#26532=ORIENTED_EDGE('',*,*,#19883,.T.);
#26533=ORIENTED_EDGE('',*,*,#19878,.T.);
#26534=ORIENTED_EDGE('',*,*,#19884,.T.);
#26535=ORIENTED_EDGE('',*,*,#19885,.F.);
#26536=ORIENTED_EDGE('',*,*,#19886,.F.);
#26537=ORIENTED_EDGE('',*,*,#19887,.F.);
#26538=ORIENTED_EDGE('',*,*,#19888,.T.);
#26539=ORIENTED_EDGE('',*,*,#19889,.T.);
#26540=ORIENTED_EDGE('',*,*,#19886,.T.);
#26541=ORIENTED_EDGE('',*,*,#19890,.T.);
#26542=ORIENTED_EDGE('',*,*,#19891,.T.);
#26543=ORIENTED_EDGE('',*,*,#19876,.T.);
#26544=ORIENTED_EDGE('',*,*,#19892,.T.);
#26545=ORIENTED_EDGE('',*,*,#19887,.T.);
#26546=ORIENTED_EDGE('',*,*,#19893,.T.);
#26547=ORIENTED_EDGE('',*,*,#18017,.T.);
#26548=ORIENTED_EDGE('',*,*,#19894,.T.);
#26549=ORIENTED_EDGE('',*,*,#19885,.T.);
#26550=ORIENTED_EDGE('',*,*,#19895,.T.);
#26551=ORIENTED_EDGE('',*,*,#19879,.F.);
#26552=ORIENTED_EDGE('',*,*,#19896,.T.);
#26553=ORIENTED_EDGE('',*,*,#19897,.T.);
#26554=ORIENTED_EDGE('',*,*,#18013,.T.);
#26555=ORIENTED_EDGE('',*,*,#19898,.T.);
#26556=ORIENTED_EDGE('',*,*,#19881,.F.);
#26557=ORIENTED_EDGE('',*,*,#19893,.F.);
#26558=ORIENTED_EDGE('',*,*,#19889,.F.);
#26559=ORIENTED_EDGE('',*,*,#19899,.F.);
#26560=ORIENTED_EDGE('',*,*,#19882,.F.);
#26561=ORIENTED_EDGE('',*,*,#19899,.T.);
#26562=ORIENTED_EDGE('',*,*,#19888,.F.);
#26563=ORIENTED_EDGE('',*,*,#19900,.F.);
#26564=ORIENTED_EDGE('',*,*,#19901,.T.);
#26565=ORIENTED_EDGE('',*,*,#19896,.F.);
#26566=ORIENTED_EDGE('',*,*,#19891,.F.);
#26567=ORIENTED_EDGE('',*,*,#19902,.T.);
#26568=ORIENTED_EDGE('',*,*,#18015,.T.);
#26569=ORIENTED_EDGE('',*,*,#19903,.T.);
#26570=ORIENTED_EDGE('',*,*,#19900,.T.);
#26571=ORIENTED_EDGE('',*,*,#19890,.F.);
#26572=ORIENTED_EDGE('',*,*,#19894,.F.);
#26573=ORIENTED_EDGE('',*,*,#18016,.F.);
#26574=ORIENTED_EDGE('',*,*,#19902,.F.);
#26575=ORIENTED_EDGE('',*,*,#19880,.F.);
#26576=ORIENTED_EDGE('',*,*,#19898,.F.);
#26577=ORIENTED_EDGE('',*,*,#18012,.F.);
#26578=ORIENTED_EDGE('',*,*,#19884,.F.);
#26579=ORIENTED_EDGE('',*,*,#19904,.F.);
#26580=ORIENTED_EDGE('',*,*,#19905,.F.);
#26581=ORIENTED_EDGE('',*,*,#19906,.F.);
#26582=ORIENTED_EDGE('',*,*,#19907,.F.);
#26583=ORIENTED_EDGE('',*,*,#19908,.F.);
#26584=ORIENTED_EDGE('',*,*,#19909,.F.);
#26585=ORIENTED_EDGE('',*,*,#19910,.F.);
#26586=ORIENTED_EDGE('',*,*,#19911,.F.);
#26587=ORIENTED_EDGE('',*,*,#19912,.F.);
#26588=ORIENTED_EDGE('',*,*,#18023,.T.);
#26589=ORIENTED_EDGE('',*,*,#19913,.T.);
#26590=ORIENTED_EDGE('',*,*,#19911,.T.);
#26591=ORIENTED_EDGE('',*,*,#19914,.T.);
#26592=ORIENTED_EDGE('',*,*,#19915,.F.);
#26593=ORIENTED_EDGE('',*,*,#19916,.F.);
#26594=ORIENTED_EDGE('',*,*,#19917,.F.);
#26595=ORIENTED_EDGE('',*,*,#18021,.T.);
#26596=ORIENTED_EDGE('',*,*,#19918,.T.);
#26597=ORIENTED_EDGE('',*,*,#19916,.T.);
#26598=ORIENTED_EDGE('',*,*,#19919,.T.);
#26599=ORIENTED_EDGE('',*,*,#19908,.T.);
#26600=ORIENTED_EDGE('',*,*,#19920,.T.);
#26601=ORIENTED_EDGE('',*,*,#19917,.T.);
#26602=ORIENTED_EDGE('',*,*,#19921,.T.);
#26603=ORIENTED_EDGE('',*,*,#19915,.T.);
#26604=ORIENTED_EDGE('',*,*,#19922,.T.);
#26605=ORIENTED_EDGE('',*,*,#19912,.T.);
#26606=ORIENTED_EDGE('',*,*,#19923,.T.);
#26607=ORIENTED_EDGE('',*,*,#19905,.T.);
#26608=ORIENTED_EDGE('',*,*,#19924,.T.);
#26609=ORIENTED_EDGE('',*,*,#19910,.T.);
#26610=ORIENTED_EDGE('',*,*,#19925,.T.);
#26611=ORIENTED_EDGE('',*,*,#18027,.T.);
#26612=ORIENTED_EDGE('',*,*,#19926,.T.);
#26613=ORIENTED_EDGE('',*,*,#19909,.T.);
#26614=ORIENTED_EDGE('',*,*,#19927,.T.);
#26615=ORIENTED_EDGE('',*,*,#19907,.T.);
#26616=ORIENTED_EDGE('',*,*,#19928,.T.);
#26617=ORIENTED_EDGE('',*,*,#19906,.T.);
#26618=ORIENTED_EDGE('',*,*,#19929,.T.);
#26619=ORIENTED_EDGE('',*,*,#18025,.T.);
#26620=ORIENTED_EDGE('',*,*,#19930,.T.);
#26621=ORIENTED_EDGE('',*,*,#19904,.T.);
#26622=ORIENTED_EDGE('',*,*,#19931,.T.);
#26623=ORIENTED_EDGE('',*,*,#19919,.F.);
#26624=ORIENTED_EDGE('',*,*,#19923,.F.);
#26625=ORIENTED_EDGE('',*,*,#19913,.F.);
#26626=ORIENTED_EDGE('',*,*,#18022,.F.);
#26627=ORIENTED_EDGE('',*,*,#19914,.F.);
#26628=ORIENTED_EDGE('',*,*,#19924,.F.);
#26629=ORIENTED_EDGE('',*,*,#19930,.F.);
#26630=ORIENTED_EDGE('',*,*,#18024,.F.);
#26631=ORIENTED_EDGE('',*,*,#19920,.F.);
#26632=ORIENTED_EDGE('',*,*,#19929,.F.);
#26633=ORIENTED_EDGE('',*,*,#19925,.F.);
#26634=ORIENTED_EDGE('',*,*,#19922,.F.);
#26635=ORIENTED_EDGE('',*,*,#19932,.F.);
#26636=ORIENTED_EDGE('',*,*,#19933,.F.);
#26637=ORIENTED_EDGE('',*,*,#19934,.F.);
#26638=ORIENTED_EDGE('',*,*,#19935,.F.);
#26639=ORIENTED_EDGE('',*,*,#19936,.F.);
#26640=ORIENTED_EDGE('',*,*,#19937,.F.);
#26641=ORIENTED_EDGE('',*,*,#19938,.F.);
#26642=ORIENTED_EDGE('',*,*,#19939,.F.);
#26643=ORIENTED_EDGE('',*,*,#19940,.F.);
#26644=ORIENTED_EDGE('',*,*,#18031,.T.);
#26645=ORIENTED_EDGE('',*,*,#19941,.T.);
#26646=ORIENTED_EDGE('',*,*,#19939,.T.);
#26647=ORIENTED_EDGE('',*,*,#19942,.T.);
#26648=ORIENTED_EDGE('',*,*,#19943,.F.);
#26649=ORIENTED_EDGE('',*,*,#19944,.F.);
#26650=ORIENTED_EDGE('',*,*,#19945,.F.);
#26651=ORIENTED_EDGE('',*,*,#18029,.T.);
#26652=ORIENTED_EDGE('',*,*,#19946,.T.);
#26653=ORIENTED_EDGE('',*,*,#19944,.T.);
#26654=ORIENTED_EDGE('',*,*,#19947,.T.);
#26655=ORIENTED_EDGE('',*,*,#19936,.T.);
#26656=ORIENTED_EDGE('',*,*,#19948,.T.);
#26657=ORIENTED_EDGE('',*,*,#19945,.T.);
#26658=ORIENTED_EDGE('',*,*,#19949,.T.);
#26659=ORIENTED_EDGE('',*,*,#19943,.T.);
#26660=ORIENTED_EDGE('',*,*,#19950,.T.);
#26661=ORIENTED_EDGE('',*,*,#19940,.T.);
#26662=ORIENTED_EDGE('',*,*,#19951,.T.);
#26663=ORIENTED_EDGE('',*,*,#19933,.T.);
#26664=ORIENTED_EDGE('',*,*,#19952,.T.);
#26665=ORIENTED_EDGE('',*,*,#19938,.T.);
#26666=ORIENTED_EDGE('',*,*,#19953,.T.);
#26667=ORIENTED_EDGE('',*,*,#18035,.T.);
#26668=ORIENTED_EDGE('',*,*,#19954,.T.);
#26669=ORIENTED_EDGE('',*,*,#19937,.T.);
#26670=ORIENTED_EDGE('',*,*,#19955,.T.);
#26671=ORIENTED_EDGE('',*,*,#19935,.T.);
#26672=ORIENTED_EDGE('',*,*,#19956,.T.);
#26673=ORIENTED_EDGE('',*,*,#19934,.T.);
#26674=ORIENTED_EDGE('',*,*,#19957,.T.);
#26675=ORIENTED_EDGE('',*,*,#18033,.T.);
#26676=ORIENTED_EDGE('',*,*,#19958,.T.);
#26677=ORIENTED_EDGE('',*,*,#19932,.T.);
#26678=ORIENTED_EDGE('',*,*,#19959,.T.);
#26679=ORIENTED_EDGE('',*,*,#19947,.F.);
#26680=ORIENTED_EDGE('',*,*,#19951,.F.);
#26681=ORIENTED_EDGE('',*,*,#19941,.F.);
#26682=ORIENTED_EDGE('',*,*,#18030,.F.);
#26683=ORIENTED_EDGE('',*,*,#19942,.F.);
#26684=ORIENTED_EDGE('',*,*,#19952,.F.);
#26685=ORIENTED_EDGE('',*,*,#19958,.F.);
#26686=ORIENTED_EDGE('',*,*,#18032,.F.);
#26687=ORIENTED_EDGE('',*,*,#19948,.F.);
#26688=ORIENTED_EDGE('',*,*,#19957,.F.);
#26689=ORIENTED_EDGE('',*,*,#19953,.F.);
#26690=ORIENTED_EDGE('',*,*,#19950,.F.);
#26691=ORIENTED_EDGE('',*,*,#19960,.T.);
#26692=ORIENTED_EDGE('',*,*,#19961,.T.);
#26693=ORIENTED_EDGE('',*,*,#18041,.T.);
#26694=ORIENTED_EDGE('',*,*,#19962,.T.);
#26695=ORIENTED_EDGE('',*,*,#19963,.T.);
#26696=ORIENTED_EDGE('',*,*,#19961,.F.);
#26697=ORIENTED_EDGE('',*,*,#19964,.F.);
#26698=ORIENTED_EDGE('',*,*,#19965,.F.);
#26699=ORIENTED_EDGE('',*,*,#18042,.F.);
#26700=ORIENTED_EDGE('',*,*,#19960,.F.);
#26701=ORIENTED_EDGE('',*,*,#19966,.F.);
#26702=ORIENTED_EDGE('',*,*,#19967,.T.);
#26703=ORIENTED_EDGE('',*,*,#19968,.T.);
#26704=ORIENTED_EDGE('',*,*,#19964,.T.);
#26705=ORIENTED_EDGE('',*,*,#19963,.F.);
#26706=ORIENTED_EDGE('',*,*,#19969,.T.);
#26707=ORIENTED_EDGE('',*,*,#19970,.T.);
#26708=ORIENTED_EDGE('',*,*,#19971,.T.);
#26709=ORIENTED_EDGE('',*,*,#19966,.T.);
#26710=ORIENTED_EDGE('',*,*,#19968,.F.);
#26711=ORIENTED_EDGE('',*,*,#19972,.F.);
#26712=ORIENTED_EDGE('',*,*,#19973,.F.);
#26713=ORIENTED_EDGE('',*,*,#19970,.F.);
#26714=ORIENTED_EDGE('',*,*,#19974,.F.);
#26715=ORIENTED_EDGE('',*,*,#19975,.F.);
#26716=ORIENTED_EDGE('',*,*,#18039,.T.);
#26717=ORIENTED_EDGE('',*,*,#19976,.T.);
#26718=ORIENTED_EDGE('',*,*,#19974,.T.);
#26719=ORIENTED_EDGE('',*,*,#19977,.T.);
#26720=ORIENTED_EDGE('',*,*,#19978,.F.);
#26721=ORIENTED_EDGE('',*,*,#19979,.F.);
#26722=ORIENTED_EDGE('',*,*,#19980,.F.);
#26723=ORIENTED_EDGE('',*,*,#18037,.T.);
#26724=ORIENTED_EDGE('',*,*,#19981,.T.);
#26725=ORIENTED_EDGE('',*,*,#19979,.T.);
#26726=ORIENTED_EDGE('',*,*,#19982,.T.);
#26727=ORIENTED_EDGE('',*,*,#19972,.T.);
#26728=ORIENTED_EDGE('',*,*,#19983,.T.);
#26729=ORIENTED_EDGE('',*,*,#19980,.T.);
#26730=ORIENTED_EDGE('',*,*,#19984,.T.);
#26731=ORIENTED_EDGE('',*,*,#19978,.T.);
#26732=ORIENTED_EDGE('',*,*,#19985,.T.);
#26733=ORIENTED_EDGE('',*,*,#19975,.T.);
#26734=ORIENTED_EDGE('',*,*,#19986,.T.);
#26735=ORIENTED_EDGE('',*,*,#18043,.T.);
#26736=ORIENTED_EDGE('',*,*,#19965,.T.);
#26737=ORIENTED_EDGE('',*,*,#19973,.T.);
#26738=ORIENTED_EDGE('',*,*,#19987,.T.);
#26739=ORIENTED_EDGE('',*,*,#19962,.F.);
#26740=ORIENTED_EDGE('',*,*,#18040,.F.);
#26741=ORIENTED_EDGE('',*,*,#19977,.F.);
#26742=ORIENTED_EDGE('',*,*,#19969,.F.);
#26743=ORIENTED_EDGE('',*,*,#19983,.F.);
#26744=ORIENTED_EDGE('',*,*,#19967,.F.);
#26745=ORIENTED_EDGE('',*,*,#19971,.F.);
#26746=ORIENTED_EDGE('',*,*,#19985,.F.);
#26747=ORIENTED_EDGE('',*,*,#19988,.F.);
#26748=ORIENTED_EDGE('',*,*,#19989,.F.);
#26749=ORIENTED_EDGE('',*,*,#19990,.F.);
#26750=ORIENTED_EDGE('',*,*,#19991,.F.);
#26751=ORIENTED_EDGE('',*,*,#19992,.F.);
#26752=ORIENTED_EDGE('',*,*,#19993,.F.);
#26753=ORIENTED_EDGE('',*,*,#19994,.F.);
#26754=ORIENTED_EDGE('',*,*,#19995,.F.);
#26755=ORIENTED_EDGE('',*,*,#19996,.F.);
#26756=ORIENTED_EDGE('',*,*,#18047,.T.);
#26757=ORIENTED_EDGE('',*,*,#19997,.T.);
#26758=ORIENTED_EDGE('',*,*,#19995,.T.);
#26759=ORIENTED_EDGE('',*,*,#19998,.T.);
#26760=ORIENTED_EDGE('',*,*,#19999,.F.);
#26761=ORIENTED_EDGE('',*,*,#20000,.F.);
#26762=ORIENTED_EDGE('',*,*,#20001,.F.);
#26763=ORIENTED_EDGE('',*,*,#18045,.T.);
#26764=ORIENTED_EDGE('',*,*,#20002,.T.);
#26765=ORIENTED_EDGE('',*,*,#20000,.T.);
#26766=ORIENTED_EDGE('',*,*,#20003,.T.);
#26767=ORIENTED_EDGE('',*,*,#19992,.T.);
#26768=ORIENTED_EDGE('',*,*,#20004,.T.);
#26769=ORIENTED_EDGE('',*,*,#20001,.T.);
#26770=ORIENTED_EDGE('',*,*,#20005,.T.);
#26771=ORIENTED_EDGE('',*,*,#19999,.T.);
#26772=ORIENTED_EDGE('',*,*,#20006,.T.);
#26773=ORIENTED_EDGE('',*,*,#19996,.T.);
#26774=ORIENTED_EDGE('',*,*,#20007,.T.);
#26775=ORIENTED_EDGE('',*,*,#19989,.T.);
#26776=ORIENTED_EDGE('',*,*,#20008,.T.);
#26777=ORIENTED_EDGE('',*,*,#19994,.T.);
#26778=ORIENTED_EDGE('',*,*,#20009,.T.);
#26779=ORIENTED_EDGE('',*,*,#18051,.T.);
#26780=ORIENTED_EDGE('',*,*,#20010,.T.);
#26781=ORIENTED_EDGE('',*,*,#19993,.T.);
#26782=ORIENTED_EDGE('',*,*,#20011,.T.);
#26783=ORIENTED_EDGE('',*,*,#19991,.T.);
#26784=ORIENTED_EDGE('',*,*,#20012,.T.);
#26785=ORIENTED_EDGE('',*,*,#19990,.T.);
#26786=ORIENTED_EDGE('',*,*,#20013,.T.);
#26787=ORIENTED_EDGE('',*,*,#18049,.T.);
#26788=ORIENTED_EDGE('',*,*,#20014,.T.);
#26789=ORIENTED_EDGE('',*,*,#19988,.T.);
#26790=ORIENTED_EDGE('',*,*,#20015,.T.);
#26791=ORIENTED_EDGE('',*,*,#20003,.F.);
#26792=ORIENTED_EDGE('',*,*,#20007,.F.);
#26793=ORIENTED_EDGE('',*,*,#19997,.F.);
#26794=ORIENTED_EDGE('',*,*,#18046,.F.);
#26795=ORIENTED_EDGE('',*,*,#19998,.F.);
#26796=ORIENTED_EDGE('',*,*,#20008,.F.);
#26797=ORIENTED_EDGE('',*,*,#20014,.F.);
#26798=ORIENTED_EDGE('',*,*,#18048,.F.);
#26799=ORIENTED_EDGE('',*,*,#20004,.F.);
#26800=ORIENTED_EDGE('',*,*,#20013,.F.);
#26801=ORIENTED_EDGE('',*,*,#20009,.F.);
#26802=ORIENTED_EDGE('',*,*,#20006,.F.);
#26803=ORIENTED_EDGE('',*,*,#20016,.F.);
#26804=ORIENTED_EDGE('',*,*,#20017,.F.);
#26805=ORIENTED_EDGE('',*,*,#20018,.F.);
#26806=ORIENTED_EDGE('',*,*,#20019,.T.);
#26807=ORIENTED_EDGE('',*,*,#20020,.T.);
#26808=ORIENTED_EDGE('',*,*,#20017,.T.);
#26809=ORIENTED_EDGE('',*,*,#20021,.T.);
#26810=ORIENTED_EDGE('',*,*,#20022,.T.);
#26811=ORIENTED_EDGE('',*,*,#18059,.T.);
#26812=ORIENTED_EDGE('',*,*,#20023,.T.);
#26813=ORIENTED_EDGE('',*,*,#20018,.T.);
#26814=ORIENTED_EDGE('',*,*,#20024,.T.);
#26815=ORIENTED_EDGE('',*,*,#20025,.F.);
#26816=ORIENTED_EDGE('',*,*,#20026,.F.);
#26817=ORIENTED_EDGE('',*,*,#20027,.F.);
#26818=ORIENTED_EDGE('',*,*,#20028,.T.);
#26819=ORIENTED_EDGE('',*,*,#20029,.T.);
#26820=ORIENTED_EDGE('',*,*,#20026,.T.);
#26821=ORIENTED_EDGE('',*,*,#20030,.T.);
#26822=ORIENTED_EDGE('',*,*,#20031,.T.);
#26823=ORIENTED_EDGE('',*,*,#20016,.T.);
#26824=ORIENTED_EDGE('',*,*,#20032,.T.);
#26825=ORIENTED_EDGE('',*,*,#20027,.T.);
#26826=ORIENTED_EDGE('',*,*,#20033,.T.);
#26827=ORIENTED_EDGE('',*,*,#18057,.T.);
#26828=ORIENTED_EDGE('',*,*,#20034,.T.);
#26829=ORIENTED_EDGE('',*,*,#20025,.T.);
#26830=ORIENTED_EDGE('',*,*,#20035,.T.);
#26831=ORIENTED_EDGE('',*,*,#20019,.F.);
#26832=ORIENTED_EDGE('',*,*,#20036,.T.);
#26833=ORIENTED_EDGE('',*,*,#20037,.T.);
#26834=ORIENTED_EDGE('',*,*,#18053,.T.);
#26835=ORIENTED_EDGE('',*,*,#20038,.T.);
#26836=ORIENTED_EDGE('',*,*,#20021,.F.);
#26837=ORIENTED_EDGE('',*,*,#20033,.F.);
#26838=ORIENTED_EDGE('',*,*,#20029,.F.);
#26839=ORIENTED_EDGE('',*,*,#20039,.F.);
#26840=ORIENTED_EDGE('',*,*,#20022,.F.);
#26841=ORIENTED_EDGE('',*,*,#20039,.T.);
#26842=ORIENTED_EDGE('',*,*,#20028,.F.);
#26843=ORIENTED_EDGE('',*,*,#20040,.F.);
#26844=ORIENTED_EDGE('',*,*,#20041,.T.);
#26845=ORIENTED_EDGE('',*,*,#20036,.F.);
#26846=ORIENTED_EDGE('',*,*,#20031,.F.);
#26847=ORIENTED_EDGE('',*,*,#20042,.T.);
#26848=ORIENTED_EDGE('',*,*,#18055,.T.);
#26849=ORIENTED_EDGE('',*,*,#20043,.T.);
#26850=ORIENTED_EDGE('',*,*,#20040,.T.);
#26851=ORIENTED_EDGE('',*,*,#20030,.F.);
#26852=ORIENTED_EDGE('',*,*,#20034,.F.);
#26853=ORIENTED_EDGE('',*,*,#18056,.F.);
#26854=ORIENTED_EDGE('',*,*,#20042,.F.);
#26855=ORIENTED_EDGE('',*,*,#20020,.F.);
#26856=ORIENTED_EDGE('',*,*,#20038,.F.);
#26857=ORIENTED_EDGE('',*,*,#18052,.F.);
#26858=ORIENTED_EDGE('',*,*,#20024,.F.);
#26859=ORIENTED_EDGE('',*,*,#20044,.F.);
#26860=ORIENTED_EDGE('',*,*,#20045,.F.);
#26861=ORIENTED_EDGE('',*,*,#20046,.F.);
#26862=ORIENTED_EDGE('',*,*,#20047,.F.);
#26863=ORIENTED_EDGE('',*,*,#20048,.F.);
#26864=ORIENTED_EDGE('',*,*,#20049,.F.);
#26865=ORIENTED_EDGE('',*,*,#20050,.F.);
#26866=ORIENTED_EDGE('',*,*,#20051,.F.);
#26867=ORIENTED_EDGE('',*,*,#20052,.F.);
#26868=ORIENTED_EDGE('',*,*,#18063,.T.);
#26869=ORIENTED_EDGE('',*,*,#20053,.T.);
#26870=ORIENTED_EDGE('',*,*,#20051,.T.);
#26871=ORIENTED_EDGE('',*,*,#20054,.T.);
#26872=ORIENTED_EDGE('',*,*,#20055,.F.);
#26873=ORIENTED_EDGE('',*,*,#20056,.F.);
#26874=ORIENTED_EDGE('',*,*,#20057,.F.);
#26875=ORIENTED_EDGE('',*,*,#18061,.T.);
#26876=ORIENTED_EDGE('',*,*,#20058,.T.);
#26877=ORIENTED_EDGE('',*,*,#20056,.T.);
#26878=ORIENTED_EDGE('',*,*,#20059,.T.);
#26879=ORIENTED_EDGE('',*,*,#20048,.T.);
#26880=ORIENTED_EDGE('',*,*,#20060,.T.);
#26881=ORIENTED_EDGE('',*,*,#20057,.T.);
#26882=ORIENTED_EDGE('',*,*,#20061,.T.);
#26883=ORIENTED_EDGE('',*,*,#20055,.T.);
#26884=ORIENTED_EDGE('',*,*,#20062,.T.);
#26885=ORIENTED_EDGE('',*,*,#20052,.T.);
#26886=ORIENTED_EDGE('',*,*,#20063,.T.);
#26887=ORIENTED_EDGE('',*,*,#20045,.T.);
#26888=ORIENTED_EDGE('',*,*,#20064,.T.);
#26889=ORIENTED_EDGE('',*,*,#20050,.T.);
#26890=ORIENTED_EDGE('',*,*,#20065,.T.);
#26891=ORIENTED_EDGE('',*,*,#18067,.T.);
#26892=ORIENTED_EDGE('',*,*,#20066,.T.);
#26893=ORIENTED_EDGE('',*,*,#20049,.T.);
#26894=ORIENTED_EDGE('',*,*,#20067,.T.);
#26895=ORIENTED_EDGE('',*,*,#20047,.T.);
#26896=ORIENTED_EDGE('',*,*,#20068,.T.);
#26897=ORIENTED_EDGE('',*,*,#20046,.T.);
#26898=ORIENTED_EDGE('',*,*,#20069,.T.);
#26899=ORIENTED_EDGE('',*,*,#18065,.T.);
#26900=ORIENTED_EDGE('',*,*,#20070,.T.);
#26901=ORIENTED_EDGE('',*,*,#20044,.T.);
#26902=ORIENTED_EDGE('',*,*,#20071,.T.);
#26903=ORIENTED_EDGE('',*,*,#20059,.F.);
#26904=ORIENTED_EDGE('',*,*,#20063,.F.);
#26905=ORIENTED_EDGE('',*,*,#20053,.F.);
#26906=ORIENTED_EDGE('',*,*,#18062,.F.);
#26907=ORIENTED_EDGE('',*,*,#20054,.F.);
#26908=ORIENTED_EDGE('',*,*,#20064,.F.);
#26909=ORIENTED_EDGE('',*,*,#20070,.F.);
#26910=ORIENTED_EDGE('',*,*,#18064,.F.);
#26911=ORIENTED_EDGE('',*,*,#20060,.F.);
#26912=ORIENTED_EDGE('',*,*,#20069,.F.);
#26913=ORIENTED_EDGE('',*,*,#20065,.F.);
#26914=ORIENTED_EDGE('',*,*,#20062,.F.);
#26915=ORIENTED_EDGE('',*,*,#20072,.F.);
#26916=ORIENTED_EDGE('',*,*,#20073,.F.);
#26917=ORIENTED_EDGE('',*,*,#20074,.F.);
#26918=ORIENTED_EDGE('',*,*,#20075,.F.);
#26919=ORIENTED_EDGE('',*,*,#20076,.F.);
#26920=ORIENTED_EDGE('',*,*,#20077,.F.);
#26921=ORIENTED_EDGE('',*,*,#20078,.F.);
#26922=ORIENTED_EDGE('',*,*,#20079,.F.);
#26923=ORIENTED_EDGE('',*,*,#20080,.F.);
#26924=ORIENTED_EDGE('',*,*,#18071,.T.);
#26925=ORIENTED_EDGE('',*,*,#20081,.T.);
#26926=ORIENTED_EDGE('',*,*,#20079,.T.);
#26927=ORIENTED_EDGE('',*,*,#20082,.T.);
#26928=ORIENTED_EDGE('',*,*,#20083,.F.);
#26929=ORIENTED_EDGE('',*,*,#20084,.F.);
#26930=ORIENTED_EDGE('',*,*,#20085,.F.);
#26931=ORIENTED_EDGE('',*,*,#18069,.T.);
#26932=ORIENTED_EDGE('',*,*,#20086,.T.);
#26933=ORIENTED_EDGE('',*,*,#20084,.T.);
#26934=ORIENTED_EDGE('',*,*,#20087,.T.);
#26935=ORIENTED_EDGE('',*,*,#20076,.T.);
#26936=ORIENTED_EDGE('',*,*,#20088,.T.);
#26937=ORIENTED_EDGE('',*,*,#20085,.T.);
#26938=ORIENTED_EDGE('',*,*,#20089,.T.);
#26939=ORIENTED_EDGE('',*,*,#20083,.T.);
#26940=ORIENTED_EDGE('',*,*,#20090,.T.);
#26941=ORIENTED_EDGE('',*,*,#20080,.T.);
#26942=ORIENTED_EDGE('',*,*,#20091,.T.);
#26943=ORIENTED_EDGE('',*,*,#20073,.T.);
#26944=ORIENTED_EDGE('',*,*,#20092,.T.);
#26945=ORIENTED_EDGE('',*,*,#20078,.T.);
#26946=ORIENTED_EDGE('',*,*,#20093,.T.);
#26947=ORIENTED_EDGE('',*,*,#18075,.T.);
#26948=ORIENTED_EDGE('',*,*,#20094,.T.);
#26949=ORIENTED_EDGE('',*,*,#20077,.T.);
#26950=ORIENTED_EDGE('',*,*,#20095,.T.);
#26951=ORIENTED_EDGE('',*,*,#20075,.T.);
#26952=ORIENTED_EDGE('',*,*,#20096,.T.);
#26953=ORIENTED_EDGE('',*,*,#20074,.T.);
#26954=ORIENTED_EDGE('',*,*,#20097,.T.);
#26955=ORIENTED_EDGE('',*,*,#18073,.T.);
#26956=ORIENTED_EDGE('',*,*,#20098,.T.);
#26957=ORIENTED_EDGE('',*,*,#20072,.T.);
#26958=ORIENTED_EDGE('',*,*,#20099,.T.);
#26959=ORIENTED_EDGE('',*,*,#20087,.F.);
#26960=ORIENTED_EDGE('',*,*,#20091,.F.);
#26961=ORIENTED_EDGE('',*,*,#20081,.F.);
#26962=ORIENTED_EDGE('',*,*,#18070,.F.);
#26963=ORIENTED_EDGE('',*,*,#20082,.F.);
#26964=ORIENTED_EDGE('',*,*,#20092,.F.);
#26965=ORIENTED_EDGE('',*,*,#20098,.F.);
#26966=ORIENTED_EDGE('',*,*,#18072,.F.);
#26967=ORIENTED_EDGE('',*,*,#20088,.F.);
#26968=ORIENTED_EDGE('',*,*,#20097,.F.);
#26969=ORIENTED_EDGE('',*,*,#20093,.F.);
#26970=ORIENTED_EDGE('',*,*,#20090,.F.);
#26971=ORIENTED_EDGE('',*,*,#20100,.T.);
#26972=ORIENTED_EDGE('',*,*,#20101,.T.);
#26973=ORIENTED_EDGE('',*,*,#20102,.T.);
#26974=ORIENTED_EDGE('',*,*,#20103,.T.);
#26975=ORIENTED_EDGE('',*,*,#20104,.T.);
#26976=ORIENTED_EDGE('',*,*,#20102,.F.);
#26977=ORIENTED_EDGE('',*,*,#20100,.F.);
#26978=ORIENTED_EDGE('',*,*,#20101,.F.);
#26979=ORIENTED_EDGE('',*,*,#20105,.T.);
#26980=ORIENTED_EDGE('',*,*,#20106,.F.);
#26981=ORIENTED_EDGE('',*,*,#20107,.F.);
#26982=ORIENTED_EDGE('',*,*,#20105,.F.);
#26983=ORIENTED_EDGE('',*,*,#20108,.T.);
#26984=ORIENTED_EDGE('',*,*,#20109,.T.);
#26985=ORIENTED_EDGE('',*,*,#20103,.F.);
#26986=ORIENTED_EDGE('',*,*,#20104,.F.);
#26987=ORIENTED_EDGE('',*,*,#20109,.F.);
#26988=ORIENTED_EDGE('',*,*,#20110,.F.);
#26989=ORIENTED_EDGE('',*,*,#20111,.F.);
#26990=ORIENTED_EDGE('',*,*,#20112,.F.);
#26991=ORIENTED_EDGE('',*,*,#20113,.F.);
#26992=ORIENTED_EDGE('',*,*,#20114,.F.);
#26993=ORIENTED_EDGE('',*,*,#20115,.F.);
#26994=ORIENTED_EDGE('',*,*,#20116,.F.);
#26995=ORIENTED_EDGE('',*,*,#20117,.F.);
#26996=ORIENTED_EDGE('',*,*,#20118,.F.);
#26997=ORIENTED_EDGE('',*,*,#18079,.T.);
#26998=ORIENTED_EDGE('',*,*,#20119,.T.);
#26999=ORIENTED_EDGE('',*,*,#20117,.T.);
#27000=ORIENTED_EDGE('',*,*,#20120,.T.);
#27001=ORIENTED_EDGE('',*,*,#20121,.F.);
#27002=ORIENTED_EDGE('',*,*,#20122,.F.);
#27003=ORIENTED_EDGE('',*,*,#20123,.F.);
#27004=ORIENTED_EDGE('',*,*,#18077,.T.);
#27005=ORIENTED_EDGE('',*,*,#20124,.T.);
#27006=ORIENTED_EDGE('',*,*,#20122,.T.);
#27007=ORIENTED_EDGE('',*,*,#20125,.T.);
#27008=ORIENTED_EDGE('',*,*,#20114,.T.);
#27009=ORIENTED_EDGE('',*,*,#20126,.T.);
#27010=ORIENTED_EDGE('',*,*,#20123,.T.);
#27011=ORIENTED_EDGE('',*,*,#20127,.T.);
#27012=ORIENTED_EDGE('',*,*,#20121,.T.);
#27013=ORIENTED_EDGE('',*,*,#20128,.T.);
#27014=ORIENTED_EDGE('',*,*,#20118,.T.);
#27015=ORIENTED_EDGE('',*,*,#20129,.T.);
#27016=ORIENTED_EDGE('',*,*,#20111,.T.);
#27017=ORIENTED_EDGE('',*,*,#20130,.T.);
#27018=ORIENTED_EDGE('',*,*,#20116,.T.);
#27019=ORIENTED_EDGE('',*,*,#20131,.T.);
#27020=ORIENTED_EDGE('',*,*,#18083,.T.);
#27021=ORIENTED_EDGE('',*,*,#20132,.T.);
#27022=ORIENTED_EDGE('',*,*,#20115,.T.);
#27023=ORIENTED_EDGE('',*,*,#20133,.T.);
#27024=ORIENTED_EDGE('',*,*,#20113,.T.);
#27025=ORIENTED_EDGE('',*,*,#20134,.T.);
#27026=ORIENTED_EDGE('',*,*,#20112,.T.);
#27027=ORIENTED_EDGE('',*,*,#20135,.T.);
#27028=ORIENTED_EDGE('',*,*,#18081,.T.);
#27029=ORIENTED_EDGE('',*,*,#20136,.T.);
#27030=ORIENTED_EDGE('',*,*,#20110,.T.);
#27031=ORIENTED_EDGE('',*,*,#20137,.T.);
#27032=ORIENTED_EDGE('',*,*,#20125,.F.);
#27033=ORIENTED_EDGE('',*,*,#20129,.F.);
#27034=ORIENTED_EDGE('',*,*,#20119,.F.);
#27035=ORIENTED_EDGE('',*,*,#18078,.F.);
#27036=ORIENTED_EDGE('',*,*,#20120,.F.);
#27037=ORIENTED_EDGE('',*,*,#20130,.F.);
#27038=ORIENTED_EDGE('',*,*,#20136,.F.);
#27039=ORIENTED_EDGE('',*,*,#18080,.F.);
#27040=ORIENTED_EDGE('',*,*,#20126,.F.);
#27041=ORIENTED_EDGE('',*,*,#20135,.F.);
#27042=ORIENTED_EDGE('',*,*,#20131,.F.);
#27043=ORIENTED_EDGE('',*,*,#20128,.F.);
#27044=ORIENTED_EDGE('',*,*,#20138,.F.);
#27045=ORIENTED_EDGE('',*,*,#20139,.F.);
#27046=ORIENTED_EDGE('',*,*,#20140,.F.);
#27047=ORIENTED_EDGE('',*,*,#20141,.F.);
#27048=ORIENTED_EDGE('',*,*,#20142,.F.);
#27049=ORIENTED_EDGE('',*,*,#20143,.F.);
#27050=ORIENTED_EDGE('',*,*,#20144,.F.);
#27051=ORIENTED_EDGE('',*,*,#20145,.F.);
#27052=ORIENTED_EDGE('',*,*,#20146,.F.);
#27053=ORIENTED_EDGE('',*,*,#18087,.T.);
#27054=ORIENTED_EDGE('',*,*,#20147,.T.);
#27055=ORIENTED_EDGE('',*,*,#20145,.T.);
#27056=ORIENTED_EDGE('',*,*,#20148,.T.);
#27057=ORIENTED_EDGE('',*,*,#20149,.F.);
#27058=ORIENTED_EDGE('',*,*,#20150,.F.);
#27059=ORIENTED_EDGE('',*,*,#20151,.F.);
#27060=ORIENTED_EDGE('',*,*,#18085,.T.);
#27061=ORIENTED_EDGE('',*,*,#20152,.T.);
#27062=ORIENTED_EDGE('',*,*,#20150,.T.);
#27063=ORIENTED_EDGE('',*,*,#20153,.T.);
#27064=ORIENTED_EDGE('',*,*,#20142,.T.);
#27065=ORIENTED_EDGE('',*,*,#20154,.T.);
#27066=ORIENTED_EDGE('',*,*,#20151,.T.);
#27067=ORIENTED_EDGE('',*,*,#20155,.T.);
#27068=ORIENTED_EDGE('',*,*,#20149,.T.);
#27069=ORIENTED_EDGE('',*,*,#20156,.T.);
#27070=ORIENTED_EDGE('',*,*,#20146,.T.);
#27071=ORIENTED_EDGE('',*,*,#20157,.T.);
#27072=ORIENTED_EDGE('',*,*,#20139,.T.);
#27073=ORIENTED_EDGE('',*,*,#20158,.T.);
#27074=ORIENTED_EDGE('',*,*,#20144,.T.);
#27075=ORIENTED_EDGE('',*,*,#20159,.T.);
#27076=ORIENTED_EDGE('',*,*,#18091,.T.);
#27077=ORIENTED_EDGE('',*,*,#20160,.T.);
#27078=ORIENTED_EDGE('',*,*,#20143,.T.);
#27079=ORIENTED_EDGE('',*,*,#20161,.T.);
#27080=ORIENTED_EDGE('',*,*,#20141,.T.);
#27081=ORIENTED_EDGE('',*,*,#20162,.T.);
#27082=ORIENTED_EDGE('',*,*,#20140,.T.);
#27083=ORIENTED_EDGE('',*,*,#20163,.T.);
#27084=ORIENTED_EDGE('',*,*,#18089,.T.);
#27085=ORIENTED_EDGE('',*,*,#20164,.T.);
#27086=ORIENTED_EDGE('',*,*,#20138,.T.);
#27087=ORIENTED_EDGE('',*,*,#20165,.T.);
#27088=ORIENTED_EDGE('',*,*,#20153,.F.);
#27089=ORIENTED_EDGE('',*,*,#20157,.F.);
#27090=ORIENTED_EDGE('',*,*,#20147,.F.);
#27091=ORIENTED_EDGE('',*,*,#18086,.F.);
#27092=ORIENTED_EDGE('',*,*,#20148,.F.);
#27093=ORIENTED_EDGE('',*,*,#20158,.F.);
#27094=ORIENTED_EDGE('',*,*,#20164,.F.);
#27095=ORIENTED_EDGE('',*,*,#18088,.F.);
#27096=ORIENTED_EDGE('',*,*,#20154,.F.);
#27097=ORIENTED_EDGE('',*,*,#20163,.F.);
#27098=ORIENTED_EDGE('',*,*,#20159,.F.);
#27099=ORIENTED_EDGE('',*,*,#20156,.F.);
#27100=ORIENTED_EDGE('',*,*,#20166,.T.);
#27101=ORIENTED_EDGE('',*,*,#20167,.T.);
#27102=ORIENTED_EDGE('',*,*,#20168,.T.);
#27103=ORIENTED_EDGE('',*,*,#20169,.T.);
#27104=ORIENTED_EDGE('',*,*,#20170,.T.);
#27105=ORIENTED_EDGE('',*,*,#20168,.F.);
#27106=ORIENTED_EDGE('',*,*,#20169,.F.);
#27107=ORIENTED_EDGE('',*,*,#20170,.F.);
#27108=ORIENTED_EDGE('',*,*,#20171,.T.);
#27109=ORIENTED_EDGE('',*,*,#20172,.F.);
#27110=ORIENTED_EDGE('',*,*,#20173,.F.);
#27111=ORIENTED_EDGE('',*,*,#20171,.F.);
#27112=ORIENTED_EDGE('',*,*,#17518,.F.);
#27113=ORIENTED_EDGE('',*,*,#20174,.T.);
#27114=ORIENTED_EDGE('',*,*,#20166,.F.);
#27115=ORIENTED_EDGE('',*,*,#20167,.F.);
#27116=ORIENTED_EDGE('',*,*,#20174,.F.);
#27117=ORIENTED_EDGE('',*,*,#20175,.T.);
#27118=ORIENTED_EDGE('',*,*,#20176,.T.);
#27119=ORIENTED_EDGE('',*,*,#20106,.T.);
#27120=ORIENTED_EDGE('',*,*,#20107,.T.);
#27121=ORIENTED_EDGE('',*,*,#20176,.F.);
#27122=ORIENTED_EDGE('',*,*,#20177,.F.);
#27123=ORIENTED_EDGE('',*,*,#20175,.F.);
#27124=ORIENTED_EDGE('',*,*,#20178,.T.);
#27125=ORIENTED_EDGE('',*,*,#20179,.T.);
#27126=ORIENTED_EDGE('',*,*,#20172,.T.);
#27127=ORIENTED_EDGE('',*,*,#20173,.T.);
#27128=ORIENTED_EDGE('',*,*,#20179,.F.);
#27129=ORIENTED_EDGE('',*,*,#20178,.F.);
#27130=ORIENTED_EDGE('',*,*,#20180,.T.);
#27131=ORIENTED_EDGE('',*,*,#20181,.F.);
#27132=ORIENTED_EDGE('',*,*,#20180,.F.);
#27133=ORIENTED_EDGE('',*,*,#20181,.T.);
#27134=ORIENTED_EDGE('',*,*,#20182,.T.);
#27135=ORIENTED_EDGE('',*,*,#20177,.T.);
#27136=ORIENTED_EDGE('',*,*,#20182,.F.);
#27137=ORIENTED_EDGE('',*,*,#20152,.F.);
#27138=ORIENTED_EDGE('',*,*,#18084,.F.);
#27139=ORIENTED_EDGE('',*,*,#20161,.F.);
#27140=ORIENTED_EDGE('',*,*,#20155,.F.);
#27141=ORIENTED_EDGE('',*,*,#20160,.F.);
#27142=ORIENTED_EDGE('',*,*,#18090,.F.);
#27143=ORIENTED_EDGE('',*,*,#20165,.F.);
#27144=ORIENTED_EDGE('',*,*,#20162,.F.);
#27145=ORIENTED_EDGE('',*,*,#20124,.F.);
#27146=ORIENTED_EDGE('',*,*,#18076,.F.);
#27147=ORIENTED_EDGE('',*,*,#20133,.F.);
#27148=ORIENTED_EDGE('',*,*,#20127,.F.);
#27149=ORIENTED_EDGE('',*,*,#20132,.F.);
#27150=ORIENTED_EDGE('',*,*,#18082,.F.);
#27151=ORIENTED_EDGE('',*,*,#20137,.F.);
#27152=ORIENTED_EDGE('',*,*,#20134,.F.);
#27153=ORIENTED_EDGE('',*,*,#20086,.F.);
#27154=ORIENTED_EDGE('',*,*,#18068,.F.);
#27155=ORIENTED_EDGE('',*,*,#20095,.F.);
#27156=ORIENTED_EDGE('',*,*,#20089,.F.);
#27157=ORIENTED_EDGE('',*,*,#20094,.F.);
#27158=ORIENTED_EDGE('',*,*,#18074,.F.);
#27159=ORIENTED_EDGE('',*,*,#20099,.F.);
#27160=ORIENTED_EDGE('',*,*,#20096,.F.);
#27161=ORIENTED_EDGE('',*,*,#20058,.F.);
#27162=ORIENTED_EDGE('',*,*,#18060,.F.);
#27163=ORIENTED_EDGE('',*,*,#20067,.F.);
#27164=ORIENTED_EDGE('',*,*,#20061,.F.);
#27165=ORIENTED_EDGE('',*,*,#20066,.F.);
#27166=ORIENTED_EDGE('',*,*,#18066,.F.);
#27167=ORIENTED_EDGE('',*,*,#20071,.F.);
#27168=ORIENTED_EDGE('',*,*,#20068,.F.);
#27169=ORIENTED_EDGE('',*,*,#20043,.F.);
#27170=ORIENTED_EDGE('',*,*,#18054,.F.);
#27171=ORIENTED_EDGE('',*,*,#20037,.F.);
#27172=ORIENTED_EDGE('',*,*,#20041,.F.);
#27173=ORIENTED_EDGE('',*,*,#20023,.F.);
#27174=ORIENTED_EDGE('',*,*,#18058,.F.);
#27175=ORIENTED_EDGE('',*,*,#20035,.F.);
#27176=ORIENTED_EDGE('',*,*,#20032,.F.);
#27177=ORIENTED_EDGE('',*,*,#20002,.F.);
#27178=ORIENTED_EDGE('',*,*,#18044,.F.);
#27179=ORIENTED_EDGE('',*,*,#20011,.F.);
#27180=ORIENTED_EDGE('',*,*,#20005,.F.);
#27181=ORIENTED_EDGE('',*,*,#20010,.F.);
#27182=ORIENTED_EDGE('',*,*,#18050,.F.);
#27183=ORIENTED_EDGE('',*,*,#20015,.F.);
#27184=ORIENTED_EDGE('',*,*,#20012,.F.);
#27185=ORIENTED_EDGE('',*,*,#19976,.F.);
#27186=ORIENTED_EDGE('',*,*,#18038,.F.);
#27187=ORIENTED_EDGE('',*,*,#19982,.F.);
#27188=ORIENTED_EDGE('',*,*,#19986,.F.);
#27189=ORIENTED_EDGE('',*,*,#19981,.F.);
#27190=ORIENTED_EDGE('',*,*,#18036,.F.);
#27191=ORIENTED_EDGE('',*,*,#19987,.F.);
#27192=ORIENTED_EDGE('',*,*,#19984,.F.);
#27193=ORIENTED_EDGE('',*,*,#19946,.F.);
#27194=ORIENTED_EDGE('',*,*,#18028,.F.);
#27195=ORIENTED_EDGE('',*,*,#19955,.F.);
#27196=ORIENTED_EDGE('',*,*,#19949,.F.);
#27197=ORIENTED_EDGE('',*,*,#19954,.F.);
#27198=ORIENTED_EDGE('',*,*,#18034,.F.);
#27199=ORIENTED_EDGE('',*,*,#19959,.F.);
#27200=ORIENTED_EDGE('',*,*,#19956,.F.);
#27201=ORIENTED_EDGE('',*,*,#19918,.F.);
#27202=ORIENTED_EDGE('',*,*,#18020,.F.);
#27203=ORIENTED_EDGE('',*,*,#19927,.F.);
#27204=ORIENTED_EDGE('',*,*,#19921,.F.);
#27205=ORIENTED_EDGE('',*,*,#19926,.F.);
#27206=ORIENTED_EDGE('',*,*,#18026,.F.);
#27207=ORIENTED_EDGE('',*,*,#19931,.F.);
#27208=ORIENTED_EDGE('',*,*,#19928,.F.);
#27209=ORIENTED_EDGE('',*,*,#19903,.F.);
#27210=ORIENTED_EDGE('',*,*,#18014,.F.);
#27211=ORIENTED_EDGE('',*,*,#19897,.F.);
#27212=ORIENTED_EDGE('',*,*,#19901,.F.);
#27213=ORIENTED_EDGE('',*,*,#19883,.F.);
#27214=ORIENTED_EDGE('',*,*,#18018,.F.);
#27215=ORIENTED_EDGE('',*,*,#19895,.F.);
#27216=ORIENTED_EDGE('',*,*,#19892,.F.);
#27217=ORIENTED_EDGE('',*,*,#19862,.F.);
#27218=ORIENTED_EDGE('',*,*,#18004,.F.);
#27219=ORIENTED_EDGE('',*,*,#19871,.F.);
#27220=ORIENTED_EDGE('',*,*,#19865,.F.);
#27221=ORIENTED_EDGE('',*,*,#19870,.F.);
#27222=ORIENTED_EDGE('',*,*,#18010,.F.);
#27223=ORIENTED_EDGE('',*,*,#19875,.F.);
#27224=ORIENTED_EDGE('',*,*,#19872,.F.);
#27225=ORIENTED_EDGE('',*,*,#19836,.F.);
#27226=ORIENTED_EDGE('',*,*,#17998,.F.);
#27227=ORIENTED_EDGE('',*,*,#19842,.F.);
#27228=ORIENTED_EDGE('',*,*,#19846,.F.);
#27229=ORIENTED_EDGE('',*,*,#19841,.F.);
#27230=ORIENTED_EDGE('',*,*,#17996,.F.);
#27231=ORIENTED_EDGE('',*,*,#19847,.F.);
#27232=ORIENTED_EDGE('',*,*,#19844,.F.);
#27233=ORIENTED_EDGE('',*,*,#19806,.F.);
#27234=ORIENTED_EDGE('',*,*,#17988,.F.);
#27235=ORIENTED_EDGE('',*,*,#19815,.F.);
#27236=ORIENTED_EDGE('',*,*,#19809,.F.);
#27237=ORIENTED_EDGE('',*,*,#19814,.F.);
#27238=ORIENTED_EDGE('',*,*,#17994,.F.);
#27239=ORIENTED_EDGE('',*,*,#19819,.F.);
#27240=ORIENTED_EDGE('',*,*,#19816,.F.);
#27241=ORIENTED_EDGE('',*,*,#19778,.F.);
#27242=ORIENTED_EDGE('',*,*,#17980,.F.);
#27243=ORIENTED_EDGE('',*,*,#19787,.F.);
#27244=ORIENTED_EDGE('',*,*,#19781,.F.);
#27245=ORIENTED_EDGE('',*,*,#19786,.F.);
#27246=ORIENTED_EDGE('',*,*,#17986,.F.);
#27247=ORIENTED_EDGE('',*,*,#19791,.F.);
#27248=ORIENTED_EDGE('',*,*,#19788,.F.);
#27249=ORIENTED_EDGE('',*,*,#19763,.F.);
#27250=ORIENTED_EDGE('',*,*,#17974,.F.);
#27251=ORIENTED_EDGE('',*,*,#19757,.F.);
#27252=ORIENTED_EDGE('',*,*,#19761,.F.);
#27253=ORIENTED_EDGE('',*,*,#19743,.F.);
#27254=ORIENTED_EDGE('',*,*,#17978,.F.);
#27255=ORIENTED_EDGE('',*,*,#19755,.F.);
#27256=ORIENTED_EDGE('',*,*,#19752,.F.);
#27257=ORIENTED_EDGE('',*,*,#19722,.F.);
#27258=ORIENTED_EDGE('',*,*,#17964,.F.);
#27259=ORIENTED_EDGE('',*,*,#19731,.F.);
#27260=ORIENTED_EDGE('',*,*,#19725,.F.);
#27261=ORIENTED_EDGE('',*,*,#19730,.F.);
#27262=ORIENTED_EDGE('',*,*,#17970,.F.);
#27263=ORIENTED_EDGE('',*,*,#19735,.F.);
#27264=ORIENTED_EDGE('',*,*,#19732,.F.);
#27265=ORIENTED_EDGE('',*,*,#19696,.F.);
#27266=ORIENTED_EDGE('',*,*,#17958,.F.);
#27267=ORIENTED_EDGE('',*,*,#19702,.F.);
#27268=ORIENTED_EDGE('',*,*,#19706,.F.);
#27269=ORIENTED_EDGE('',*,*,#19701,.F.);
#27270=ORIENTED_EDGE('',*,*,#17956,.F.);
#27271=ORIENTED_EDGE('',*,*,#19707,.F.);
#27272=ORIENTED_EDGE('',*,*,#19704,.F.);
#27273=ORIENTED_EDGE('',*,*,#19666,.F.);
#27274=ORIENTED_EDGE('',*,*,#17948,.F.);
#27275=ORIENTED_EDGE('',*,*,#19675,.F.);
#27276=ORIENTED_EDGE('',*,*,#19669,.F.);
#27277=ORIENTED_EDGE('',*,*,#19674,.F.);
#27278=ORIENTED_EDGE('',*,*,#17954,.F.);
#27279=ORIENTED_EDGE('',*,*,#19679,.F.);
#27280=ORIENTED_EDGE('',*,*,#19676,.F.);
#27281=ORIENTED_EDGE('',*,*,#19638,.F.);
#27282=ORIENTED_EDGE('',*,*,#17940,.F.);
#27283=ORIENTED_EDGE('',*,*,#19647,.F.);
#27284=ORIENTED_EDGE('',*,*,#19641,.F.);
#27285=ORIENTED_EDGE('',*,*,#19646,.F.);
#27286=ORIENTED_EDGE('',*,*,#17946,.F.);
#27287=ORIENTED_EDGE('',*,*,#19651,.F.);
#27288=ORIENTED_EDGE('',*,*,#19648,.F.);
#27289=ORIENTED_EDGE('',*,*,#19623,.F.);
#27290=ORIENTED_EDGE('',*,*,#17934,.F.);
#27291=ORIENTED_EDGE('',*,*,#19617,.F.);
#27292=ORIENTED_EDGE('',*,*,#19621,.F.);
#27293=ORIENTED_EDGE('',*,*,#19603,.F.);
#27294=ORIENTED_EDGE('',*,*,#17938,.F.);
#27295=ORIENTED_EDGE('',*,*,#19615,.F.);
#27296=ORIENTED_EDGE('',*,*,#19612,.F.);
#27297=ORIENTED_EDGE('',*,*,#19582,.F.);
#27298=ORIENTED_EDGE('',*,*,#17924,.F.);
#27299=ORIENTED_EDGE('',*,*,#19591,.F.);
#27300=ORIENTED_EDGE('',*,*,#19585,.F.);
#27301=ORIENTED_EDGE('',*,*,#19590,.F.);
#27302=ORIENTED_EDGE('',*,*,#17930,.F.);
#27303=ORIENTED_EDGE('',*,*,#19595,.F.);
#27304=ORIENTED_EDGE('',*,*,#19592,.F.);
#27305=ORIENTED_EDGE('',*,*,#19556,.F.);
#27306=ORIENTED_EDGE('',*,*,#17918,.F.);
#27307=ORIENTED_EDGE('',*,*,#19562,.F.);
#27308=ORIENTED_EDGE('',*,*,#19566,.F.);
#27309=ORIENTED_EDGE('',*,*,#19561,.F.);
#27310=ORIENTED_EDGE('',*,*,#17916,.F.);
#27311=ORIENTED_EDGE('',*,*,#19567,.F.);
#27312=ORIENTED_EDGE('',*,*,#19564,.F.);
#27313=ORIENTED_EDGE('',*,*,#19526,.F.);
#27314=ORIENTED_EDGE('',*,*,#17908,.F.);
#27315=ORIENTED_EDGE('',*,*,#19535,.F.);
#27316=ORIENTED_EDGE('',*,*,#19529,.F.);
#27317=ORIENTED_EDGE('',*,*,#19534,.F.);
#27318=ORIENTED_EDGE('',*,*,#17914,.F.);
#27319=ORIENTED_EDGE('',*,*,#19539,.F.);
#27320=ORIENTED_EDGE('',*,*,#19536,.F.);
#27321=ORIENTED_EDGE('',*,*,#19498,.F.);
#27322=ORIENTED_EDGE('',*,*,#17900,.F.);
#27323=ORIENTED_EDGE('',*,*,#19507,.F.);
#27324=ORIENTED_EDGE('',*,*,#19501,.F.);
#27325=ORIENTED_EDGE('',*,*,#19506,.F.);
#27326=ORIENTED_EDGE('',*,*,#17906,.F.);
#27327=ORIENTED_EDGE('',*,*,#19511,.F.);
#27328=ORIENTED_EDGE('',*,*,#19508,.F.);
#27329=ORIENTED_EDGE('',*,*,#19483,.F.);
#27330=ORIENTED_EDGE('',*,*,#17894,.F.);
#27331=ORIENTED_EDGE('',*,*,#19477,.F.);
#27332=ORIENTED_EDGE('',*,*,#19481,.F.);
#27333=ORIENTED_EDGE('',*,*,#19463,.F.);
#27334=ORIENTED_EDGE('',*,*,#17898,.F.);
#27335=ORIENTED_EDGE('',*,*,#19475,.F.);
#27336=ORIENTED_EDGE('',*,*,#19472,.F.);
#27337=ORIENTED_EDGE('',*,*,#19442,.F.);
#27338=ORIENTED_EDGE('',*,*,#17884,.F.);
#27339=ORIENTED_EDGE('',*,*,#19451,.F.);
#27340=ORIENTED_EDGE('',*,*,#19445,.F.);
#27341=ORIENTED_EDGE('',*,*,#19450,.F.);
#27342=ORIENTED_EDGE('',*,*,#17890,.F.);
#27343=ORIENTED_EDGE('',*,*,#19455,.F.);
#27344=ORIENTED_EDGE('',*,*,#19452,.F.);
#27345=ORIENTED_EDGE('',*,*,#19416,.F.);
#27346=ORIENTED_EDGE('',*,*,#17878,.F.);
#27347=ORIENTED_EDGE('',*,*,#19422,.F.);
#27348=ORIENTED_EDGE('',*,*,#19426,.F.);
#27349=ORIENTED_EDGE('',*,*,#19421,.F.);
#27350=ORIENTED_EDGE('',*,*,#17876,.F.);
#27351=ORIENTED_EDGE('',*,*,#19427,.F.);
#27352=ORIENTED_EDGE('',*,*,#19424,.F.);
#27353=ORIENTED_EDGE('',*,*,#19386,.F.);
#27354=ORIENTED_EDGE('',*,*,#17868,.F.);
#27355=ORIENTED_EDGE('',*,*,#19395,.F.);
#27356=ORIENTED_EDGE('',*,*,#19389,.F.);
#27357=ORIENTED_EDGE('',*,*,#19394,.F.);
#27358=ORIENTED_EDGE('',*,*,#17874,.F.);
#27359=ORIENTED_EDGE('',*,*,#19399,.F.);
#27360=ORIENTED_EDGE('',*,*,#19396,.F.);
#27361=ORIENTED_EDGE('',*,*,#19358,.F.);
#27362=ORIENTED_EDGE('',*,*,#17860,.F.);
#27363=ORIENTED_EDGE('',*,*,#19367,.F.);
#27364=ORIENTED_EDGE('',*,*,#19361,.F.);
#27365=ORIENTED_EDGE('',*,*,#19366,.F.);
#27366=ORIENTED_EDGE('',*,*,#17866,.F.);
#27367=ORIENTED_EDGE('',*,*,#19371,.F.);
#27368=ORIENTED_EDGE('',*,*,#19368,.F.);
#27369=ORIENTED_EDGE('',*,*,#19343,.F.);
#27370=ORIENTED_EDGE('',*,*,#17854,.F.);
#27371=ORIENTED_EDGE('',*,*,#19337,.F.);
#27372=ORIENTED_EDGE('',*,*,#19341,.F.);
#27373=ORIENTED_EDGE('',*,*,#19323,.F.);
#27374=ORIENTED_EDGE('',*,*,#17858,.F.);
#27375=ORIENTED_EDGE('',*,*,#19335,.F.);
#27376=ORIENTED_EDGE('',*,*,#19332,.F.);
#27377=ORIENTED_EDGE('',*,*,#19302,.F.);
#27378=ORIENTED_EDGE('',*,*,#17844,.F.);
#27379=ORIENTED_EDGE('',*,*,#19311,.F.);
#27380=ORIENTED_EDGE('',*,*,#19305,.F.);
#27381=ORIENTED_EDGE('',*,*,#19310,.F.);
#27382=ORIENTED_EDGE('',*,*,#17850,.F.);
#27383=ORIENTED_EDGE('',*,*,#19315,.F.);
#27384=ORIENTED_EDGE('',*,*,#19312,.F.);
#27385=ORIENTED_EDGE('',*,*,#19276,.F.);
#27386=ORIENTED_EDGE('',*,*,#17838,.F.);
#27387=ORIENTED_EDGE('',*,*,#19282,.F.);
#27388=ORIENTED_EDGE('',*,*,#19286,.F.);
#27389=ORIENTED_EDGE('',*,*,#19281,.F.);
#27390=ORIENTED_EDGE('',*,*,#17836,.F.);
#27391=ORIENTED_EDGE('',*,*,#19287,.F.);
#27392=ORIENTED_EDGE('',*,*,#19284,.F.);
#27393=ORIENTED_EDGE('',*,*,#19246,.F.);
#27394=ORIENTED_EDGE('',*,*,#17828,.F.);
#27395=ORIENTED_EDGE('',*,*,#19255,.F.);
#27396=ORIENTED_EDGE('',*,*,#19249,.F.);
#27397=ORIENTED_EDGE('',*,*,#19254,.F.);
#27398=ORIENTED_EDGE('',*,*,#17834,.F.);
#27399=ORIENTED_EDGE('',*,*,#19259,.F.);
#27400=ORIENTED_EDGE('',*,*,#19256,.F.);
#27401=ORIENTED_EDGE('',*,*,#19218,.F.);
#27402=ORIENTED_EDGE('',*,*,#17820,.F.);
#27403=ORIENTED_EDGE('',*,*,#19227,.F.);
#27404=ORIENTED_EDGE('',*,*,#19221,.F.);
#27405=ORIENTED_EDGE('',*,*,#19226,.F.);
#27406=ORIENTED_EDGE('',*,*,#17826,.F.);
#27407=ORIENTED_EDGE('',*,*,#19231,.F.);
#27408=ORIENTED_EDGE('',*,*,#19228,.F.);
#27409=ORIENTED_EDGE('',*,*,#19203,.F.);
#27410=ORIENTED_EDGE('',*,*,#17814,.F.);
#27411=ORIENTED_EDGE('',*,*,#19197,.F.);
#27412=ORIENTED_EDGE('',*,*,#19201,.F.);
#27413=ORIENTED_EDGE('',*,*,#19183,.F.);
#27414=ORIENTED_EDGE('',*,*,#17818,.F.);
#27415=ORIENTED_EDGE('',*,*,#19195,.F.);
#27416=ORIENTED_EDGE('',*,*,#19192,.F.);
#27417=ORIENTED_EDGE('',*,*,#19162,.F.);
#27418=ORIENTED_EDGE('',*,*,#17804,.F.);
#27419=ORIENTED_EDGE('',*,*,#19171,.F.);
#27420=ORIENTED_EDGE('',*,*,#19165,.F.);
#27421=ORIENTED_EDGE('',*,*,#19170,.F.);
#27422=ORIENTED_EDGE('',*,*,#17810,.F.);
#27423=ORIENTED_EDGE('',*,*,#19175,.F.);
#27424=ORIENTED_EDGE('',*,*,#19172,.F.);
#27425=ORIENTED_EDGE('',*,*,#19136,.F.);
#27426=ORIENTED_EDGE('',*,*,#17798,.F.);
#27427=ORIENTED_EDGE('',*,*,#19142,.F.);
#27428=ORIENTED_EDGE('',*,*,#19146,.F.);
#27429=ORIENTED_EDGE('',*,*,#19141,.F.);
#27430=ORIENTED_EDGE('',*,*,#17796,.F.);
#27431=ORIENTED_EDGE('',*,*,#19147,.F.);
#27432=ORIENTED_EDGE('',*,*,#19144,.F.);
#27433=ORIENTED_EDGE('',*,*,#19106,.F.);
#27434=ORIENTED_EDGE('',*,*,#17788,.F.);
#27435=ORIENTED_EDGE('',*,*,#19115,.F.);
#27436=ORIENTED_EDGE('',*,*,#19109,.F.);
#27437=ORIENTED_EDGE('',*,*,#19114,.F.);
#27438=ORIENTED_EDGE('',*,*,#17794,.F.);
#27439=ORIENTED_EDGE('',*,*,#19119,.F.);
#27440=ORIENTED_EDGE('',*,*,#19116,.F.);
#27441=ORIENTED_EDGE('',*,*,#19078,.F.);
#27442=ORIENTED_EDGE('',*,*,#17780,.F.);
#27443=ORIENTED_EDGE('',*,*,#19087,.F.);
#27444=ORIENTED_EDGE('',*,*,#19081,.F.);
#27445=ORIENTED_EDGE('',*,*,#19086,.F.);
#27446=ORIENTED_EDGE('',*,*,#17786,.F.);
#27447=ORIENTED_EDGE('',*,*,#19091,.F.);
#27448=ORIENTED_EDGE('',*,*,#19088,.F.);
#27449=ORIENTED_EDGE('',*,*,#19063,.F.);
#27450=ORIENTED_EDGE('',*,*,#17774,.F.);
#27451=ORIENTED_EDGE('',*,*,#19057,.F.);
#27452=ORIENTED_EDGE('',*,*,#19061,.F.);
#27453=ORIENTED_EDGE('',*,*,#19043,.F.);
#27454=ORIENTED_EDGE('',*,*,#17778,.F.);
#27455=ORIENTED_EDGE('',*,*,#19055,.F.);
#27456=ORIENTED_EDGE('',*,*,#19052,.F.);
#27457=ORIENTED_EDGE('',*,*,#19022,.F.);
#27458=ORIENTED_EDGE('',*,*,#17764,.F.);
#27459=ORIENTED_EDGE('',*,*,#19031,.F.);
#27460=ORIENTED_EDGE('',*,*,#19025,.F.);
#27461=ORIENTED_EDGE('',*,*,#19030,.F.);
#27462=ORIENTED_EDGE('',*,*,#17770,.F.);
#27463=ORIENTED_EDGE('',*,*,#19035,.F.);
#27464=ORIENTED_EDGE('',*,*,#19032,.F.);
#27465=ORIENTED_EDGE('',*,*,#18996,.F.);
#27466=ORIENTED_EDGE('',*,*,#17758,.F.);
#27467=ORIENTED_EDGE('',*,*,#19002,.F.);
#27468=ORIENTED_EDGE('',*,*,#19006,.F.);
#27469=ORIENTED_EDGE('',*,*,#19001,.F.);
#27470=ORIENTED_EDGE('',*,*,#17756,.F.);
#27471=ORIENTED_EDGE('',*,*,#19007,.F.);
#27472=ORIENTED_EDGE('',*,*,#19004,.F.);
#27473=ORIENTED_EDGE('',*,*,#18966,.F.);
#27474=ORIENTED_EDGE('',*,*,#17748,.F.);
#27475=ORIENTED_EDGE('',*,*,#18975,.F.);
#27476=ORIENTED_EDGE('',*,*,#18969,.F.);
#27477=ORIENTED_EDGE('',*,*,#18974,.F.);
#27478=ORIENTED_EDGE('',*,*,#17754,.F.);
#27479=ORIENTED_EDGE('',*,*,#18979,.F.);
#27480=ORIENTED_EDGE('',*,*,#18976,.F.);
#27481=ORIENTED_EDGE('',*,*,#18938,.F.);
#27482=ORIENTED_EDGE('',*,*,#17740,.F.);
#27483=ORIENTED_EDGE('',*,*,#18947,.F.);
#27484=ORIENTED_EDGE('',*,*,#18941,.F.);
#27485=ORIENTED_EDGE('',*,*,#18946,.F.);
#27486=ORIENTED_EDGE('',*,*,#17746,.F.);
#27487=ORIENTED_EDGE('',*,*,#18951,.F.);
#27488=ORIENTED_EDGE('',*,*,#18948,.F.);
#27489=ORIENTED_EDGE('',*,*,#18923,.F.);
#27490=ORIENTED_EDGE('',*,*,#17734,.F.);
#27491=ORIENTED_EDGE('',*,*,#18917,.F.);
#27492=ORIENTED_EDGE('',*,*,#18921,.F.);
#27493=ORIENTED_EDGE('',*,*,#18903,.F.);
#27494=ORIENTED_EDGE('',*,*,#17738,.F.);
#27495=ORIENTED_EDGE('',*,*,#18915,.F.);
#27496=ORIENTED_EDGE('',*,*,#18912,.F.);
#27497=ORIENTED_EDGE('',*,*,#18882,.F.);
#27498=ORIENTED_EDGE('',*,*,#17724,.F.);
#27499=ORIENTED_EDGE('',*,*,#18891,.F.);
#27500=ORIENTED_EDGE('',*,*,#18885,.F.);
#27501=ORIENTED_EDGE('',*,*,#18890,.F.);
#27502=ORIENTED_EDGE('',*,*,#17730,.F.);
#27503=ORIENTED_EDGE('',*,*,#18895,.F.);
#27504=ORIENTED_EDGE('',*,*,#18892,.F.);
#27505=ORIENTED_EDGE('',*,*,#18856,.F.);
#27506=ORIENTED_EDGE('',*,*,#17718,.F.);
#27507=ORIENTED_EDGE('',*,*,#18862,.F.);
#27508=ORIENTED_EDGE('',*,*,#18866,.F.);
#27509=ORIENTED_EDGE('',*,*,#18861,.F.);
#27510=ORIENTED_EDGE('',*,*,#17716,.F.);
#27511=ORIENTED_EDGE('',*,*,#18867,.F.);
#27512=ORIENTED_EDGE('',*,*,#18864,.F.);
#27513=ORIENTED_EDGE('',*,*,#18826,.F.);
#27514=ORIENTED_EDGE('',*,*,#17708,.F.);
#27515=ORIENTED_EDGE('',*,*,#18835,.F.);
#27516=ORIENTED_EDGE('',*,*,#18829,.F.);
#27517=ORIENTED_EDGE('',*,*,#18834,.F.);
#27518=ORIENTED_EDGE('',*,*,#17714,.F.);
#27519=ORIENTED_EDGE('',*,*,#18839,.F.);
#27520=ORIENTED_EDGE('',*,*,#18836,.F.);
#27521=ORIENTED_EDGE('',*,*,#18798,.F.);
#27522=ORIENTED_EDGE('',*,*,#17700,.F.);
#27523=ORIENTED_EDGE('',*,*,#18807,.F.);
#27524=ORIENTED_EDGE('',*,*,#18801,.F.);
#27525=ORIENTED_EDGE('',*,*,#18806,.F.);
#27526=ORIENTED_EDGE('',*,*,#17706,.F.);
#27527=ORIENTED_EDGE('',*,*,#18811,.F.);
#27528=ORIENTED_EDGE('',*,*,#18808,.F.);
#27529=ORIENTED_EDGE('',*,*,#18783,.F.);
#27530=ORIENTED_EDGE('',*,*,#17694,.F.);
#27531=ORIENTED_EDGE('',*,*,#18777,.F.);
#27532=ORIENTED_EDGE('',*,*,#18781,.F.);
#27533=ORIENTED_EDGE('',*,*,#18763,.F.);
#27534=ORIENTED_EDGE('',*,*,#17698,.F.);
#27535=ORIENTED_EDGE('',*,*,#18775,.F.);
#27536=ORIENTED_EDGE('',*,*,#18772,.F.);
#27537=ORIENTED_EDGE('',*,*,#18742,.F.);
#27538=ORIENTED_EDGE('',*,*,#17684,.F.);
#27539=ORIENTED_EDGE('',*,*,#18751,.F.);
#27540=ORIENTED_EDGE('',*,*,#18745,.F.);
#27541=ORIENTED_EDGE('',*,*,#18750,.F.);
#27542=ORIENTED_EDGE('',*,*,#17690,.F.);
#27543=ORIENTED_EDGE('',*,*,#18755,.F.);
#27544=ORIENTED_EDGE('',*,*,#18752,.F.);
#27545=ORIENTED_EDGE('',*,*,#18716,.F.);
#27546=ORIENTED_EDGE('',*,*,#17678,.F.);
#27547=ORIENTED_EDGE('',*,*,#18722,.F.);
#27548=ORIENTED_EDGE('',*,*,#18726,.F.);
#27549=ORIENTED_EDGE('',*,*,#18721,.F.);
#27550=ORIENTED_EDGE('',*,*,#17676,.F.);
#27551=ORIENTED_EDGE('',*,*,#18727,.F.);
#27552=ORIENTED_EDGE('',*,*,#18724,.F.);
#27553=ORIENTED_EDGE('',*,*,#18686,.F.);
#27554=ORIENTED_EDGE('',*,*,#17668,.F.);
#27555=ORIENTED_EDGE('',*,*,#18695,.F.);
#27556=ORIENTED_EDGE('',*,*,#18689,.F.);
#27557=ORIENTED_EDGE('',*,*,#18694,.F.);
#27558=ORIENTED_EDGE('',*,*,#17674,.F.);
#27559=ORIENTED_EDGE('',*,*,#18699,.F.);
#27560=ORIENTED_EDGE('',*,*,#18696,.F.);
#27561=ORIENTED_EDGE('',*,*,#18658,.F.);
#27562=ORIENTED_EDGE('',*,*,#17514,.F.);
#27563=ORIENTED_EDGE('',*,*,#18667,.F.);
#27564=ORIENTED_EDGE('',*,*,#18661,.F.);
#27565=ORIENTED_EDGE('',*,*,#18666,.F.);
#27566=ORIENTED_EDGE('',*,*,#17512,.F.);
#27567=ORIENTED_EDGE('',*,*,#17523,.F.);
#27568=ORIENTED_EDGE('',*,*,#18671,.F.);
#27569=ORIENTED_EDGE('',*,*,#18668,.F.);
#27570=ORIENTED_EDGE('',*,*,#18643,.F.);
#27571=ORIENTED_EDGE('',*,*,#17662,.F.);
#27572=ORIENTED_EDGE('',*,*,#18637,.F.);
#27573=ORIENTED_EDGE('',*,*,#18641,.F.);
#27574=ORIENTED_EDGE('',*,*,#18623,.F.);
#27575=ORIENTED_EDGE('',*,*,#17666,.F.);
#27576=ORIENTED_EDGE('',*,*,#18635,.F.);
#27577=ORIENTED_EDGE('',*,*,#18632,.F.);
#27578=ORIENTED_EDGE('',*,*,#18602,.F.);
#27579=ORIENTED_EDGE('',*,*,#17652,.F.);
#27580=ORIENTED_EDGE('',*,*,#18611,.F.);
#27581=ORIENTED_EDGE('',*,*,#18605,.F.);
#27582=ORIENTED_EDGE('',*,*,#18610,.F.);
#27583=ORIENTED_EDGE('',*,*,#17658,.F.);
#27584=ORIENTED_EDGE('',*,*,#18615,.F.);
#27585=ORIENTED_EDGE('',*,*,#18612,.F.);
#27586=ORIENTED_EDGE('',*,*,#18576,.F.);
#27587=ORIENTED_EDGE('',*,*,#17646,.F.);
#27588=ORIENTED_EDGE('',*,*,#18582,.F.);
#27589=ORIENTED_EDGE('',*,*,#18586,.F.);
#27590=ORIENTED_EDGE('',*,*,#18581,.F.);
#27591=ORIENTED_EDGE('',*,*,#17644,.F.);
#27592=ORIENTED_EDGE('',*,*,#18587,.F.);
#27593=ORIENTED_EDGE('',*,*,#18584,.F.);
#27594=ORIENTED_EDGE('',*,*,#18546,.F.);
#27595=ORIENTED_EDGE('',*,*,#17636,.F.);
#27596=ORIENTED_EDGE('',*,*,#18555,.F.);
#27597=ORIENTED_EDGE('',*,*,#18549,.F.);
#27598=ORIENTED_EDGE('',*,*,#18554,.F.);
#27599=ORIENTED_EDGE('',*,*,#17642,.F.);
#27600=ORIENTED_EDGE('',*,*,#18559,.F.);
#27601=ORIENTED_EDGE('',*,*,#18556,.F.);
#27602=ORIENTED_EDGE('',*,*,#18518,.F.);
#27603=ORIENTED_EDGE('',*,*,#17628,.F.);
#27604=ORIENTED_EDGE('',*,*,#18527,.F.);
#27605=ORIENTED_EDGE('',*,*,#18521,.F.);
#27606=ORIENTED_EDGE('',*,*,#18526,.F.);
#27607=ORIENTED_EDGE('',*,*,#17634,.F.);
#27608=ORIENTED_EDGE('',*,*,#18531,.F.);
#27609=ORIENTED_EDGE('',*,*,#18528,.F.);
#27610=ORIENTED_EDGE('',*,*,#18503,.F.);
#27611=ORIENTED_EDGE('',*,*,#17622,.F.);
#27612=ORIENTED_EDGE('',*,*,#18497,.F.);
#27613=ORIENTED_EDGE('',*,*,#18501,.F.);
#27614=ORIENTED_EDGE('',*,*,#18483,.F.);
#27615=ORIENTED_EDGE('',*,*,#17626,.F.);
#27616=ORIENTED_EDGE('',*,*,#18495,.F.);
#27617=ORIENTED_EDGE('',*,*,#18492,.F.);
#27618=ORIENTED_EDGE('',*,*,#18462,.F.);
#27619=ORIENTED_EDGE('',*,*,#17612,.F.);
#27620=ORIENTED_EDGE('',*,*,#18471,.F.);
#27621=ORIENTED_EDGE('',*,*,#18465,.F.);
#27622=ORIENTED_EDGE('',*,*,#18470,.F.);
#27623=ORIENTED_EDGE('',*,*,#17618,.F.);
#27624=ORIENTED_EDGE('',*,*,#18475,.F.);
#27625=ORIENTED_EDGE('',*,*,#18472,.F.);
#27626=ORIENTED_EDGE('',*,*,#18436,.F.);
#27627=ORIENTED_EDGE('',*,*,#17606,.F.);
#27628=ORIENTED_EDGE('',*,*,#18442,.F.);
#27629=ORIENTED_EDGE('',*,*,#18446,.F.);
#27630=ORIENTED_EDGE('',*,*,#18441,.F.);
#27631=ORIENTED_EDGE('',*,*,#17604,.F.);
#27632=ORIENTED_EDGE('',*,*,#18447,.F.);
#27633=ORIENTED_EDGE('',*,*,#18444,.F.);
#27634=ORIENTED_EDGE('',*,*,#18406,.F.);
#27635=ORIENTED_EDGE('',*,*,#17596,.F.);
#27636=ORIENTED_EDGE('',*,*,#18415,.F.);
#27637=ORIENTED_EDGE('',*,*,#18409,.F.);
#27638=ORIENTED_EDGE('',*,*,#18414,.F.);
#27639=ORIENTED_EDGE('',*,*,#17602,.F.);
#27640=ORIENTED_EDGE('',*,*,#18419,.F.);
#27641=ORIENTED_EDGE('',*,*,#18416,.F.);
#27642=ORIENTED_EDGE('',*,*,#18378,.F.);
#27643=ORIENTED_EDGE('',*,*,#17588,.F.);
#27644=ORIENTED_EDGE('',*,*,#18387,.F.);
#27645=ORIENTED_EDGE('',*,*,#18381,.F.);
#27646=ORIENTED_EDGE('',*,*,#18386,.F.);
#27647=ORIENTED_EDGE('',*,*,#17594,.F.);
#27648=ORIENTED_EDGE('',*,*,#18391,.F.);
#27649=ORIENTED_EDGE('',*,*,#18388,.F.);
#27650=ORIENTED_EDGE('',*,*,#18363,.F.);
#27651=ORIENTED_EDGE('',*,*,#17582,.F.);
#27652=ORIENTED_EDGE('',*,*,#18357,.F.);
#27653=ORIENTED_EDGE('',*,*,#18361,.F.);
#27654=ORIENTED_EDGE('',*,*,#18343,.F.);
#27655=ORIENTED_EDGE('',*,*,#17586,.F.);
#27656=ORIENTED_EDGE('',*,*,#18355,.F.);
#27657=ORIENTED_EDGE('',*,*,#18352,.F.);
#27658=ORIENTED_EDGE('',*,*,#18322,.F.);
#27659=ORIENTED_EDGE('',*,*,#17572,.F.);
#27660=ORIENTED_EDGE('',*,*,#18331,.F.);
#27661=ORIENTED_EDGE('',*,*,#18325,.F.);
#27662=ORIENTED_EDGE('',*,*,#18330,.F.);
#27663=ORIENTED_EDGE('',*,*,#17578,.F.);
#27664=ORIENTED_EDGE('',*,*,#18335,.F.);
#27665=ORIENTED_EDGE('',*,*,#18332,.F.);
#27666=ORIENTED_EDGE('',*,*,#18296,.F.);
#27667=ORIENTED_EDGE('',*,*,#17566,.F.);
#27668=ORIENTED_EDGE('',*,*,#18302,.F.);
#27669=ORIENTED_EDGE('',*,*,#18306,.F.);
#27670=ORIENTED_EDGE('',*,*,#18301,.F.);
#27671=ORIENTED_EDGE('',*,*,#17564,.F.);
#27672=ORIENTED_EDGE('',*,*,#18307,.F.);
#27673=ORIENTED_EDGE('',*,*,#18304,.F.);
#27674=ORIENTED_EDGE('',*,*,#18266,.F.);
#27675=ORIENTED_EDGE('',*,*,#17556,.F.);
#27676=ORIENTED_EDGE('',*,*,#18275,.F.);
#27677=ORIENTED_EDGE('',*,*,#18269,.F.);
#27678=ORIENTED_EDGE('',*,*,#18274,.F.);
#27679=ORIENTED_EDGE('',*,*,#17562,.F.);
#27680=ORIENTED_EDGE('',*,*,#18279,.F.);
#27681=ORIENTED_EDGE('',*,*,#18276,.F.);
#27682=ORIENTED_EDGE('',*,*,#18238,.F.);
#27683=ORIENTED_EDGE('',*,*,#17548,.F.);
#27684=ORIENTED_EDGE('',*,*,#18247,.F.);
#27685=ORIENTED_EDGE('',*,*,#18241,.F.);
#27686=ORIENTED_EDGE('',*,*,#18246,.F.);
#27687=ORIENTED_EDGE('',*,*,#17554,.F.);
#27688=ORIENTED_EDGE('',*,*,#18251,.F.);
#27689=ORIENTED_EDGE('',*,*,#18248,.F.);
#27690=ORIENTED_EDGE('',*,*,#18223,.F.);
#27691=ORIENTED_EDGE('',*,*,#17542,.F.);
#27692=ORIENTED_EDGE('',*,*,#18217,.F.);
#27693=ORIENTED_EDGE('',*,*,#18221,.F.);
#27694=ORIENTED_EDGE('',*,*,#18203,.F.);
#27695=ORIENTED_EDGE('',*,*,#17546,.F.);
#27696=ORIENTED_EDGE('',*,*,#18215,.F.);
#27697=ORIENTED_EDGE('',*,*,#18212,.F.);
#27698=ORIENTED_EDGE('',*,*,#18182,.F.);
#27699=ORIENTED_EDGE('',*,*,#17532,.F.);
#27700=ORIENTED_EDGE('',*,*,#18191,.F.);
#27701=ORIENTED_EDGE('',*,*,#18185,.F.);
#27702=ORIENTED_EDGE('',*,*,#18190,.F.);
#27703=ORIENTED_EDGE('',*,*,#17538,.F.);
#27704=ORIENTED_EDGE('',*,*,#18195,.F.);
#27705=ORIENTED_EDGE('',*,*,#18192,.F.);
#27706=ORIENTED_EDGE('',*,*,#18156,.F.);
#27707=ORIENTED_EDGE('',*,*,#17526,.F.);
#27708=ORIENTED_EDGE('',*,*,#18162,.F.);
#27709=ORIENTED_EDGE('',*,*,#18166,.F.);
#27710=ORIENTED_EDGE('',*,*,#18161,.F.);
#27711=ORIENTED_EDGE('',*,*,#17524,.F.);
#27712=ORIENTED_EDGE('',*,*,#18167,.F.);
#27713=ORIENTED_EDGE('',*,*,#18164,.F.);
#27714=ORIENTED_EDGE('',*,*,#18135,.F.);
#27715=ORIENTED_EDGE('',*,*,#20183,.T.);
#27716=ORIENTED_EDGE('',*,*,#20184,.F.);
#27717=ORIENTED_EDGE('',*,*,#20183,.F.);
#27718=ORIENTED_EDGE('',*,*,#18136,.F.);
#27719=ORIENTED_EDGE('',*,*,#20185,.T.);
#27720=ORIENTED_EDGE('',*,*,#20186,.F.);
#27721=ORIENTED_EDGE('',*,*,#20185,.F.);
#27722=ORIENTED_EDGE('',*,*,#18137,.F.);
#27723=ORIENTED_EDGE('',*,*,#20187,.T.);
#27724=ORIENTED_EDGE('',*,*,#20188,.F.);
#27725=ORIENTED_EDGE('',*,*,#20187,.F.);
#27726=ORIENTED_EDGE('',*,*,#18138,.F.);
#27727=ORIENTED_EDGE('',*,*,#20189,.T.);
#27728=ORIENTED_EDGE('',*,*,#20190,.F.);
#27729=ORIENTED_EDGE('',*,*,#20189,.F.);
#27730=ORIENTED_EDGE('',*,*,#18139,.F.);
#27731=ORIENTED_EDGE('',*,*,#20191,.T.);
#27732=ORIENTED_EDGE('',*,*,#20192,.F.);
#27733=ORIENTED_EDGE('',*,*,#20191,.F.);
#27734=ORIENTED_EDGE('',*,*,#20193,.F.);
#27735=ORIENTED_EDGE('',*,*,#20194,.T.);
#27736=ORIENTED_EDGE('',*,*,#20195,.T.);
#27737=ORIENTED_EDGE('',*,*,#20194,.F.);
#27738=ORIENTED_EDGE('',*,*,#20195,.F.);
#27739=ORIENTED_EDGE('',*,*,#20196,.T.);
#27740=ORIENTED_EDGE('',*,*,#20197,.F.);
#27741=ORIENTED_EDGE('',*,*,#20196,.F.);
#27742=ORIENTED_EDGE('',*,*,#18098,.F.);
#27743=ORIENTED_EDGE('',*,*,#20198,.F.);
#27744=ORIENTED_EDGE('',*,*,#20199,.F.);
#27745=ORIENTED_EDGE('',*,*,#18133,.T.);
#27746=ORIENTED_EDGE('',*,*,#18101,.F.);
#27747=ORIENTED_EDGE('',*,*,#20200,.F.);
#27748=ORIENTED_EDGE('',*,*,#20201,.F.);
#27749=ORIENTED_EDGE('',*,*,#20198,.T.);
#27750=ORIENTED_EDGE('',*,*,#18104,.F.);
#27751=ORIENTED_EDGE('',*,*,#20202,.F.);
#27752=ORIENTED_EDGE('',*,*,#20203,.F.);
#27753=ORIENTED_EDGE('',*,*,#20200,.T.);
#27754=ORIENTED_EDGE('',*,*,#18107,.F.);
#27755=ORIENTED_EDGE('',*,*,#18124,.F.);
#27756=ORIENTED_EDGE('',*,*,#20204,.F.);
#27757=ORIENTED_EDGE('',*,*,#20202,.T.);
#27758=ORIENTED_EDGE('',*,*,#17494,.T.);
#27759=ORIENTED_EDGE('',*,*,#18126,.T.);
#27760=ORIENTED_EDGE('',*,*,#18128,.T.);
#27761=ORIENTED_EDGE('',*,*,#18130,.T.);
#27762=ORIENTED_EDGE('',*,*,#18132,.T.);
#27763=ORIENTED_EDGE('',*,*,#18134,.T.);
#27764=ORIENTED_EDGE('',*,*,#20199,.T.);
#27765=ORIENTED_EDGE('',*,*,#20201,.T.);
#27766=ORIENTED_EDGE('',*,*,#20203,.T.);
#27767=ORIENTED_EDGE('',*,*,#20204,.T.);
#27768=ORIENTED_EDGE('',*,*,#18123,.T.);
#27769=ORIENTED_EDGE('',*,*,#17480,.T.);
#27770=ORIENTED_EDGE('',*,*,#20205,.T.);
#27771=ORIENTED_EDGE('',*,*,#20206,.F.);
#27772=ORIENTED_EDGE('',*,*,#20205,.F.);
#27773=ORIENTED_EDGE('',*,*,#20206,.T.);
#27774=ORIENTED_EDGE('',*,*,#20197,.T.);
#27775=ORIENTED_EDGE('',*,*,#20193,.T.);
#27776=ORIENTED_EDGE('',*,*,#20207,.T.);
#27777=ORIENTED_EDGE('',*,*,#20208,.F.);
#27778=ORIENTED_EDGE('',*,*,#20207,.F.);
#27779=ORIENTED_EDGE('',*,*,#20208,.T.);
#27780=ORIENTED_EDGE('',*,*,#17470,.F.);
#27781=ORIENTED_EDGE('',*,*,#17472,.T.);
#27782=ORIENTED_EDGE('',*,*,#20209,.T.);
#27783=ORIENTED_EDGE('',*,*,#20210,.F.);
#27784=ORIENTED_EDGE('',*,*,#20209,.F.);
#27785=ORIENTED_EDGE('',*,*,#20211,.F.);
#27786=ORIENTED_EDGE('',*,*,#20210,.T.);
#27787=ORIENTED_EDGE('',*,*,#20211,.T.);
#27788=ORIENTED_EDGE('',*,*,#20212,.T.);
#27789=ORIENTED_EDGE('',*,*,#20213,.F.);
#27790=ORIENTED_EDGE('',*,*,#20212,.F.);
#27791=ORIENTED_EDGE('',*,*,#20213,.T.);
#27792=ORIENTED_EDGE('',*,*,#20214,.T.);
#27793=ORIENTED_EDGE('',*,*,#17465,.F.);
#27794=ORIENTED_EDGE('',*,*,#20214,.F.);
#27795=ORIENTED_EDGE('',*,*,#20215,.F.);
#27796=ORIENTED_EDGE('',*,*,#20216,.T.);
#27797=ORIENTED_EDGE('',*,*,#17461,.T.);
#27798=ORIENTED_EDGE('',*,*,#20216,.F.);
#27799=ORIENTED_EDGE('',*,*,#20217,.F.);
#27800=ORIENTED_EDGE('',*,*,#20215,.T.);
#27801=ORIENTED_EDGE('',*,*,#20192,.T.);
#27802=ORIENTED_EDGE('',*,*,#20190,.T.);
#27803=ORIENTED_EDGE('',*,*,#20188,.T.);
#27804=ORIENTED_EDGE('',*,*,#20186,.T.);
#27805=ORIENTED_EDGE('',*,*,#20184,.T.);
#27806=ORIENTED_EDGE('',*,*,#20217,.T.);
#27807=ORIENTED_EDGE('',*,*,#20218,.T.);
#27808=ORIENTED_EDGE('',*,*,#20219,.F.);
#27809=ORIENTED_EDGE('',*,*,#20218,.F.);
#27810=ORIENTED_EDGE('',*,*,#20219,.T.);
#27811=ORIENTED_EDGE('',*,*,#20220,.T.);
#27812=ORIENTED_EDGE('',*,*,#20108,.F.);
#27813=ORIENTED_EDGE('',*,*,#20220,.F.);
#27814=ORIENTED_EDGE('',*,*,#20221,.F.);
#27815=ORIENTED_EDGE('',*,*,#20222,.T.);
#27816=ORIENTED_EDGE('',*,*,#20223,.F.);
#27817=ORIENTED_EDGE('',*,*,#20224,.F.);
#27818=ORIENTED_EDGE('',*,*,#20225,.F.);
#27819=ORIENTED_EDGE('',*,*,#20226,.F.);
#27820=ORIENTED_EDGE('',*,*,#20227,.F.);
#27821=ORIENTED_EDGE('',*,*,#20228,.F.);
#27822=ORIENTED_EDGE('',*,*,#20229,.T.);
#27823=ORIENTED_EDGE('',*,*,#20221,.T.);
#27824=ORIENTED_EDGE('',*,*,#20230,.F.);
#27825=ORIENTED_EDGE('',*,*,#20231,.F.);
#27826=ORIENTED_EDGE('',*,*,#20232,.T.);
#27827=ORIENTED_EDGE('',*,*,#20228,.T.);
#27828=ORIENTED_EDGE('',*,*,#20233,.F.);
#27829=ORIENTED_EDGE('',*,*,#20234,.F.);
#27830=ORIENTED_EDGE('',*,*,#20235,.T.);
#27831=ORIENTED_EDGE('',*,*,#20231,.T.);
#27832=ORIENTED_EDGE('',*,*,#20236,.F.);
#27833=ORIENTED_EDGE('',*,*,#20237,.F.);
#27834=ORIENTED_EDGE('',*,*,#20238,.T.);
#27835=ORIENTED_EDGE('',*,*,#20234,.T.);
#27836=ORIENTED_EDGE('',*,*,#20239,.F.);
#27837=ORIENTED_EDGE('',*,*,#20240,.F.);
#27838=ORIENTED_EDGE('',*,*,#20241,.T.);
#27839=ORIENTED_EDGE('',*,*,#20237,.T.);
#27840=ORIENTED_EDGE('',*,*,#20242,.F.);
#27841=ORIENTED_EDGE('',*,*,#20243,.F.);
#27842=ORIENTED_EDGE('',*,*,#20244,.T.);
#27843=ORIENTED_EDGE('',*,*,#20245,.F.);
#27844=ORIENTED_EDGE('',*,*,#20246,.F.);
#27845=ORIENTED_EDGE('',*,*,#20247,.F.);
#27846=ORIENTED_EDGE('',*,*,#20248,.T.);
#27847=ORIENTED_EDGE('',*,*,#20243,.T.);
#27848=ORIENTED_EDGE('',*,*,#20249,.F.);
#27849=ORIENTED_EDGE('',*,*,#20250,.F.);
#27850=ORIENTED_EDGE('',*,*,#20251,.T.);
#27851=ORIENTED_EDGE('',*,*,#20247,.T.);
#27852=ORIENTED_EDGE('',*,*,#20252,.F.);
#27853=ORIENTED_EDGE('',*,*,#20253,.T.);
#27854=ORIENTED_EDGE('',*,*,#20254,.T.);
#27855=ORIENTED_EDGE('',*,*,#20255,.T.);
#27856=ORIENTED_EDGE('',*,*,#20254,.F.);
#27857=ORIENTED_EDGE('',*,*,#20256,.T.);
#27858=ORIENTED_EDGE('',*,*,#20255,.F.);
#27859=ORIENTED_EDGE('',*,*,#20256,.F.);
#27860=ORIENTED_EDGE('',*,*,#20257,.T.);
#27861=ORIENTED_EDGE('',*,*,#20253,.F.);
#27862=ORIENTED_EDGE('',*,*,#20258,.T.);
#27863=ORIENTED_EDGE('',*,*,#20259,.T.);
#27864=ORIENTED_EDGE('',*,*,#20260,.T.);
#27865=ORIENTED_EDGE('',*,*,#20261,.T.);
#27866=ORIENTED_EDGE('',*,*,#20259,.F.);
#27867=ORIENTED_EDGE('',*,*,#20262,.T.);
#27868=ORIENTED_EDGE('',*,*,#20263,.T.);
#27869=ORIENTED_EDGE('',*,*,#20264,.F.);
#27870=ORIENTED_EDGE('',*,*,#20265,.T.);
#27871=ORIENTED_EDGE('',*,*,#20266,.T.);
#27872=ORIENTED_EDGE('',*,*,#20267,.T.);
#27873=ORIENTED_EDGE('',*,*,#20268,.T.);
#27874=ORIENTED_EDGE('',*,*,#20269,.T.);
#27875=ORIENTED_EDGE('',*,*,#20270,.T.);
#27876=ORIENTED_EDGE('',*,*,#20269,.F.);
#27877=ORIENTED_EDGE('',*,*,#20271,.F.);
#27878=ORIENTED_EDGE('',*,*,#20272,.F.);
#27879=ORIENTED_EDGE('',*,*,#20273,.F.);
#27880=ORIENTED_EDGE('',*,*,#20268,.F.);
#27881=ORIENTED_EDGE('',*,*,#20274,.F.);
#27882=ORIENTED_EDGE('',*,*,#20275,.T.);
#27883=ORIENTED_EDGE('',*,*,#20276,.T.);
#27884=ORIENTED_EDGE('',*,*,#20271,.T.);
#27885=ORIENTED_EDGE('',*,*,#20267,.F.);
#27886=ORIENTED_EDGE('',*,*,#20277,.T.);
#27887=ORIENTED_EDGE('',*,*,#20278,.F.);
#27888=ORIENTED_EDGE('',*,*,#20279,.F.);
#27889=ORIENTED_EDGE('',*,*,#20280,.T.);
#27890=ORIENTED_EDGE('',*,*,#20274,.T.);
#27891=ORIENTED_EDGE('',*,*,#20281,.F.);
#27892=ORIENTED_EDGE('',*,*,#20282,.F.);
#27893=ORIENTED_EDGE('',*,*,#20283,.F.);
#27894=ORIENTED_EDGE('',*,*,#20278,.T.);
#27895=ORIENTED_EDGE('',*,*,#20284,.T.);
#27896=ORIENTED_EDGE('',*,*,#20282,.T.);
#27897=ORIENTED_EDGE('',*,*,#20285,.T.);
#27898=ORIENTED_EDGE('',*,*,#20286,.T.);
#27899=ORIENTED_EDGE('',*,*,#20265,.F.);
#27900=ORIENTED_EDGE('',*,*,#20287,.T.);
#27901=ORIENTED_EDGE('',*,*,#20288,.T.);
#27902=ORIENTED_EDGE('',*,*,#20283,.T.);
#27903=ORIENTED_EDGE('',*,*,#20289,.T.);
#27904=ORIENTED_EDGE('',*,*,#20290,.F.);
#27905=ORIENTED_EDGE('',*,*,#20291,.F.);
#27906=ORIENTED_EDGE('',*,*,#20292,.F.);
#27907=ORIENTED_EDGE('',*,*,#20293,.T.);
#27908=ORIENTED_EDGE('',*,*,#20294,.T.);
#27909=ORIENTED_EDGE('',*,*,#20291,.T.);
#27910=ORIENTED_EDGE('',*,*,#20295,.T.);
#27911=ORIENTED_EDGE('',*,*,#20296,.T.);
#27912=ORIENTED_EDGE('',*,*,#20281,.T.);
#27913=ORIENTED_EDGE('',*,*,#20297,.T.);
#27914=ORIENTED_EDGE('',*,*,#20292,.T.);
#27915=ORIENTED_EDGE('',*,*,#20298,.T.);
#27916=ORIENTED_EDGE('',*,*,#20299,.F.);
#27917=ORIENTED_EDGE('',*,*,#20300,.F.);
#27918=ORIENTED_EDGE('',*,*,#20301,.F.);
#27919=ORIENTED_EDGE('',*,*,#20302,.T.);
#27920=ORIENTED_EDGE('',*,*,#20303,.T.);
#27921=ORIENTED_EDGE('',*,*,#20300,.T.);
#27922=ORIENTED_EDGE('',*,*,#20304,.T.);
#27923=ORIENTED_EDGE('',*,*,#20305,.T.);
#27924=ORIENTED_EDGE('',*,*,#20290,.T.);
#27925=ORIENTED_EDGE('',*,*,#20306,.T.);
#27926=ORIENTED_EDGE('',*,*,#20301,.T.);
#27927=ORIENTED_EDGE('',*,*,#20307,.T.);
#27928=ORIENTED_EDGE('',*,*,#20308,.F.);
#27929=ORIENTED_EDGE('',*,*,#20309,.F.);
#27930=ORIENTED_EDGE('',*,*,#20310,.F.);
#27931=ORIENTED_EDGE('',*,*,#20311,.T.);
#27932=ORIENTED_EDGE('',*,*,#20312,.T.);
#27933=ORIENTED_EDGE('',*,*,#20309,.T.);
#27934=ORIENTED_EDGE('',*,*,#20313,.T.);
#27935=ORIENTED_EDGE('',*,*,#20314,.T.);
#27936=ORIENTED_EDGE('',*,*,#20299,.T.);
#27937=ORIENTED_EDGE('',*,*,#20315,.T.);
#27938=ORIENTED_EDGE('',*,*,#20310,.T.);
#27939=ORIENTED_EDGE('',*,*,#20316,.T.);
#27940=ORIENTED_EDGE('',*,*,#20317,.F.);
#27941=ORIENTED_EDGE('',*,*,#20318,.F.);
#27942=ORIENTED_EDGE('',*,*,#20319,.F.);
#27943=ORIENTED_EDGE('',*,*,#20320,.T.);
#27944=ORIENTED_EDGE('',*,*,#20321,.T.);
#27945=ORIENTED_EDGE('',*,*,#20318,.T.);
#27946=ORIENTED_EDGE('',*,*,#20322,.T.);
#27947=ORIENTED_EDGE('',*,*,#20323,.T.);
#27948=ORIENTED_EDGE('',*,*,#20308,.T.);
#27949=ORIENTED_EDGE('',*,*,#20324,.T.);
#27950=ORIENTED_EDGE('',*,*,#20319,.T.);
#27951=ORIENTED_EDGE('',*,*,#20325,.T.);
#27952=ORIENTED_EDGE('',*,*,#20326,.F.);
#27953=ORIENTED_EDGE('',*,*,#20327,.F.);
#27954=ORIENTED_EDGE('',*,*,#20328,.F.);
#27955=ORIENTED_EDGE('',*,*,#20329,.T.);
#27956=ORIENTED_EDGE('',*,*,#20330,.T.);
#27957=ORIENTED_EDGE('',*,*,#20327,.T.);
#27958=ORIENTED_EDGE('',*,*,#20331,.T.);
#27959=ORIENTED_EDGE('',*,*,#20332,.T.);
#27960=ORIENTED_EDGE('',*,*,#20317,.T.);
#27961=ORIENTED_EDGE('',*,*,#20333,.T.);
#27962=ORIENTED_EDGE('',*,*,#20328,.T.);
#27963=ORIENTED_EDGE('',*,*,#20334,.T.);
#27964=ORIENTED_EDGE('',*,*,#20335,.T.);
#27965=ORIENTED_EDGE('',*,*,#20336,.T.);
#27966=ORIENTED_EDGE('',*,*,#20326,.T.);
#27967=ORIENTED_EDGE('',*,*,#20337,.T.);
#27968=ORIENTED_EDGE('',*,*,#20338,.T.);
#27969=ORIENTED_EDGE('',*,*,#20302,.F.);
#27970=ORIENTED_EDGE('',*,*,#20339,.F.);
#27971=ORIENTED_EDGE('',*,*,#20340,.T.);
#27972=ORIENTED_EDGE('',*,*,#20341,.T.);
#27973=ORIENTED_EDGE('',*,*,#20296,.F.);
#27974=ORIENTED_EDGE('',*,*,#20342,.T.);
#27975=ORIENTED_EDGE('',*,*,#20304,.F.);
#27976=ORIENTED_EDGE('',*,*,#20316,.F.);
#27977=ORIENTED_EDGE('',*,*,#20312,.F.);
#27978=ORIENTED_EDGE('',*,*,#20343,.F.);
#27979=ORIENTED_EDGE('',*,*,#20305,.F.);
#27980=ORIENTED_EDGE('',*,*,#20343,.T.);
#27981=ORIENTED_EDGE('',*,*,#20311,.F.);
#27982=ORIENTED_EDGE('',*,*,#20344,.F.);
#27983=ORIENTED_EDGE('',*,*,#20345,.T.);
#27984=ORIENTED_EDGE('',*,*,#20339,.T.);
#27985=ORIENTED_EDGE('',*,*,#20313,.F.);
#27986=ORIENTED_EDGE('',*,*,#20325,.F.);
#27987=ORIENTED_EDGE('',*,*,#20321,.F.);
#27988=ORIENTED_EDGE('',*,*,#20346,.F.);
#27989=ORIENTED_EDGE('',*,*,#20314,.F.);
#27990=ORIENTED_EDGE('',*,*,#20346,.T.);
#27991=ORIENTED_EDGE('',*,*,#20320,.F.);
#27992=ORIENTED_EDGE('',*,*,#20347,.F.);
#27993=ORIENTED_EDGE('',*,*,#20348,.T.);
#27994=ORIENTED_EDGE('',*,*,#20344,.T.);
#27995=ORIENTED_EDGE('',*,*,#20322,.F.);
#27996=ORIENTED_EDGE('',*,*,#20334,.F.);
#27997=ORIENTED_EDGE('',*,*,#20330,.F.);
#27998=ORIENTED_EDGE('',*,*,#20349,.F.);
#27999=ORIENTED_EDGE('',*,*,#20323,.F.);
#28000=ORIENTED_EDGE('',*,*,#20349,.T.);
#28001=ORIENTED_EDGE('',*,*,#20329,.F.);
#28002=ORIENTED_EDGE('',*,*,#20350,.F.);
#28003=ORIENTED_EDGE('',*,*,#20351,.T.);
#28004=ORIENTED_EDGE('',*,*,#20347,.T.);
#28005=ORIENTED_EDGE('',*,*,#20332,.F.);
#28006=ORIENTED_EDGE('',*,*,#20352,.T.);
#28007=ORIENTED_EDGE('',*,*,#20353,.T.);
#28008=ORIENTED_EDGE('',*,*,#20354,.T.);
#28009=ORIENTED_EDGE('',*,*,#20350,.T.);
#28010=ORIENTED_EDGE('',*,*,#20331,.F.);
#28011=ORIENTED_EDGE('',*,*,#20336,.F.);
#28012=ORIENTED_EDGE('',*,*,#20355,.F.);
#28013=ORIENTED_EDGE('',*,*,#20352,.F.);
#28014=ORIENTED_EDGE('',*,*,#20335,.F.);
#28015=ORIENTED_EDGE('',*,*,#20356,.T.);
#28016=ORIENTED_EDGE('',*,*,#20272,.T.);
#28017=ORIENTED_EDGE('',*,*,#20357,.T.);
#28018=ORIENTED_EDGE('',*,*,#20355,.T.);
#28019=ORIENTED_EDGE('',*,*,#20358,.T.);
#28020=ORIENTED_EDGE('',*,*,#20359,.T.);
#28021=ORIENTED_EDGE('',*,*,#20360,.T.);
#28022=ORIENTED_EDGE('',*,*,#20359,.F.);
#28023=ORIENTED_EDGE('',*,*,#20288,.F.);
#28024=ORIENTED_EDGE('',*,*,#20361,.F.);
#28025=ORIENTED_EDGE('',*,*,#20337,.F.);
#28026=ORIENTED_EDGE('',*,*,#20333,.F.);
#28027=ORIENTED_EDGE('',*,*,#20324,.F.);
#28028=ORIENTED_EDGE('',*,*,#20315,.F.);
#28029=ORIENTED_EDGE('',*,*,#20306,.F.);
#28030=ORIENTED_EDGE('',*,*,#20297,.F.);
#28031=ORIENTED_EDGE('',*,*,#20362,.F.);
#28032=ORIENTED_EDGE('',*,*,#20363,.F.);
#28033=ORIENTED_EDGE('',*,*,#20364,.F.);
#28034=ORIENTED_EDGE('',*,*,#20365,.F.);
#28035=ORIENTED_EDGE('',*,*,#20358,.F.);
#28036=ORIENTED_EDGE('',*,*,#20366,.F.);
#28037=ORIENTED_EDGE('',*,*,#20367,.T.);
#28038=ORIENTED_EDGE('',*,*,#20360,.F.);
#28039=ORIENTED_EDGE('',*,*,#20367,.F.);
#28040=ORIENTED_EDGE('',*,*,#20362,.T.);
#28041=ORIENTED_EDGE('',*,*,#20368,.T.);
#28042=ORIENTED_EDGE('',*,*,#20369,.T.);
#28043=ORIENTED_EDGE('',*,*,#20368,.F.);
#28044=ORIENTED_EDGE('',*,*,#20370,.F.);
#28045=ORIENTED_EDGE('',*,*,#20371,.T.);
#28046=ORIENTED_EDGE('',*,*,#20369,.F.);
#28047=ORIENTED_EDGE('',*,*,#20371,.F.);
#28048=ORIENTED_EDGE('',*,*,#20365,.T.);
#28049=ORIENTED_EDGE('',*,*,#20372,.T.);
#28050=ORIENTED_EDGE('',*,*,#20373,.T.);
#28051=ORIENTED_EDGE('',*,*,#20372,.F.);
#28052=ORIENTED_EDGE('',*,*,#20374,.F.);
#28053=ORIENTED_EDGE('',*,*,#20375,.T.);
#28054=ORIENTED_EDGE('',*,*,#20373,.F.);
#28055=ORIENTED_EDGE('',*,*,#20375,.F.);
#28056=ORIENTED_EDGE('',*,*,#20363,.T.);
#28057=ORIENTED_EDGE('',*,*,#20376,.T.);
#28058=ORIENTED_EDGE('',*,*,#20377,.T.);
#28059=ORIENTED_EDGE('',*,*,#20376,.F.);
#28060=ORIENTED_EDGE('',*,*,#20378,.F.);
#28061=ORIENTED_EDGE('',*,*,#20379,.T.);
#28062=ORIENTED_EDGE('',*,*,#20377,.F.);
#28063=ORIENTED_EDGE('',*,*,#20379,.F.);
#28064=ORIENTED_EDGE('',*,*,#20380,.T.);
#28065=ORIENTED_EDGE('',*,*,#20381,.T.);
#28066=ORIENTED_EDGE('',*,*,#20378,.T.);
#28067=ORIENTED_EDGE('',*,*,#20381,.F.);
#28068=ORIENTED_EDGE('',*,*,#20354,.F.);
#28069=ORIENTED_EDGE('',*,*,#20275,.F.);
#28070=ORIENTED_EDGE('',*,*,#20280,.F.);
#28071=ORIENTED_EDGE('',*,*,#20382,.F.);
#28072=ORIENTED_EDGE('',*,*,#20340,.F.);
#28073=ORIENTED_EDGE('',*,*,#20345,.F.);
#28074=ORIENTED_EDGE('',*,*,#20348,.F.);
#28075=ORIENTED_EDGE('',*,*,#20351,.F.);
#28076=ORIENTED_EDGE('',*,*,#20383,.F.);
#28077=ORIENTED_EDGE('',*,*,#20384,.F.);
#28078=ORIENTED_EDGE('',*,*,#20385,.F.);
#28079=ORIENTED_EDGE('',*,*,#20386,.F.);
#28080=ORIENTED_EDGE('',*,*,#20380,.F.);
#28081=ORIENTED_EDGE('',*,*,#20383,.T.);
#28082=ORIENTED_EDGE('',*,*,#20387,.T.);
#28083=ORIENTED_EDGE('',*,*,#20374,.T.);
#28084=ORIENTED_EDGE('',*,*,#20387,.F.);
#28085=ORIENTED_EDGE('',*,*,#20386,.T.);
#28086=ORIENTED_EDGE('',*,*,#20388,.T.);
#28087=ORIENTED_EDGE('',*,*,#20370,.T.);
#28088=ORIENTED_EDGE('',*,*,#20388,.F.);
#28089=ORIENTED_EDGE('',*,*,#20384,.T.);
#28090=ORIENTED_EDGE('',*,*,#20389,.T.);
#28091=ORIENTED_EDGE('',*,*,#20366,.T.);
#28092=ORIENTED_EDGE('',*,*,#20389,.F.);
#28093=ORIENTED_EDGE('',*,*,#20293,.F.);
#28094=ORIENTED_EDGE('',*,*,#20341,.F.);
#28095=ORIENTED_EDGE('',*,*,#20382,.T.);
#28096=ORIENTED_EDGE('',*,*,#20279,.T.);
#28097=ORIENTED_EDGE('',*,*,#20286,.F.);
#28098=ORIENTED_EDGE('',*,*,#20390,.T.);
#28099=ORIENTED_EDGE('',*,*,#20276,.F.);
#28100=ORIENTED_EDGE('',*,*,#20353,.F.);
#28101=ORIENTED_EDGE('',*,*,#20357,.F.);
#28102=ORIENTED_EDGE('',*,*,#20270,.F.);
#28103=ORIENTED_EDGE('',*,*,#20273,.T.);
#28104=ORIENTED_EDGE('',*,*,#20356,.F.);
#28105=ORIENTED_EDGE('',*,*,#20338,.F.);
#28106=ORIENTED_EDGE('',*,*,#20361,.T.);
#28107=ORIENTED_EDGE('',*,*,#20287,.F.);
#28108=ORIENTED_EDGE('',*,*,#20303,.F.);
#28109=ORIENTED_EDGE('',*,*,#20342,.F.);
#28110=ORIENTED_EDGE('',*,*,#20295,.F.);
#28111=ORIENTED_EDGE('',*,*,#20307,.F.);
#28112=ORIENTED_EDGE('',*,*,#20294,.F.);
#28113=ORIENTED_EDGE('',*,*,#20390,.F.);
#28114=ORIENTED_EDGE('',*,*,#20285,.F.);
#28115=ORIENTED_EDGE('',*,*,#20298,.F.);
#28116=ORIENTED_EDGE('',*,*,#20266,.F.);
#28117=ORIENTED_EDGE('',*,*,#20289,.F.);
#28118=ORIENTED_EDGE('',*,*,#20284,.F.);
#28119=ORIENTED_EDGE('',*,*,#20277,.F.);
#28120=ORIENTED_EDGE('',*,*,#20391,.T.);
#28121=ORIENTED_EDGE('',*,*,#20392,.T.);
#28122=ORIENTED_EDGE('',*,*,#20393,.T.);
#28123=ORIENTED_EDGE('',*,*,#20394,.T.);
#28124=ORIENTED_EDGE('',*,*,#20395,.T.);
#28125=ORIENTED_EDGE('',*,*,#20393,.F.);
#28126=ORIENTED_EDGE('',*,*,#20394,.F.);
#28127=ORIENTED_EDGE('',*,*,#20395,.F.);
#28128=ORIENTED_EDGE('',*,*,#20396,.T.);
#28129=ORIENTED_EDGE('',*,*,#20397,.F.);
#28130=ORIENTED_EDGE('',*,*,#20398,.F.);
#28131=ORIENTED_EDGE('',*,*,#20396,.F.);
#28132=ORIENTED_EDGE('',*,*,#20385,.T.);
#28133=ORIENTED_EDGE('',*,*,#20399,.T.);
#28134=ORIENTED_EDGE('',*,*,#20391,.F.);
#28135=ORIENTED_EDGE('',*,*,#20392,.F.);
#28136=ORIENTED_EDGE('',*,*,#20399,.F.);
#28137=ORIENTED_EDGE('',*,*,#20397,.T.);
#28138=ORIENTED_EDGE('',*,*,#20398,.T.);
#28139=ORIENTED_EDGE('',*,*,#20400,.T.);
#28140=ORIENTED_EDGE('',*,*,#20401,.T.);
#28141=ORIENTED_EDGE('',*,*,#20400,.F.);
#28142=ORIENTED_EDGE('',*,*,#20401,.F.);
#28143=ORIENTED_EDGE('',*,*,#20402,.F.);
#28144=ORIENTED_EDGE('',*,*,#20403,.T.);
#28145=ORIENTED_EDGE('',*,*,#20404,.F.);
#28146=ORIENTED_EDGE('',*,*,#20405,.F.);
#28147=ORIENTED_EDGE('',*,*,#20406,.F.);
#28148=ORIENTED_EDGE('',*,*,#20407,.F.);
#28149=ORIENTED_EDGE('',*,*,#20408,.F.);
#28150=ORIENTED_EDGE('',*,*,#20409,.F.);
#28151=ORIENTED_EDGE('',*,*,#20410,.F.);
#28152=ORIENTED_EDGE('',*,*,#20411,.F.);
#28153=ORIENTED_EDGE('',*,*,#20412,.F.);
#28154=ORIENTED_EDGE('',*,*,#20413,.F.);
#28155=ORIENTED_EDGE('',*,*,#20414,.F.);
#28156=ORIENTED_EDGE('',*,*,#20415,.T.);
#28157=ORIENTED_EDGE('',*,*,#20252,.T.);
#28158=ORIENTED_EDGE('',*,*,#20249,.T.);
#28159=ORIENTED_EDGE('',*,*,#20246,.T.);
#28160=ORIENTED_EDGE('',*,*,#20416,.F.);
#28161=ORIENTED_EDGE('',*,*,#20417,.F.);
#28162=ORIENTED_EDGE('',*,*,#20418,.F.);
#28163=ORIENTED_EDGE('',*,*,#20419,.F.);
#28164=ORIENTED_EDGE('',*,*,#20420,.F.);
#28165=ORIENTED_EDGE('',*,*,#20421,.T.);
#28166=ORIENTED_EDGE('',*,*,#20242,.T.);
#28167=ORIENTED_EDGE('',*,*,#20239,.T.);
#28168=ORIENTED_EDGE('',*,*,#20236,.T.);
#28169=ORIENTED_EDGE('',*,*,#20233,.T.);
#28170=ORIENTED_EDGE('',*,*,#20230,.T.);
#28171=ORIENTED_EDGE('',*,*,#20227,.T.);
#28172=ORIENTED_EDGE('',*,*,#20422,.F.);
#28173=ORIENTED_EDGE('',*,*,#20423,.F.);
#28174=ORIENTED_EDGE('',*,*,#20424,.F.);
#28175=ORIENTED_EDGE('',*,*,#20425,.F.);
#28176=ORIENTED_EDGE('',*,*,#20426,.F.);
#28177=ORIENTED_EDGE('',*,*,#20427,.F.);
#28178=ORIENTED_EDGE('',*,*,#20428,.F.);
#28179=ORIENTED_EDGE('',*,*,#20429,.F.);
#28180=ORIENTED_EDGE('',*,*,#20430,.F.);
#28181=ORIENTED_EDGE('',*,*,#20431,.F.);
#28182=ORIENTED_EDGE('',*,*,#20432,.F.);
#28183=ORIENTED_EDGE('',*,*,#20433,.F.);
#28184=ORIENTED_EDGE('',*,*,#20434,.F.);
#28185=ORIENTED_EDGE('',*,*,#20435,.F.);
#28186=ORIENTED_EDGE('',*,*,#20436,.F.);
#28187=ORIENTED_EDGE('',*,*,#20437,.F.);
#28188=ORIENTED_EDGE('',*,*,#20224,.T.);
#28189=ORIENTED_EDGE('',*,*,#20438,.F.);
#28190=ORIENTED_EDGE('',*,*,#20439,.F.);
#28191=ORIENTED_EDGE('',*,*,#20440,.F.);
#28192=ORIENTED_EDGE('',*,*,#20441,.T.);
#28193=ORIENTED_EDGE('',*,*,#20442,.F.);
#28194=ORIENTED_EDGE('',*,*,#20443,.T.);
#28195=ORIENTED_EDGE('',*,*,#20444,.F.);
#28196=ORIENTED_EDGE('',*,*,#20445,.F.);
#28197=ORIENTED_EDGE('',*,*,#20446,.F.);
#28198=ORIENTED_EDGE('',*,*,#20447,.F.);
#28199=ORIENTED_EDGE('',*,*,#20448,.F.);
#28200=ORIENTED_EDGE('',*,*,#20244,.F.);
#28201=ORIENTED_EDGE('',*,*,#20248,.F.);
#28202=ORIENTED_EDGE('',*,*,#20251,.F.);
#28203=ORIENTED_EDGE('',*,*,#20449,.F.);
#28204=ORIENTED_EDGE('',*,*,#20450,.F.);
#28205=ORIENTED_EDGE('',*,*,#20451,.F.);
#28206=ORIENTED_EDGE('',*,*,#20452,.F.);
#28207=ORIENTED_EDGE('',*,*,#20453,.F.);
#28208=ORIENTED_EDGE('',*,*,#20454,.F.);
#28209=ORIENTED_EDGE('',*,*,#20455,.F.);
#28210=ORIENTED_EDGE('',*,*,#20456,.F.);
#28211=ORIENTED_EDGE('',*,*,#20457,.F.);
#28212=ORIENTED_EDGE('',*,*,#20458,.F.);
#28213=ORIENTED_EDGE('',*,*,#20459,.F.);
#28214=ORIENTED_EDGE('',*,*,#20460,.F.);
#28215=ORIENTED_EDGE('',*,*,#20461,.F.);
#28216=ORIENTED_EDGE('',*,*,#20462,.F.);
#28217=ORIENTED_EDGE('',*,*,#20463,.F.);
#28218=ORIENTED_EDGE('',*,*,#20464,.F.);
#28219=ORIENTED_EDGE('',*,*,#20465,.F.);
#28220=ORIENTED_EDGE('',*,*,#20466,.F.);
#28221=ORIENTED_EDGE('',*,*,#20467,.F.);
#28222=ORIENTED_EDGE('',*,*,#20468,.F.);
#28223=ORIENTED_EDGE('',*,*,#20469,.F.);
#28224=ORIENTED_EDGE('',*,*,#20470,.F.);
#28225=ORIENTED_EDGE('',*,*,#20471,.F.);
#28226=ORIENTED_EDGE('',*,*,#20472,.F.);
#28227=ORIENTED_EDGE('',*,*,#20473,.F.);
#28228=ORIENTED_EDGE('',*,*,#20474,.F.);
#28229=ORIENTED_EDGE('',*,*,#20475,.F.);
#28230=ORIENTED_EDGE('',*,*,#20476,.F.);
#28231=ORIENTED_EDGE('',*,*,#20222,.F.);
#28232=ORIENTED_EDGE('',*,*,#20229,.F.);
#28233=ORIENTED_EDGE('',*,*,#20232,.F.);
#28234=ORIENTED_EDGE('',*,*,#20235,.F.);
#28235=ORIENTED_EDGE('',*,*,#20238,.F.);
#28236=ORIENTED_EDGE('',*,*,#20241,.F.);
#28237=ORIENTED_EDGE('',*,*,#20477,.F.);
#28238=ORIENTED_EDGE('',*,*,#20478,.F.);
#28239=ORIENTED_EDGE('',*,*,#20479,.F.);
#28240=ORIENTED_EDGE('',*,*,#20480,.F.);
#28241=ORIENTED_EDGE('',*,*,#20481,.F.);
#28242=ORIENTED_EDGE('',*,*,#20482,.F.);
#28243=ORIENTED_EDGE('',*,*,#20483,.F.);
#28244=ORIENTED_EDGE('',*,*,#20250,.T.);
#28245=ORIENTED_EDGE('',*,*,#20415,.F.);
#28246=ORIENTED_EDGE('',*,*,#20484,.F.);
#28247=ORIENTED_EDGE('',*,*,#20459,.T.);
#28248=ORIENTED_EDGE('',*,*,#20485,.F.);
#28249=ORIENTED_EDGE('',*,*,#20449,.T.);
#28250=ORIENTED_EDGE('',*,*,#20240,.T.);
#28251=ORIENTED_EDGE('',*,*,#20421,.F.);
#28252=ORIENTED_EDGE('',*,*,#20486,.F.);
#28253=ORIENTED_EDGE('',*,*,#20477,.T.);
#28254=ORIENTED_EDGE('',*,*,#20487,.F.);
#28255=ORIENTED_EDGE('',*,*,#20463,.T.);
#28256=ORIENTED_EDGE('',*,*,#20488,.F.);
#28257=ORIENTED_EDGE('',*,*,#20403,.F.);
#28258=ORIENTED_EDGE('',*,*,#20489,.F.);
#28259=ORIENTED_EDGE('',*,*,#20441,.F.);
#28260=ORIENTED_EDGE('',*,*,#20490,.F.);
#28261=ORIENTED_EDGE('',*,*,#20481,.T.);
#28262=ORIENTED_EDGE('',*,*,#20491,.F.);
#28263=ORIENTED_EDGE('',*,*,#20492,.T.);
#28264=ORIENTED_EDGE('',*,*,#20493,.F.);
#28265=ORIENTED_EDGE('',*,*,#20443,.F.);
#28266=ORIENTED_EDGE('',*,*,#20245,.T.);
#28267=ORIENTED_EDGE('',*,*,#20448,.T.);
#28268=ORIENTED_EDGE('',*,*,#20494,.F.);
#28269=ORIENTED_EDGE('',*,*,#20495,.F.);
#28270=ORIENTED_EDGE('',*,*,#20416,.T.);
#28271=ORIENTED_EDGE('',*,*,#20496,.F.);
#28272=ORIENTED_EDGE('',*,*,#20497,.T.);
#28273=ORIENTED_EDGE('',*,*,#20478,.T.);
#28274=ORIENTED_EDGE('',*,*,#20486,.T.);
#28275=ORIENTED_EDGE('',*,*,#20420,.T.);
#28276=ORIENTED_EDGE('',*,*,#20498,.T.);
#28277=ORIENTED_EDGE('',*,*,#20499,.T.);
#28278=ORIENTED_EDGE('',*,*,#20500,.F.);
#28279=ORIENTED_EDGE('',*,*,#20501,.F.);
#28280=ORIENTED_EDGE('',*,*,#20502,.F.);
#28281=ORIENTED_EDGE('',*,*,#20492,.F.);
#28282=ORIENTED_EDGE('',*,*,#20423,.T.);
#28283=ORIENTED_EDGE('',*,*,#20503,.F.);
#28284=ORIENTED_EDGE('',*,*,#20504,.F.);
#28285=ORIENTED_EDGE('',*,*,#20474,.T.);
#28286=ORIENTED_EDGE('',*,*,#20505,.F.);
#28287=ORIENTED_EDGE('',*,*,#20425,.T.);
#28288=ORIENTED_EDGE('',*,*,#20506,.F.);
#28289=ORIENTED_EDGE('',*,*,#20427,.T.);
#28290=ORIENTED_EDGE('',*,*,#20507,.F.);
#28291=ORIENTED_EDGE('',*,*,#20472,.T.);
#28292=ORIENTED_EDGE('',*,*,#20508,.F.);
#28293=ORIENTED_EDGE('',*,*,#20429,.T.);
#28294=ORIENTED_EDGE('',*,*,#20509,.F.);
#28295=ORIENTED_EDGE('',*,*,#20470,.T.);
#28296=ORIENTED_EDGE('',*,*,#20510,.F.);
#28297=ORIENTED_EDGE('',*,*,#20431,.T.);
#28298=ORIENTED_EDGE('',*,*,#20511,.F.);
#28299=ORIENTED_EDGE('',*,*,#20468,.T.);
#28300=ORIENTED_EDGE('',*,*,#20512,.F.);
#28301=ORIENTED_EDGE('',*,*,#20433,.T.);
#28302=ORIENTED_EDGE('',*,*,#20513,.F.);
#28303=ORIENTED_EDGE('',*,*,#20466,.T.);
#28304=ORIENTED_EDGE('',*,*,#20514,.F.);
#28305=ORIENTED_EDGE('',*,*,#20418,.T.);
#28306=ORIENTED_EDGE('',*,*,#20515,.F.);
#28307=ORIENTED_EDGE('',*,*,#20464,.T.);
#28308=ORIENTED_EDGE('',*,*,#20516,.F.);
#28309=ORIENTED_EDGE('',*,*,#20454,.T.);
#28310=ORIENTED_EDGE('',*,*,#20517,.F.);
#28311=ORIENTED_EDGE('',*,*,#20411,.T.);
#28312=ORIENTED_EDGE('',*,*,#20518,.F.);
#28313=ORIENTED_EDGE('',*,*,#20446,.T.);
#28314=ORIENTED_EDGE('',*,*,#20519,.F.);
#28315=ORIENTED_EDGE('',*,*,#20409,.T.);
#28316=ORIENTED_EDGE('',*,*,#20520,.F.);
#28317=ORIENTED_EDGE('',*,*,#20407,.T.);
#28318=ORIENTED_EDGE('',*,*,#20521,.F.);
#28319=ORIENTED_EDGE('',*,*,#20522,.F.);
#28320=ORIENTED_EDGE('',*,*,#20523,.F.);
#28321=ORIENTED_EDGE('',*,*,#20405,.T.);
#28322=ORIENTED_EDGE('',*,*,#20524,.F.);
#28323=ORIENTED_EDGE('',*,*,#20413,.T.);
#28324=ORIENTED_EDGE('',*,*,#20525,.F.);
#28325=ORIENTED_EDGE('',*,*,#20452,.T.);
#28326=ORIENTED_EDGE('',*,*,#20526,.F.);
#28327=ORIENTED_EDGE('',*,*,#20453,.T.);
#28328=ORIENTED_EDGE('',*,*,#20525,.T.);
#28329=ORIENTED_EDGE('',*,*,#20412,.T.);
#28330=ORIENTED_EDGE('',*,*,#20517,.T.);
#28331=ORIENTED_EDGE('',*,*,#20406,.T.);
#28332=ORIENTED_EDGE('',*,*,#20526,.T.);
#28333=ORIENTED_EDGE('',*,*,#20451,.T.);
#28334=ORIENTED_EDGE('',*,*,#20527,.T.);
#28335=ORIENTED_EDGE('',*,*,#20455,.T.);
#28336=ORIENTED_EDGE('',*,*,#20518,.T.);
#28337=ORIENTED_EDGE('',*,*,#20410,.T.);
#28338=ORIENTED_EDGE('',*,*,#20519,.T.);
#28339=ORIENTED_EDGE('',*,*,#20447,.T.);
#28340=ORIENTED_EDGE('',*,*,#20520,.T.);
#28341=ORIENTED_EDGE('',*,*,#20408,.T.);
#28342=ORIENTED_EDGE('',*,*,#20523,.T.);
#28343=ORIENTED_EDGE('',*,*,#20528,.F.);
#28344=ORIENTED_EDGE('',*,*,#20417,.T.);
#28345=ORIENTED_EDGE('',*,*,#20529,.F.);
#28346=ORIENTED_EDGE('',*,*,#20521,.T.);
#28347=ORIENTED_EDGE('',*,*,#20445,.T.);
#28348=ORIENTED_EDGE('',*,*,#20530,.T.);
#28349=ORIENTED_EDGE('',*,*,#20457,.T.);
#28350=ORIENTED_EDGE('',*,*,#20531,.T.);
#28351=ORIENTED_EDGE('',*,*,#20426,.T.);
#28352=ORIENTED_EDGE('',*,*,#20505,.T.);
#28353=ORIENTED_EDGE('',*,*,#20473,.T.);
#28354=ORIENTED_EDGE('',*,*,#20507,.T.);
#28355=ORIENTED_EDGE('',*,*,#20428,.T.);
#28356=ORIENTED_EDGE('',*,*,#20508,.T.);
#28357=ORIENTED_EDGE('',*,*,#20471,.T.);
#28358=ORIENTED_EDGE('',*,*,#20509,.T.);
#28359=ORIENTED_EDGE('',*,*,#20430,.T.);
#28360=ORIENTED_EDGE('',*,*,#20510,.T.);
#28361=ORIENTED_EDGE('',*,*,#20469,.T.);
#28362=ORIENTED_EDGE('',*,*,#20511,.T.);
#28363=ORIENTED_EDGE('',*,*,#20432,.T.);
#28364=ORIENTED_EDGE('',*,*,#20512,.T.);
#28365=ORIENTED_EDGE('',*,*,#20467,.T.);
#28366=ORIENTED_EDGE('',*,*,#20513,.T.);
#28367=ORIENTED_EDGE('',*,*,#20434,.T.);
#28368=ORIENTED_EDGE('',*,*,#20514,.T.);
#28369=ORIENTED_EDGE('',*,*,#20465,.T.);
#28370=ORIENTED_EDGE('',*,*,#20515,.T.);
#28371=ORIENTED_EDGE('',*,*,#20419,.T.);
#28372=ORIENTED_EDGE('',*,*,#20516,.T.);
#28373=ORIENTED_EDGE('',*,*,#20479,.T.);
#28374=ORIENTED_EDGE('',*,*,#20532,.T.);
#28375=ORIENTED_EDGE('',*,*,#20483,.T.);
#28376=ORIENTED_EDGE('',*,*,#20533,.T.);
#28377=ORIENTED_EDGE('',*,*,#20534,.T.);
#28378=ORIENTED_EDGE('',*,*,#20475,.T.);
#28379=ORIENTED_EDGE('',*,*,#20506,.T.);
#28380=ORIENTED_EDGE('',*,*,#20424,.T.);
#28381=ORIENTED_EDGE('',*,*,#20504,.T.);
#28382=ORIENTED_EDGE('',*,*,#20535,.T.);
#28383=ORIENTED_EDGE('',*,*,#20439,.T.);
#28384=ORIENTED_EDGE('',*,*,#20536,.T.);
#28385=ORIENTED_EDGE('',*,*,#20461,.T.);
#28386=ORIENTED_EDGE('',*,*,#20537,.T.);
#28387=ORIENTED_EDGE('',*,*,#20502,.T.);
#28388=ORIENTED_EDGE('',*,*,#20538,.F.);
#28389=ORIENTED_EDGE('',*,*,#20435,.T.);
#28390=ORIENTED_EDGE('',*,*,#20223,.T.);
#28391=ORIENTED_EDGE('',*,*,#20476,.T.);
#28392=ORIENTED_EDGE('',*,*,#20534,.F.);
#28393=ORIENTED_EDGE('',*,*,#20539,.T.);
#28394=ORIENTED_EDGE('',*,*,#20225,.T.);
#28395=ORIENTED_EDGE('',*,*,#20437,.T.);
#28396=ORIENTED_EDGE('',*,*,#20540,.F.);
#28397=ORIENTED_EDGE('',*,*,#20500,.T.);
#28398=ORIENTED_EDGE('',*,*,#20491,.T.);
#28399=ORIENTED_EDGE('',*,*,#20442,.T.);
#28400=ORIENTED_EDGE('',*,*,#20531,.F.);
#28401=ORIENTED_EDGE('',*,*,#20456,.T.);
#28402=ORIENTED_EDGE('',*,*,#20484,.T.);
#28403=ORIENTED_EDGE('',*,*,#20414,.T.);
#28404=ORIENTED_EDGE('',*,*,#20524,.T.);
#28405=ORIENTED_EDGE('',*,*,#20404,.T.);
#28406=ORIENTED_EDGE('',*,*,#20488,.T.);
#28407=ORIENTED_EDGE('',*,*,#20462,.T.);
#28408=ORIENTED_EDGE('',*,*,#20536,.F.);
#28409=ORIENTED_EDGE('',*,*,#20438,.T.);
#28410=ORIENTED_EDGE('',*,*,#20489,.T.);
#28411=ORIENTED_EDGE('',*,*,#20480,.T.);
#28412=ORIENTED_EDGE('',*,*,#20535,.F.);
#28413=ORIENTED_EDGE('',*,*,#20503,.T.);
#28414=ORIENTED_EDGE('',*,*,#20422,.T.);
#28415=ORIENTED_EDGE('',*,*,#20226,.T.);
#28416=ORIENTED_EDGE('',*,*,#20539,.F.);
#28417=ORIENTED_EDGE('',*,*,#20533,.F.);
#28418=ORIENTED_EDGE('',*,*,#20482,.T.);
#28419=ORIENTED_EDGE('',*,*,#20490,.T.);
#28420=ORIENTED_EDGE('',*,*,#20440,.T.);
#28421=ORIENTED_EDGE('',*,*,#20537,.F.);
#28422=ORIENTED_EDGE('',*,*,#20460,.T.);
#28423=ORIENTED_EDGE('',*,*,#20487,.T.);
#28424=ORIENTED_EDGE('',*,*,#20402,.T.);
#28425=ORIENTED_EDGE('',*,*,#20527,.F.);
#28426=ORIENTED_EDGE('',*,*,#20450,.T.);
#28427=ORIENTED_EDGE('',*,*,#20485,.T.);
#28428=ORIENTED_EDGE('',*,*,#20458,.T.);
#28429=ORIENTED_EDGE('',*,*,#20530,.F.);
#28430=ORIENTED_EDGE('',*,*,#20444,.T.);
#28431=ORIENTED_EDGE('',*,*,#20493,.T.);
#28432=ORIENTED_EDGE('',*,*,#20541,.F.);
#28433=ORIENTED_EDGE('',*,*,#20542,.T.);
#28434=ORIENTED_EDGE('',*,*,#20364,.T.);
#28435=ORIENTED_EDGE('',*,*,#20542,.F.);
#28436=ORIENTED_EDGE('',*,*,#20543,.F.);
#28437=ORIENTED_EDGE('',*,*,#20544,.T.);
#28438=ORIENTED_EDGE('',*,*,#20541,.T.);
#28439=ORIENTED_EDGE('',*,*,#20544,.F.);
#28440=ORIENTED_EDGE('',*,*,#20543,.T.);
#28441=ORIENTED_EDGE('',*,*,#20545,.F.);
#28442=ORIENTED_EDGE('',*,*,#20546,.F.);
#28443=ORIENTED_EDGE('',*,*,#20547,.T.);
#28444=ORIENTED_EDGE('',*,*,#20545,.T.);
#28445=ORIENTED_EDGE('',*,*,#20547,.F.);
#28446=ORIENTED_EDGE('',*,*,#20548,.F.);
#28447=ORIENTED_EDGE('',*,*,#20549,.T.);
#28448=ORIENTED_EDGE('',*,*,#20546,.T.);
#28449=ORIENTED_EDGE('',*,*,#20549,.F.);
#28450=ORIENTED_EDGE('',*,*,#20550,.F.);
#28451=ORIENTED_EDGE('',*,*,#20551,.T.);
#28452=ORIENTED_EDGE('',*,*,#20548,.T.);
#28453=ORIENTED_EDGE('',*,*,#20551,.F.);
#28454=ORIENTED_EDGE('',*,*,#20552,.F.);
#28455=ORIENTED_EDGE('',*,*,#20553,.T.);
#28456=ORIENTED_EDGE('',*,*,#20550,.T.);
#28457=ORIENTED_EDGE('',*,*,#20553,.F.);
#28458=ORIENTED_EDGE('',*,*,#20554,.F.);
#28459=ORIENTED_EDGE('',*,*,#20555,.F.);
#28460=ORIENTED_EDGE('',*,*,#20263,.F.);
#28461=ORIENTED_EDGE('',*,*,#20556,.F.);
#28462=ORIENTED_EDGE('',*,*,#20557,.F.);
#28463=ORIENTED_EDGE('',*,*,#20558,.F.);
#28464=ORIENTED_EDGE('',*,*,#20556,.T.);
#28465=ORIENTED_EDGE('',*,*,#20262,.F.);
#28466=ORIENTED_EDGE('',*,*,#20258,.F.);
#28467=ORIENTED_EDGE('',*,*,#20559,.T.);
#28468=ORIENTED_EDGE('',*,*,#20554,.T.);
#28469=ORIENTED_EDGE('',*,*,#20558,.T.);
#28470=ORIENTED_EDGE('',*,*,#20560,.F.);
#28471=ORIENTED_EDGE('',*,*,#20561,.T.);
#28472=ORIENTED_EDGE('',*,*,#20552,.T.);
#28473=ORIENTED_EDGE('',*,*,#20561,.F.);
#28474=ORIENTED_EDGE('',*,*,#20562,.F.);
#28475=ORIENTED_EDGE('',*,*,#20563,.F.);
#28476=ORIENTED_EDGE('',*,*,#20260,.F.);
#28477=ORIENTED_EDGE('',*,*,#20264,.T.);
#28478=ORIENTED_EDGE('',*,*,#20555,.T.);
#28479=ORIENTED_EDGE('',*,*,#20559,.F.);
#28480=ORIENTED_EDGE('',*,*,#20563,.T.);
#28481=ORIENTED_EDGE('',*,*,#20562,.T.);
#28482=ORIENTED_EDGE('',*,*,#20560,.T.);
#28483=ORIENTED_EDGE('',*,*,#20557,.T.);
#28484=ORIENTED_EDGE('',*,*,#20261,.F.);
#28485=ORIENTED_EDGE('',*,*,#20564,.F.);
#28486=ORIENTED_EDGE('',*,*,#20565,.F.);
#28487=ORIENTED_EDGE('',*,*,#20566,.T.);
#28488=ORIENTED_EDGE('',*,*,#20564,.T.);
#28489=ORIENTED_EDGE('',*,*,#20566,.F.);
#28490=ORIENTED_EDGE('',*,*,#20567,.T.);
#28491=ORIENTED_EDGE('',*,*,#20499,.F.);
#28492=ORIENTED_EDGE('',*,*,#20568,.T.);
#28493=ORIENTED_EDGE('',*,*,#20565,.T.);
#28494=ORIENTED_EDGE('',*,*,#20568,.F.);
#28495=ORIENTED_EDGE('',*,*,#20498,.F.);
#28496=ORIENTED_EDGE('',*,*,#20532,.F.);
#28497=ORIENTED_EDGE('',*,*,#20497,.F.);
#28498=ORIENTED_EDGE('',*,*,#20257,.F.);
#28499=ORIENTED_EDGE('',*,*,#20569,.T.);
#28500=ORIENTED_EDGE('',*,*,#20494,.T.);
#28501=ORIENTED_EDGE('',*,*,#20528,.T.);
#28502=ORIENTED_EDGE('',*,*,#20522,.T.);
#28503=ORIENTED_EDGE('',*,*,#20529,.T.);
#28504=ORIENTED_EDGE('',*,*,#20495,.T.);
#28505=ORIENTED_EDGE('',*,*,#20569,.F.);
#28506=ORIENTED_EDGE('',*,*,#20496,.T.);
#28507=ORIENTED_EDGE('',*,*,#20567,.F.);
#28508=ORIENTED_EDGE('',*,*,#20501,.T.);
#28509=ORIENTED_EDGE('',*,*,#20540,.T.);
#28510=ORIENTED_EDGE('',*,*,#20436,.T.);
#28511=ORIENTED_EDGE('',*,*,#20538,.T.);
#28512=ORIENTED_EDGE('',*,*,#20570,.T.);
#28513=ORIENTED_EDGE('',*,*,#20571,.T.);
#28514=ORIENTED_EDGE('',*,*,#20572,.T.);
#28515=ORIENTED_EDGE('',*,*,#20573,.T.);
#28516=ORIENTED_EDGE('',*,*,#20572,.F.);
#28517=ORIENTED_EDGE('',*,*,#20574,.T.);
#28518=ORIENTED_EDGE('',*,*,#20573,.F.);
#28519=ORIENTED_EDGE('',*,*,#20570,.F.);
#28520=ORIENTED_EDGE('',*,*,#20571,.F.);
#28521=ORIENTED_EDGE('',*,*,#20575,.T.);
#28522=ORIENTED_EDGE('',*,*,#20576,.F.);
#28523=ORIENTED_EDGE('',*,*,#20575,.F.);
#28524=ORIENTED_EDGE('',*,*,#20577,.T.);
#28525=ORIENTED_EDGE('',*,*,#20578,.T.);
#28526=ORIENTED_EDGE('',*,*,#20579,.T.);
#28527=ORIENTED_EDGE('',*,*,#20580,.T.);
#28528=ORIENTED_EDGE('',*,*,#20578,.F.);
#28529=ORIENTED_EDGE('',*,*,#20581,.F.);
#28530=ORIENTED_EDGE('',*,*,#20577,.F.);
#28531=ORIENTED_EDGE('',*,*,#20582,.T.);
#28532=ORIENTED_EDGE('',*,*,#20583,.T.);
#28533=ORIENTED_EDGE('',*,*,#20579,.F.);
#28534=ORIENTED_EDGE('',*,*,#20580,.F.);
#28535=ORIENTED_EDGE('',*,*,#20583,.F.);
#28536=ORIENTED_EDGE('',*,*,#20584,.F.);
#28537=ORIENTED_EDGE('',*,*,#20585,.T.);
#28538=ORIENTED_EDGE('',*,*,#20586,.F.);
#28539=ORIENTED_EDGE('',*,*,#20585,.F.);
#28540=ORIENTED_EDGE('',*,*,#20586,.T.);
#28541=ORIENTED_EDGE('',*,*,#20587,.T.);
#28542=ORIENTED_EDGE('',*,*,#20588,.F.);
#28543=ORIENTED_EDGE('',*,*,#20589,.T.);
#28544=ORIENTED_EDGE('',*,*,#20581,.T.);
#28545=ORIENTED_EDGE('',*,*,#20589,.F.);
#28546=ORIENTED_EDGE('',*,*,#20590,.F.);
#28547=ORIENTED_EDGE('',*,*,#20591,.T.);
#28548=ORIENTED_EDGE('',*,*,#20588,.T.);
#28549=ORIENTED_EDGE('',*,*,#20591,.F.);
#28550=ORIENTED_EDGE('',*,*,#20574,.F.);
#28551=ORIENTED_EDGE('',*,*,#20592,.T.);
#28552=ORIENTED_EDGE('',*,*,#20590,.T.);
#28553=ORIENTED_EDGE('',*,*,#20592,.F.);
#28554=ORIENTED_EDGE('',*,*,#20576,.T.);
#28555=ORIENTED_EDGE('',*,*,#20593,.T.);
#28556=ORIENTED_EDGE('',*,*,#20594,.F.);
#28557=ORIENTED_EDGE('',*,*,#20593,.F.);
#28558=ORIENTED_EDGE('',*,*,#20594,.T.);
#28559=ORIENTED_EDGE('',*,*,#20595,.T.);
#28560=ORIENTED_EDGE('',*,*,#20596,.F.);
#28561=ORIENTED_EDGE('',*,*,#20595,.F.);
#28562=ORIENTED_EDGE('',*,*,#20596,.T.);
#28563=ORIENTED_EDGE('',*,*,#20597,.T.);
#28564=ORIENTED_EDGE('',*,*,#20598,.F.);
#28565=ORIENTED_EDGE('',*,*,#20597,.F.);
#28566=ORIENTED_EDGE('',*,*,#20598,.T.);
#28567=ORIENTED_EDGE('',*,*,#20599,.T.);
#28568=ORIENTED_EDGE('',*,*,#20587,.F.);
#28569=ORIENTED_EDGE('',*,*,#20599,.F.);
#28570=ORIENTED_EDGE('',*,*,#20582,.F.);
#28571=ORIENTED_EDGE('',*,*,#20584,.T.);
#28572=ORIENTED_EDGE('',*,*,#20600,.F.);
#28573=ORIENTED_EDGE('',*,*,#20601,.T.);
#28574=ORIENTED_EDGE('',*,*,#20602,.T.);
#28575=ORIENTED_EDGE('',*,*,#20601,.F.);
#28576=ORIENTED_EDGE('',*,*,#20603,.F.);
#28577=ORIENTED_EDGE('',*,*,#20604,.T.);
#28578=ORIENTED_EDGE('',*,*,#20600,.T.);
#28579=ORIENTED_EDGE('',*,*,#20604,.F.);
#28580=ORIENTED_EDGE('',*,*,#20605,.F.);
#28581=ORIENTED_EDGE('',*,*,#20606,.T.);
#28582=ORIENTED_EDGE('',*,*,#20603,.T.);
#28583=ORIENTED_EDGE('',*,*,#20606,.F.);
#28584=ORIENTED_EDGE('',*,*,#20605,.T.);
#28585=ORIENTED_EDGE('',*,*,#20607,.F.);
#28586=ORIENTED_EDGE('',*,*,#20607,.T.);
#28587=ORIENTED_EDGE('',*,*,#20608,.T.);
#28588=ORIENTED_EDGE('',*,*,#20609,.F.);
#28589=ORIENTED_EDGE('',*,*,#20608,.F.);
#28590=ORIENTED_EDGE('',*,*,#20609,.T.);
#28591=ORIENTED_EDGE('',*,*,#20610,.T.);
#28592=ORIENTED_EDGE('',*,*,#20611,.F.);
#28593=ORIENTED_EDGE('',*,*,#20610,.F.);
#28594=ORIENTED_EDGE('',*,*,#20611,.T.);
#28595=ORIENTED_EDGE('',*,*,#20612,.T.);
#28596=ORIENTED_EDGE('',*,*,#20613,.F.);
#28597=ORIENTED_EDGE('',*,*,#20612,.F.);
#28598=ORIENTED_EDGE('',*,*,#20602,.F.);
#28599=ORIENTED_EDGE('',*,*,#20613,.T.);
#28600=ORIENTED_EDGE('',*,*,#20614,.T.);
#28601=ORIENTED_EDGE('',*,*,#20615,.T.);
#28602=ORIENTED_EDGE('',*,*,#20616,.T.);
#28603=ORIENTED_EDGE('',*,*,#20617,.T.);
#28604=ORIENTED_EDGE('',*,*,#20616,.F.);
#28605=ORIENTED_EDGE('',*,*,#20617,.F.);
#28606=ORIENTED_EDGE('',*,*,#20618,.T.);
#28607=ORIENTED_EDGE('',*,*,#20619,.F.);
#28608=ORIENTED_EDGE('',*,*,#20620,.T.);
#28609=ORIENTED_EDGE('',*,*,#20614,.F.);
#28610=ORIENTED_EDGE('',*,*,#20615,.F.);
#28611=ORIENTED_EDGE('',*,*,#20620,.F.);
#28612=ORIENTED_EDGE('',*,*,#20621,.T.);
#28613=ORIENTED_EDGE('',*,*,#20622,.T.);
#28614=ORIENTED_EDGE('',*,*,#20623,.T.);
#28615=ORIENTED_EDGE('',*,*,#20624,.T.);
#28616=ORIENTED_EDGE('',*,*,#20622,.F.);
#28617=ORIENTED_EDGE('',*,*,#20623,.F.);
#28618=ORIENTED_EDGE('',*,*,#20624,.F.);
#28619=ORIENTED_EDGE('',*,*,#20625,.T.);
#28620=ORIENTED_EDGE('',*,*,#20626,.T.);
#28621=ORIENTED_EDGE('',*,*,#20625,.F.);
#28622=ORIENTED_EDGE('',*,*,#20621,.F.);
#28623=ORIENTED_EDGE('',*,*,#20627,.F.);
#28624=ORIENTED_EDGE('',*,*,#20628,.F.);
#28625=ORIENTED_EDGE('',*,*,#20629,.T.);
#28626=ORIENTED_EDGE('',*,*,#20630,.T.);
#28627=ORIENTED_EDGE('',*,*,#20631,.T.);
#28628=ORIENTED_EDGE('',*,*,#20630,.F.);
#28629=ORIENTED_EDGE('',*,*,#20632,.T.);
#28630=ORIENTED_EDGE('',*,*,#20633,.F.);
#28631=ORIENTED_EDGE('',*,*,#20634,.F.);
#28632=ORIENTED_EDGE('',*,*,#20635,.F.);
#28633=ORIENTED_EDGE('',*,*,#20636,.F.);
#28634=ORIENTED_EDGE('',*,*,#20632,.F.);
#28635=ORIENTED_EDGE('',*,*,#20629,.F.);
#28636=ORIENTED_EDGE('',*,*,#20637,.T.);
#28637=ORIENTED_EDGE('',*,*,#20638,.T.);
#28638=ORIENTED_EDGE('',*,*,#20634,.T.);
#28639=ORIENTED_EDGE('',*,*,#20639,.F.);
#28640=ORIENTED_EDGE('',*,*,#20635,.T.);
#28641=ORIENTED_EDGE('',*,*,#20638,.F.);
#28642=ORIENTED_EDGE('',*,*,#20637,.F.);
#28643=ORIENTED_EDGE('',*,*,#20631,.F.);
#28644=ORIENTED_EDGE('',*,*,#20640,.F.);
#28645=ORIENTED_EDGE('',*,*,#20641,.T.);
#28646=ORIENTED_EDGE('',*,*,#20642,.T.);
#28647=ORIENTED_EDGE('',*,*,#20643,.T.);
#28648=ORIENTED_EDGE('',*,*,#20642,.F.);
#28649=ORIENTED_EDGE('',*,*,#20644,.T.);
#28650=ORIENTED_EDGE('',*,*,#20645,.F.);
#28651=ORIENTED_EDGE('',*,*,#20646,.F.);
#28652=ORIENTED_EDGE('',*,*,#20647,.F.);
#28653=ORIENTED_EDGE('',*,*,#20648,.F.);
#28654=ORIENTED_EDGE('',*,*,#20644,.F.);
#28655=ORIENTED_EDGE('',*,*,#20641,.F.);
#28656=ORIENTED_EDGE('',*,*,#20649,.T.);
#28657=ORIENTED_EDGE('',*,*,#20650,.T.);
#28658=ORIENTED_EDGE('',*,*,#20646,.T.);
#28659=ORIENTED_EDGE('',*,*,#20651,.F.);
#28660=ORIENTED_EDGE('',*,*,#20647,.T.);
#28661=ORIENTED_EDGE('',*,*,#20650,.F.);
#28662=ORIENTED_EDGE('',*,*,#20649,.F.);
#28663=ORIENTED_EDGE('',*,*,#20643,.F.);
#28664=ORIENTED_EDGE('',*,*,#20652,.F.);
#28665=ORIENTED_EDGE('',*,*,#20653,.T.);
#28666=ORIENTED_EDGE('',*,*,#20654,.T.);
#28667=ORIENTED_EDGE('',*,*,#20655,.T.);
#28668=ORIENTED_EDGE('',*,*,#20654,.F.);
#28669=ORIENTED_EDGE('',*,*,#20656,.T.);
#28670=ORIENTED_EDGE('',*,*,#20657,.F.);
#28671=ORIENTED_EDGE('',*,*,#20658,.F.);
#28672=ORIENTED_EDGE('',*,*,#20659,.F.);
#28673=ORIENTED_EDGE('',*,*,#20660,.F.);
#28674=ORIENTED_EDGE('',*,*,#20656,.F.);
#28675=ORIENTED_EDGE('',*,*,#20653,.F.);
#28676=ORIENTED_EDGE('',*,*,#20661,.T.);
#28677=ORIENTED_EDGE('',*,*,#20662,.T.);
#28678=ORIENTED_EDGE('',*,*,#20658,.T.);
#28679=ORIENTED_EDGE('',*,*,#20663,.F.);
#28680=ORIENTED_EDGE('',*,*,#20659,.T.);
#28681=ORIENTED_EDGE('',*,*,#20662,.F.);
#28682=ORIENTED_EDGE('',*,*,#20661,.F.);
#28683=ORIENTED_EDGE('',*,*,#20655,.F.);
#28684=ORIENTED_EDGE('',*,*,#20664,.F.);
#28685=ORIENTED_EDGE('',*,*,#20665,.T.);
#28686=ORIENTED_EDGE('',*,*,#20666,.T.);
#28687=ORIENTED_EDGE('',*,*,#20667,.T.);
#28688=ORIENTED_EDGE('',*,*,#20666,.F.);
#28689=ORIENTED_EDGE('',*,*,#20668,.T.);
#28690=ORIENTED_EDGE('',*,*,#20669,.F.);
#28691=ORIENTED_EDGE('',*,*,#20670,.F.);
#28692=ORIENTED_EDGE('',*,*,#20671,.F.);
#28693=ORIENTED_EDGE('',*,*,#20672,.F.);
#28694=ORIENTED_EDGE('',*,*,#20668,.F.);
#28695=ORIENTED_EDGE('',*,*,#20665,.F.);
#28696=ORIENTED_EDGE('',*,*,#20673,.T.);
#28697=ORIENTED_EDGE('',*,*,#20674,.T.);
#28698=ORIENTED_EDGE('',*,*,#20670,.T.);
#28699=ORIENTED_EDGE('',*,*,#20675,.F.);
#28700=ORIENTED_EDGE('',*,*,#20671,.T.);
#28701=ORIENTED_EDGE('',*,*,#20674,.F.);
#28702=ORIENTED_EDGE('',*,*,#20673,.F.);
#28703=ORIENTED_EDGE('',*,*,#20667,.F.);
#28704=ORIENTED_EDGE('',*,*,#20676,.F.);
#28705=ORIENTED_EDGE('',*,*,#20677,.T.);
#28706=ORIENTED_EDGE('',*,*,#20678,.T.);
#28707=ORIENTED_EDGE('',*,*,#20679,.T.);
#28708=ORIENTED_EDGE('',*,*,#20678,.F.);
#28709=ORIENTED_EDGE('',*,*,#20680,.T.);
#28710=ORIENTED_EDGE('',*,*,#20681,.F.);
#28711=ORIENTED_EDGE('',*,*,#20682,.F.);
#28712=ORIENTED_EDGE('',*,*,#20683,.F.);
#28713=ORIENTED_EDGE('',*,*,#20684,.F.);
#28714=ORIENTED_EDGE('',*,*,#20680,.F.);
#28715=ORIENTED_EDGE('',*,*,#20677,.F.);
#28716=ORIENTED_EDGE('',*,*,#20685,.T.);
#28717=ORIENTED_EDGE('',*,*,#20686,.T.);
#28718=ORIENTED_EDGE('',*,*,#20682,.T.);
#28719=ORIENTED_EDGE('',*,*,#20687,.F.);
#28720=ORIENTED_EDGE('',*,*,#20683,.T.);
#28721=ORIENTED_EDGE('',*,*,#20686,.F.);
#28722=ORIENTED_EDGE('',*,*,#20685,.F.);
#28723=ORIENTED_EDGE('',*,*,#20679,.F.);
#28724=ORIENTED_EDGE('',*,*,#20688,.F.);
#28725=ORIENTED_EDGE('',*,*,#20689,.T.);
#28726=ORIENTED_EDGE('',*,*,#20690,.T.);
#28727=ORIENTED_EDGE('',*,*,#20691,.T.);
#28728=ORIENTED_EDGE('',*,*,#20690,.F.);
#28729=ORIENTED_EDGE('',*,*,#20692,.T.);
#28730=ORIENTED_EDGE('',*,*,#20693,.F.);
#28731=ORIENTED_EDGE('',*,*,#20694,.F.);
#28732=ORIENTED_EDGE('',*,*,#20695,.F.);
#28733=ORIENTED_EDGE('',*,*,#20696,.F.);
#28734=ORIENTED_EDGE('',*,*,#20692,.F.);
#28735=ORIENTED_EDGE('',*,*,#20689,.F.);
#28736=ORIENTED_EDGE('',*,*,#20697,.T.);
#28737=ORIENTED_EDGE('',*,*,#20698,.T.);
#28738=ORIENTED_EDGE('',*,*,#20694,.T.);
#28739=ORIENTED_EDGE('',*,*,#20699,.F.);
#28740=ORIENTED_EDGE('',*,*,#20695,.T.);
#28741=ORIENTED_EDGE('',*,*,#20698,.F.);
#28742=ORIENTED_EDGE('',*,*,#20697,.F.);
#28743=ORIENTED_EDGE('',*,*,#20691,.F.);
#28744=ORIENTED_EDGE('',*,*,#20700,.F.);
#28745=ORIENTED_EDGE('',*,*,#20701,.T.);
#28746=ORIENTED_EDGE('',*,*,#20702,.T.);
#28747=ORIENTED_EDGE('',*,*,#20703,.T.);
#28748=ORIENTED_EDGE('',*,*,#20702,.F.);
#28749=ORIENTED_EDGE('',*,*,#20704,.T.);
#28750=ORIENTED_EDGE('',*,*,#20705,.F.);
#28751=ORIENTED_EDGE('',*,*,#20706,.F.);
#28752=ORIENTED_EDGE('',*,*,#20707,.F.);
#28753=ORIENTED_EDGE('',*,*,#20708,.F.);
#28754=ORIENTED_EDGE('',*,*,#20704,.F.);
#28755=ORIENTED_EDGE('',*,*,#20701,.F.);
#28756=ORIENTED_EDGE('',*,*,#20709,.T.);
#28757=ORIENTED_EDGE('',*,*,#20710,.T.);
#28758=ORIENTED_EDGE('',*,*,#20706,.T.);
#28759=ORIENTED_EDGE('',*,*,#20711,.F.);
#28760=ORIENTED_EDGE('',*,*,#20707,.T.);
#28761=ORIENTED_EDGE('',*,*,#20710,.F.);
#28762=ORIENTED_EDGE('',*,*,#20709,.F.);
#28763=ORIENTED_EDGE('',*,*,#20703,.F.);
#28764=ORIENTED_EDGE('',*,*,#20712,.F.);
#28765=ORIENTED_EDGE('',*,*,#20713,.T.);
#28766=ORIENTED_EDGE('',*,*,#20714,.T.);
#28767=ORIENTED_EDGE('',*,*,#20715,.T.);
#28768=ORIENTED_EDGE('',*,*,#20714,.F.);
#28769=ORIENTED_EDGE('',*,*,#20716,.T.);
#28770=ORIENTED_EDGE('',*,*,#20717,.F.);
#28771=ORIENTED_EDGE('',*,*,#20718,.F.);
#28772=ORIENTED_EDGE('',*,*,#20719,.F.);
#28773=ORIENTED_EDGE('',*,*,#20720,.F.);
#28774=ORIENTED_EDGE('',*,*,#20716,.F.);
#28775=ORIENTED_EDGE('',*,*,#20713,.F.);
#28776=ORIENTED_EDGE('',*,*,#20721,.T.);
#28777=ORIENTED_EDGE('',*,*,#20722,.T.);
#28778=ORIENTED_EDGE('',*,*,#20718,.T.);
#28779=ORIENTED_EDGE('',*,*,#20723,.F.);
#28780=ORIENTED_EDGE('',*,*,#20719,.T.);
#28781=ORIENTED_EDGE('',*,*,#20722,.F.);
#28782=ORIENTED_EDGE('',*,*,#20721,.F.);
#28783=ORIENTED_EDGE('',*,*,#20715,.F.);
#28784=ORIENTED_EDGE('',*,*,#20724,.F.);
#28785=ORIENTED_EDGE('',*,*,#20725,.T.);
#28786=ORIENTED_EDGE('',*,*,#20726,.T.);
#28787=ORIENTED_EDGE('',*,*,#20727,.T.);
#28788=ORIENTED_EDGE('',*,*,#20726,.F.);
#28789=ORIENTED_EDGE('',*,*,#20728,.T.);
#28790=ORIENTED_EDGE('',*,*,#20729,.F.);
#28791=ORIENTED_EDGE('',*,*,#20730,.F.);
#28792=ORIENTED_EDGE('',*,*,#20731,.F.);
#28793=ORIENTED_EDGE('',*,*,#20732,.F.);
#28794=ORIENTED_EDGE('',*,*,#20728,.F.);
#28795=ORIENTED_EDGE('',*,*,#20725,.F.);
#28796=ORIENTED_EDGE('',*,*,#20733,.T.);
#28797=ORIENTED_EDGE('',*,*,#20734,.T.);
#28798=ORIENTED_EDGE('',*,*,#20730,.T.);
#28799=ORIENTED_EDGE('',*,*,#20735,.F.);
#28800=ORIENTED_EDGE('',*,*,#20731,.T.);
#28801=ORIENTED_EDGE('',*,*,#20734,.F.);
#28802=ORIENTED_EDGE('',*,*,#20733,.F.);
#28803=ORIENTED_EDGE('',*,*,#20727,.F.);
#28804=ORIENTED_EDGE('',*,*,#20736,.F.);
#28805=ORIENTED_EDGE('',*,*,#20737,.T.);
#28806=ORIENTED_EDGE('',*,*,#20738,.T.);
#28807=ORIENTED_EDGE('',*,*,#20739,.T.);
#28808=ORIENTED_EDGE('',*,*,#20738,.F.);
#28809=ORIENTED_EDGE('',*,*,#20740,.T.);
#28810=ORIENTED_EDGE('',*,*,#20741,.F.);
#28811=ORIENTED_EDGE('',*,*,#20742,.F.);
#28812=ORIENTED_EDGE('',*,*,#20743,.F.);
#28813=ORIENTED_EDGE('',*,*,#20744,.F.);
#28814=ORIENTED_EDGE('',*,*,#20740,.F.);
#28815=ORIENTED_EDGE('',*,*,#20737,.F.);
#28816=ORIENTED_EDGE('',*,*,#20745,.T.);
#28817=ORIENTED_EDGE('',*,*,#20746,.T.);
#28818=ORIENTED_EDGE('',*,*,#20742,.T.);
#28819=ORIENTED_EDGE('',*,*,#20747,.F.);
#28820=ORIENTED_EDGE('',*,*,#20743,.T.);
#28821=ORIENTED_EDGE('',*,*,#20746,.F.);
#28822=ORIENTED_EDGE('',*,*,#20745,.F.);
#28823=ORIENTED_EDGE('',*,*,#20739,.F.);
#28824=ORIENTED_EDGE('',*,*,#20748,.F.);
#28825=ORIENTED_EDGE('',*,*,#20749,.T.);
#28826=ORIENTED_EDGE('',*,*,#20750,.T.);
#28827=ORIENTED_EDGE('',*,*,#20751,.T.);
#28828=ORIENTED_EDGE('',*,*,#20750,.F.);
#28829=ORIENTED_EDGE('',*,*,#20752,.T.);
#28830=ORIENTED_EDGE('',*,*,#20753,.F.);
#28831=ORIENTED_EDGE('',*,*,#20754,.F.);
#28832=ORIENTED_EDGE('',*,*,#20755,.F.);
#28833=ORIENTED_EDGE('',*,*,#20756,.F.);
#28834=ORIENTED_EDGE('',*,*,#20757,.F.);
#28835=ORIENTED_EDGE('',*,*,#20752,.F.);
#28836=ORIENTED_EDGE('',*,*,#20749,.F.);
#28837=ORIENTED_EDGE('',*,*,#20758,.T.);
#28838=ORIENTED_EDGE('',*,*,#20759,.T.);
#28839=ORIENTED_EDGE('',*,*,#20755,.T.);
#28840=ORIENTED_EDGE('',*,*,#20760,.F.);
#28841=ORIENTED_EDGE('',*,*,#20761,.F.);
#28842=ORIENTED_EDGE('',*,*,#20756,.T.);
#28843=ORIENTED_EDGE('',*,*,#20759,.F.);
#28844=ORIENTED_EDGE('',*,*,#20758,.F.);
#28845=ORIENTED_EDGE('',*,*,#20751,.F.);
#28846=ORIENTED_EDGE('',*,*,#20762,.F.);
#28847=ORIENTED_EDGE('',*,*,#20763,.T.);
#28848=ORIENTED_EDGE('',*,*,#20764,.T.);
#28849=ORIENTED_EDGE('',*,*,#20765,.T.);
#28850=ORIENTED_EDGE('',*,*,#20764,.F.);
#28851=ORIENTED_EDGE('',*,*,#20766,.T.);
#28852=ORIENTED_EDGE('',*,*,#20767,.F.);
#28853=ORIENTED_EDGE('',*,*,#20768,.F.);
#28854=ORIENTED_EDGE('',*,*,#20769,.F.);
#28855=ORIENTED_EDGE('',*,*,#20770,.F.);
#28856=ORIENTED_EDGE('',*,*,#20766,.F.);
#28857=ORIENTED_EDGE('',*,*,#20763,.F.);
#28858=ORIENTED_EDGE('',*,*,#20771,.T.);
#28859=ORIENTED_EDGE('',*,*,#20772,.T.);
#28860=ORIENTED_EDGE('',*,*,#20768,.T.);
#28861=ORIENTED_EDGE('',*,*,#20773,.F.);
#28862=ORIENTED_EDGE('',*,*,#20769,.T.);
#28863=ORIENTED_EDGE('',*,*,#20772,.F.);
#28864=ORIENTED_EDGE('',*,*,#20771,.F.);
#28865=ORIENTED_EDGE('',*,*,#20765,.F.);
#28866=ORIENTED_EDGE('',*,*,#20774,.F.);
#28867=ORIENTED_EDGE('',*,*,#20775,.T.);
#28868=ORIENTED_EDGE('',*,*,#20776,.T.);
#28869=ORIENTED_EDGE('',*,*,#20777,.T.);
#28870=ORIENTED_EDGE('',*,*,#20776,.F.);
#28871=ORIENTED_EDGE('',*,*,#20778,.T.);
#28872=ORIENTED_EDGE('',*,*,#20779,.F.);
#28873=ORIENTED_EDGE('',*,*,#20780,.F.);
#28874=ORIENTED_EDGE('',*,*,#20781,.F.);
#28875=ORIENTED_EDGE('',*,*,#20782,.F.);
#28876=ORIENTED_EDGE('',*,*,#20778,.F.);
#28877=ORIENTED_EDGE('',*,*,#20775,.F.);
#28878=ORIENTED_EDGE('',*,*,#20783,.T.);
#28879=ORIENTED_EDGE('',*,*,#20784,.T.);
#28880=ORIENTED_EDGE('',*,*,#20780,.T.);
#28881=ORIENTED_EDGE('',*,*,#20785,.F.);
#28882=ORIENTED_EDGE('',*,*,#20781,.T.);
#28883=ORIENTED_EDGE('',*,*,#20784,.F.);
#28884=ORIENTED_EDGE('',*,*,#20783,.F.);
#28885=ORIENTED_EDGE('',*,*,#20777,.F.);
#28886=ORIENTED_EDGE('',*,*,#20786,.F.);
#28887=ORIENTED_EDGE('',*,*,#20787,.T.);
#28888=ORIENTED_EDGE('',*,*,#20788,.T.);
#28889=ORIENTED_EDGE('',*,*,#20789,.T.);
#28890=ORIENTED_EDGE('',*,*,#20788,.F.);
#28891=ORIENTED_EDGE('',*,*,#20790,.T.);
#28892=ORIENTED_EDGE('',*,*,#20791,.F.);
#28893=ORIENTED_EDGE('',*,*,#20792,.F.);
#28894=ORIENTED_EDGE('',*,*,#20793,.F.);
#28895=ORIENTED_EDGE('',*,*,#20794,.F.);
#28896=ORIENTED_EDGE('',*,*,#20790,.F.);
#28897=ORIENTED_EDGE('',*,*,#20787,.F.);
#28898=ORIENTED_EDGE('',*,*,#20795,.T.);
#28899=ORIENTED_EDGE('',*,*,#20796,.T.);
#28900=ORIENTED_EDGE('',*,*,#20792,.T.);
#28901=ORIENTED_EDGE('',*,*,#20797,.F.);
#28902=ORIENTED_EDGE('',*,*,#20793,.T.);
#28903=ORIENTED_EDGE('',*,*,#20796,.F.);
#28904=ORIENTED_EDGE('',*,*,#20795,.F.);
#28905=ORIENTED_EDGE('',*,*,#20789,.F.);
#28906=ORIENTED_EDGE('',*,*,#20798,.F.);
#28907=ORIENTED_EDGE('',*,*,#20799,.T.);
#28908=ORIENTED_EDGE('',*,*,#20800,.T.);
#28909=ORIENTED_EDGE('',*,*,#20801,.T.);
#28910=ORIENTED_EDGE('',*,*,#20800,.F.);
#28911=ORIENTED_EDGE('',*,*,#20802,.T.);
#28912=ORIENTED_EDGE('',*,*,#20803,.F.);
#28913=ORIENTED_EDGE('',*,*,#20804,.F.);
#28914=ORIENTED_EDGE('',*,*,#20805,.F.);
#28915=ORIENTED_EDGE('',*,*,#20806,.F.);
#28916=ORIENTED_EDGE('',*,*,#20802,.F.);
#28917=ORIENTED_EDGE('',*,*,#20799,.F.);
#28918=ORIENTED_EDGE('',*,*,#20807,.T.);
#28919=ORIENTED_EDGE('',*,*,#20808,.T.);
#28920=ORIENTED_EDGE('',*,*,#20804,.T.);
#28921=ORIENTED_EDGE('',*,*,#20809,.F.);
#28922=ORIENTED_EDGE('',*,*,#20805,.T.);
#28923=ORIENTED_EDGE('',*,*,#20808,.F.);
#28924=ORIENTED_EDGE('',*,*,#20807,.F.);
#28925=ORIENTED_EDGE('',*,*,#20801,.F.);
#28926=ORIENTED_EDGE('',*,*,#20810,.F.);
#28927=ORIENTED_EDGE('',*,*,#20811,.T.);
#28928=ORIENTED_EDGE('',*,*,#20812,.T.);
#28929=ORIENTED_EDGE('',*,*,#20813,.T.);
#28930=ORIENTED_EDGE('',*,*,#20812,.F.);
#28931=ORIENTED_EDGE('',*,*,#20814,.T.);
#28932=ORIENTED_EDGE('',*,*,#20815,.F.);
#28933=ORIENTED_EDGE('',*,*,#20816,.F.);
#28934=ORIENTED_EDGE('',*,*,#20817,.F.);
#28935=ORIENTED_EDGE('',*,*,#20818,.F.);
#28936=ORIENTED_EDGE('',*,*,#20814,.F.);
#28937=ORIENTED_EDGE('',*,*,#20811,.F.);
#28938=ORIENTED_EDGE('',*,*,#20819,.T.);
#28939=ORIENTED_EDGE('',*,*,#20820,.T.);
#28940=ORIENTED_EDGE('',*,*,#20816,.T.);
#28941=ORIENTED_EDGE('',*,*,#20821,.F.);
#28942=ORIENTED_EDGE('',*,*,#20817,.T.);
#28943=ORIENTED_EDGE('',*,*,#20820,.F.);
#28944=ORIENTED_EDGE('',*,*,#20819,.F.);
#28945=ORIENTED_EDGE('',*,*,#20813,.F.);
#28946=ORIENTED_EDGE('',*,*,#20822,.F.);
#28947=ORIENTED_EDGE('',*,*,#20823,.T.);
#28948=ORIENTED_EDGE('',*,*,#20824,.T.);
#28949=ORIENTED_EDGE('',*,*,#20825,.T.);
#28950=ORIENTED_EDGE('',*,*,#20824,.F.);
#28951=ORIENTED_EDGE('',*,*,#20826,.T.);
#28952=ORIENTED_EDGE('',*,*,#20827,.F.);
#28953=ORIENTED_EDGE('',*,*,#20828,.F.);
#28954=ORIENTED_EDGE('',*,*,#20829,.F.);
#28955=ORIENTED_EDGE('',*,*,#20830,.F.);
#28956=ORIENTED_EDGE('',*,*,#20826,.F.);
#28957=ORIENTED_EDGE('',*,*,#20823,.F.);
#28958=ORIENTED_EDGE('',*,*,#20831,.T.);
#28959=ORIENTED_EDGE('',*,*,#20832,.T.);
#28960=ORIENTED_EDGE('',*,*,#20828,.T.);
#28961=ORIENTED_EDGE('',*,*,#20833,.F.);
#28962=ORIENTED_EDGE('',*,*,#20829,.T.);
#28963=ORIENTED_EDGE('',*,*,#20832,.F.);
#28964=ORIENTED_EDGE('',*,*,#20831,.F.);
#28965=ORIENTED_EDGE('',*,*,#20825,.F.);
#28966=ORIENTED_EDGE('',*,*,#20834,.F.);
#28967=ORIENTED_EDGE('',*,*,#20835,.T.);
#28968=ORIENTED_EDGE('',*,*,#20836,.T.);
#28969=ORIENTED_EDGE('',*,*,#20837,.T.);
#28970=ORIENTED_EDGE('',*,*,#20836,.F.);
#28971=ORIENTED_EDGE('',*,*,#20838,.T.);
#28972=ORIENTED_EDGE('',*,*,#20839,.F.);
#28973=ORIENTED_EDGE('',*,*,#20840,.F.);
#28974=ORIENTED_EDGE('',*,*,#20841,.F.);
#28975=ORIENTED_EDGE('',*,*,#20842,.F.);
#28976=ORIENTED_EDGE('',*,*,#20838,.F.);
#28977=ORIENTED_EDGE('',*,*,#20835,.F.);
#28978=ORIENTED_EDGE('',*,*,#20843,.T.);
#28979=ORIENTED_EDGE('',*,*,#20844,.T.);
#28980=ORIENTED_EDGE('',*,*,#20840,.T.);
#28981=ORIENTED_EDGE('',*,*,#20845,.F.);
#28982=ORIENTED_EDGE('',*,*,#20841,.T.);
#28983=ORIENTED_EDGE('',*,*,#20844,.F.);
#28984=ORIENTED_EDGE('',*,*,#20843,.F.);
#28985=ORIENTED_EDGE('',*,*,#20837,.F.);
#28986=ORIENTED_EDGE('',*,*,#20846,.F.);
#28987=ORIENTED_EDGE('',*,*,#20847,.T.);
#28988=ORIENTED_EDGE('',*,*,#20848,.T.);
#28989=ORIENTED_EDGE('',*,*,#20849,.T.);
#28990=ORIENTED_EDGE('',*,*,#20848,.F.);
#28991=ORIENTED_EDGE('',*,*,#20850,.T.);
#28992=ORIENTED_EDGE('',*,*,#20851,.F.);
#28993=ORIENTED_EDGE('',*,*,#20852,.F.);
#28994=ORIENTED_EDGE('',*,*,#20853,.F.);
#28995=ORIENTED_EDGE('',*,*,#20854,.F.);
#28996=ORIENTED_EDGE('',*,*,#20850,.F.);
#28997=ORIENTED_EDGE('',*,*,#20847,.F.);
#28998=ORIENTED_EDGE('',*,*,#20855,.T.);
#28999=ORIENTED_EDGE('',*,*,#20856,.T.);
#29000=ORIENTED_EDGE('',*,*,#20852,.T.);
#29001=ORIENTED_EDGE('',*,*,#20857,.F.);
#29002=ORIENTED_EDGE('',*,*,#20853,.T.);
#29003=ORIENTED_EDGE('',*,*,#20856,.F.);
#29004=ORIENTED_EDGE('',*,*,#20855,.F.);
#29005=ORIENTED_EDGE('',*,*,#20849,.F.);
#29006=ORIENTED_EDGE('',*,*,#20858,.F.);
#29007=ORIENTED_EDGE('',*,*,#20859,.T.);
#29008=ORIENTED_EDGE('',*,*,#20860,.T.);
#29009=ORIENTED_EDGE('',*,*,#20861,.T.);
#29010=ORIENTED_EDGE('',*,*,#20860,.F.);
#29011=ORIENTED_EDGE('',*,*,#20862,.T.);
#29012=ORIENTED_EDGE('',*,*,#20863,.F.);
#29013=ORIENTED_EDGE('',*,*,#20864,.F.);
#29014=ORIENTED_EDGE('',*,*,#20865,.F.);
#29015=ORIENTED_EDGE('',*,*,#20866,.F.);
#29016=ORIENTED_EDGE('',*,*,#20862,.F.);
#29017=ORIENTED_EDGE('',*,*,#20859,.F.);
#29018=ORIENTED_EDGE('',*,*,#20867,.T.);
#29019=ORIENTED_EDGE('',*,*,#20868,.T.);
#29020=ORIENTED_EDGE('',*,*,#20864,.T.);
#29021=ORIENTED_EDGE('',*,*,#20869,.F.);
#29022=ORIENTED_EDGE('',*,*,#20865,.T.);
#29023=ORIENTED_EDGE('',*,*,#20868,.F.);
#29024=ORIENTED_EDGE('',*,*,#20867,.F.);
#29025=ORIENTED_EDGE('',*,*,#20861,.F.);
#29026=ORIENTED_EDGE('',*,*,#20870,.F.);
#29027=ORIENTED_EDGE('',*,*,#20871,.T.);
#29028=ORIENTED_EDGE('',*,*,#20872,.T.);
#29029=ORIENTED_EDGE('',*,*,#20873,.T.);
#29030=ORIENTED_EDGE('',*,*,#20872,.F.);
#29031=ORIENTED_EDGE('',*,*,#20874,.T.);
#29032=ORIENTED_EDGE('',*,*,#20875,.F.);
#29033=ORIENTED_EDGE('',*,*,#20876,.F.);
#29034=ORIENTED_EDGE('',*,*,#20877,.F.);
#29035=ORIENTED_EDGE('',*,*,#20878,.F.);
#29036=ORIENTED_EDGE('',*,*,#20874,.F.);
#29037=ORIENTED_EDGE('',*,*,#20871,.F.);
#29038=ORIENTED_EDGE('',*,*,#20879,.T.);
#29039=ORIENTED_EDGE('',*,*,#20880,.T.);
#29040=ORIENTED_EDGE('',*,*,#20876,.T.);
#29041=ORIENTED_EDGE('',*,*,#20881,.F.);
#29042=ORIENTED_EDGE('',*,*,#20877,.T.);
#29043=ORIENTED_EDGE('',*,*,#20880,.F.);
#29044=ORIENTED_EDGE('',*,*,#20879,.F.);
#29045=ORIENTED_EDGE('',*,*,#20873,.F.);
#29046=ORIENTED_EDGE('',*,*,#20882,.F.);
#29047=ORIENTED_EDGE('',*,*,#20883,.T.);
#29048=ORIENTED_EDGE('',*,*,#20884,.T.);
#29049=ORIENTED_EDGE('',*,*,#20885,.T.);
#29050=ORIENTED_EDGE('',*,*,#20884,.F.);
#29051=ORIENTED_EDGE('',*,*,#20886,.T.);
#29052=ORIENTED_EDGE('',*,*,#20887,.F.);
#29053=ORIENTED_EDGE('',*,*,#20888,.F.);
#29054=ORIENTED_EDGE('',*,*,#20889,.F.);
#29055=ORIENTED_EDGE('',*,*,#20890,.F.);
#29056=ORIENTED_EDGE('',*,*,#20886,.F.);
#29057=ORIENTED_EDGE('',*,*,#20883,.F.);
#29058=ORIENTED_EDGE('',*,*,#20891,.T.);
#29059=ORIENTED_EDGE('',*,*,#20892,.T.);
#29060=ORIENTED_EDGE('',*,*,#20888,.T.);
#29061=ORIENTED_EDGE('',*,*,#20893,.F.);
#29062=ORIENTED_EDGE('',*,*,#20889,.T.);
#29063=ORIENTED_EDGE('',*,*,#20892,.F.);
#29064=ORIENTED_EDGE('',*,*,#20891,.F.);
#29065=ORIENTED_EDGE('',*,*,#20885,.F.);
#29066=ORIENTED_EDGE('',*,*,#20626,.F.);
#29067=ORIENTED_EDGE('',*,*,#20894,.T.);
#29068=ORIENTED_EDGE('',*,*,#20895,.T.);
#29069=ORIENTED_EDGE('',*,*,#20894,.F.);
#29070=ORIENTED_EDGE('',*,*,#20618,.F.);
#29071=ORIENTED_EDGE('',*,*,#20896,.T.);
#29072=ORIENTED_EDGE('',*,*,#20760,.T.);
#29073=ORIENTED_EDGE('',*,*,#20754,.T.);
#29074=ORIENTED_EDGE('',*,*,#20748,.T.);
#29075=ORIENTED_EDGE('',*,*,#20897,.T.);
#29076=ORIENTED_EDGE('',*,*,#20627,.T.);
#29077=ORIENTED_EDGE('',*,*,#20897,.F.);
#29078=ORIENTED_EDGE('',*,*,#20753,.T.);
#29079=ORIENTED_EDGE('',*,*,#20757,.T.);
#29080=ORIENTED_EDGE('',*,*,#20761,.T.);
#29081=ORIENTED_EDGE('',*,*,#20896,.F.);
#29082=ORIENTED_EDGE('',*,*,#20639,.T.);
#29083=ORIENTED_EDGE('',*,*,#20633,.T.);
#29084=ORIENTED_EDGE('',*,*,#20628,.T.);
#29085=ORIENTED_EDGE('',*,*,#20636,.T.);
#29086=ORIENTED_EDGE('',*,*,#20651,.T.);
#29087=ORIENTED_EDGE('',*,*,#20645,.T.);
#29088=ORIENTED_EDGE('',*,*,#20640,.T.);
#29089=ORIENTED_EDGE('',*,*,#20648,.T.);
#29090=ORIENTED_EDGE('',*,*,#20663,.T.);
#29091=ORIENTED_EDGE('',*,*,#20657,.T.);
#29092=ORIENTED_EDGE('',*,*,#20652,.T.);
#29093=ORIENTED_EDGE('',*,*,#20660,.T.);
#29094=ORIENTED_EDGE('',*,*,#20675,.T.);
#29095=ORIENTED_EDGE('',*,*,#20669,.T.);
#29096=ORIENTED_EDGE('',*,*,#20664,.T.);
#29097=ORIENTED_EDGE('',*,*,#20672,.T.);
#29098=ORIENTED_EDGE('',*,*,#20687,.T.);
#29099=ORIENTED_EDGE('',*,*,#20681,.T.);
#29100=ORIENTED_EDGE('',*,*,#20676,.T.);
#29101=ORIENTED_EDGE('',*,*,#20684,.T.);
#29102=ORIENTED_EDGE('',*,*,#20699,.T.);
#29103=ORIENTED_EDGE('',*,*,#20693,.T.);
#29104=ORIENTED_EDGE('',*,*,#20688,.T.);
#29105=ORIENTED_EDGE('',*,*,#20696,.T.);
#29106=ORIENTED_EDGE('',*,*,#20711,.T.);
#29107=ORIENTED_EDGE('',*,*,#20705,.T.);
#29108=ORIENTED_EDGE('',*,*,#20700,.T.);
#29109=ORIENTED_EDGE('',*,*,#20708,.T.);
#29110=ORIENTED_EDGE('',*,*,#20723,.T.);
#29111=ORIENTED_EDGE('',*,*,#20717,.T.);
#29112=ORIENTED_EDGE('',*,*,#20712,.T.);
#29113=ORIENTED_EDGE('',*,*,#20720,.T.);
#29114=ORIENTED_EDGE('',*,*,#20735,.T.);
#29115=ORIENTED_EDGE('',*,*,#20729,.T.);
#29116=ORIENTED_EDGE('',*,*,#20724,.T.);
#29117=ORIENTED_EDGE('',*,*,#20732,.T.);
#29118=ORIENTED_EDGE('',*,*,#20747,.T.);
#29119=ORIENTED_EDGE('',*,*,#20741,.T.);
#29120=ORIENTED_EDGE('',*,*,#20736,.T.);
#29121=ORIENTED_EDGE('',*,*,#20744,.T.);
#29122=ORIENTED_EDGE('',*,*,#20773,.T.);
#29123=ORIENTED_EDGE('',*,*,#20767,.T.);
#29124=ORIENTED_EDGE('',*,*,#20762,.T.);
#29125=ORIENTED_EDGE('',*,*,#20770,.T.);
#29126=ORIENTED_EDGE('',*,*,#20785,.T.);
#29127=ORIENTED_EDGE('',*,*,#20779,.T.);
#29128=ORIENTED_EDGE('',*,*,#20774,.T.);
#29129=ORIENTED_EDGE('',*,*,#20782,.T.);
#29130=ORIENTED_EDGE('',*,*,#20797,.T.);
#29131=ORIENTED_EDGE('',*,*,#20791,.T.);
#29132=ORIENTED_EDGE('',*,*,#20786,.T.);
#29133=ORIENTED_EDGE('',*,*,#20794,.T.);
#29134=ORIENTED_EDGE('',*,*,#20809,.T.);
#29135=ORIENTED_EDGE('',*,*,#20803,.T.);
#29136=ORIENTED_EDGE('',*,*,#20798,.T.);
#29137=ORIENTED_EDGE('',*,*,#20806,.T.);
#29138=ORIENTED_EDGE('',*,*,#20821,.T.);
#29139=ORIENTED_EDGE('',*,*,#20815,.T.);
#29140=ORIENTED_EDGE('',*,*,#20810,.T.);
#29141=ORIENTED_EDGE('',*,*,#20818,.T.);
#29142=ORIENTED_EDGE('',*,*,#20833,.T.);
#29143=ORIENTED_EDGE('',*,*,#20827,.T.);
#29144=ORIENTED_EDGE('',*,*,#20822,.T.);
#29145=ORIENTED_EDGE('',*,*,#20830,.T.);
#29146=ORIENTED_EDGE('',*,*,#20845,.T.);
#29147=ORIENTED_EDGE('',*,*,#20839,.T.);
#29148=ORIENTED_EDGE('',*,*,#20834,.T.);
#29149=ORIENTED_EDGE('',*,*,#20842,.T.);
#29150=ORIENTED_EDGE('',*,*,#20857,.T.);
#29151=ORIENTED_EDGE('',*,*,#20851,.T.);
#29152=ORIENTED_EDGE('',*,*,#20846,.T.);
#29153=ORIENTED_EDGE('',*,*,#20854,.T.);
#29154=ORIENTED_EDGE('',*,*,#20869,.T.);
#29155=ORIENTED_EDGE('',*,*,#20863,.T.);
#29156=ORIENTED_EDGE('',*,*,#20858,.T.);
#29157=ORIENTED_EDGE('',*,*,#20866,.T.);
#29158=ORIENTED_EDGE('',*,*,#20881,.T.);
#29159=ORIENTED_EDGE('',*,*,#20875,.T.);
#29160=ORIENTED_EDGE('',*,*,#20870,.T.);
#29161=ORIENTED_EDGE('',*,*,#20878,.T.);
#29162=ORIENTED_EDGE('',*,*,#20893,.T.);
#29163=ORIENTED_EDGE('',*,*,#20887,.T.);
#29164=ORIENTED_EDGE('',*,*,#20882,.T.);
#29165=ORIENTED_EDGE('',*,*,#20890,.T.);
#29166=ORIENTED_EDGE('',*,*,#20898,.F.);
#29167=ORIENTED_EDGE('',*,*,#20899,.T.);
#29168=ORIENTED_EDGE('',*,*,#20619,.T.);
#29169=ORIENTED_EDGE('',*,*,#20899,.F.);
#29170=ORIENTED_EDGE('',*,*,#20898,.T.);
#29171=ORIENTED_EDGE('',*,*,#20900,.F.);
#29172=ORIENTED_EDGE('',*,*,#20900,.T.);
#29173=ORIENTED_EDGE('',*,*,#20901,.T.);
#29174=ORIENTED_EDGE('',*,*,#20902,.F.);
#29175=ORIENTED_EDGE('',*,*,#20901,.F.);
#29176=ORIENTED_EDGE('',*,*,#20902,.T.);
#29177=ORIENTED_EDGE('',*,*,#20903,.T.);
#29178=ORIENTED_EDGE('',*,*,#20904,.F.);
#29179=ORIENTED_EDGE('',*,*,#20903,.F.);
#29180=ORIENTED_EDGE('',*,*,#20904,.T.);
#29181=ORIENTED_EDGE('',*,*,#20905,.T.);
#29182=ORIENTED_EDGE('',*,*,#20906,.F.);
#29183=ORIENTED_EDGE('',*,*,#20905,.F.);
#29184=ORIENTED_EDGE('',*,*,#20895,.F.);
#29185=ORIENTED_EDGE('',*,*,#20906,.T.);
#29186=ORIENTED_EDGE('',*,*,#20907,.F.);
#29187=ORIENTED_EDGE('',*,*,#20908,.T.);
#29188=ORIENTED_EDGE('',*,*,#20909,.T.);
#29189=ORIENTED_EDGE('',*,*,#20908,.F.);
#29190=ORIENTED_EDGE('',*,*,#20910,.F.);
#29191=ORIENTED_EDGE('',*,*,#20911,.T.);
#29192=ORIENTED_EDGE('',*,*,#20907,.T.);
#29193=ORIENTED_EDGE('',*,*,#20911,.F.);
#29194=ORIENTED_EDGE('',*,*,#20912,.F.);
#29195=ORIENTED_EDGE('',*,*,#20913,.T.);
#29196=ORIENTED_EDGE('',*,*,#20910,.T.);
#29197=ORIENTED_EDGE('',*,*,#20913,.F.);
#29198=ORIENTED_EDGE('',*,*,#20912,.T.);
#29199=ORIENTED_EDGE('',*,*,#20914,.F.);
#29200=ORIENTED_EDGE('',*,*,#20914,.T.);
#29201=ORIENTED_EDGE('',*,*,#20915,.T.);
#29202=ORIENTED_EDGE('',*,*,#20916,.F.);
#29203=ORIENTED_EDGE('',*,*,#20915,.F.);
#29204=ORIENTED_EDGE('',*,*,#20916,.T.);
#29205=ORIENTED_EDGE('',*,*,#20917,.T.);
#29206=ORIENTED_EDGE('',*,*,#20918,.F.);
#29207=ORIENTED_EDGE('',*,*,#20917,.F.);
#29208=ORIENTED_EDGE('',*,*,#20918,.T.);
#29209=ORIENTED_EDGE('',*,*,#20919,.T.);
#29210=ORIENTED_EDGE('',*,*,#20920,.F.);
#29211=ORIENTED_EDGE('',*,*,#20919,.F.);
#29212=ORIENTED_EDGE('',*,*,#20909,.F.);
#29213=ORIENTED_EDGE('',*,*,#20920,.T.);
#29214=ORIENTED_EDGE('',*,*,#20921,.T.);
#29215=ORIENTED_EDGE('',*,*,#20922,.T.);
#29216=ORIENTED_EDGE('',*,*,#20923,.T.);
#29217=ORIENTED_EDGE('',*,*,#20924,.T.);
#29218=ORIENTED_EDGE('',*,*,#20923,.F.);
#29219=ORIENTED_EDGE('',*,*,#20924,.F.);
#29220=ORIENTED_EDGE('',*,*,#20925,.T.);
#29221=ORIENTED_EDGE('',*,*,#20926,.F.);
#29222=ORIENTED_EDGE('',*,*,#20927,.T.);
#29223=ORIENTED_EDGE('',*,*,#20921,.F.);
#29224=ORIENTED_EDGE('',*,*,#20922,.F.);
#29225=ORIENTED_EDGE('',*,*,#20927,.F.);
#29226=ORIENTED_EDGE('',*,*,#20928,.T.);
#29227=ORIENTED_EDGE('',*,*,#20929,.T.);
#29228=ORIENTED_EDGE('',*,*,#20930,.T.);
#29229=ORIENTED_EDGE('',*,*,#20931,.T.);
#29230=ORIENTED_EDGE('',*,*,#20929,.F.);
#29231=ORIENTED_EDGE('',*,*,#20930,.F.);
#29232=ORIENTED_EDGE('',*,*,#20931,.F.);
#29233=ORIENTED_EDGE('',*,*,#20932,.T.);
#29234=ORIENTED_EDGE('',*,*,#20933,.T.);
#29235=ORIENTED_EDGE('',*,*,#20932,.F.);
#29236=ORIENTED_EDGE('',*,*,#20928,.F.);
#29237=ORIENTED_EDGE('',*,*,#20934,.F.);
#29238=ORIENTED_EDGE('',*,*,#20935,.F.);
#29239=ORIENTED_EDGE('',*,*,#20936,.T.);
#29240=ORIENTED_EDGE('',*,*,#20937,.T.);
#29241=ORIENTED_EDGE('',*,*,#20938,.T.);
#29242=ORIENTED_EDGE('',*,*,#20937,.F.);
#29243=ORIENTED_EDGE('',*,*,#20939,.T.);
#29244=ORIENTED_EDGE('',*,*,#20940,.F.);
#29245=ORIENTED_EDGE('',*,*,#20941,.F.);
#29246=ORIENTED_EDGE('',*,*,#20942,.F.);
#29247=ORIENTED_EDGE('',*,*,#20943,.F.);
#29248=ORIENTED_EDGE('',*,*,#20939,.F.);
#29249=ORIENTED_EDGE('',*,*,#20936,.F.);
#29250=ORIENTED_EDGE('',*,*,#20944,.T.);
#29251=ORIENTED_EDGE('',*,*,#20945,.T.);
#29252=ORIENTED_EDGE('',*,*,#20941,.T.);
#29253=ORIENTED_EDGE('',*,*,#20946,.F.);
#29254=ORIENTED_EDGE('',*,*,#20942,.T.);
#29255=ORIENTED_EDGE('',*,*,#20945,.F.);
#29256=ORIENTED_EDGE('',*,*,#20944,.F.);
#29257=ORIENTED_EDGE('',*,*,#20938,.F.);
#29258=ORIENTED_EDGE('',*,*,#20947,.F.);
#29259=ORIENTED_EDGE('',*,*,#20948,.T.);
#29260=ORIENTED_EDGE('',*,*,#20949,.T.);
#29261=ORIENTED_EDGE('',*,*,#20950,.T.);
#29262=ORIENTED_EDGE('',*,*,#20949,.F.);
#29263=ORIENTED_EDGE('',*,*,#20951,.T.);
#29264=ORIENTED_EDGE('',*,*,#20952,.F.);
#29265=ORIENTED_EDGE('',*,*,#20953,.F.);
#29266=ORIENTED_EDGE('',*,*,#20954,.F.);
#29267=ORIENTED_EDGE('',*,*,#20955,.F.);
#29268=ORIENTED_EDGE('',*,*,#20951,.F.);
#29269=ORIENTED_EDGE('',*,*,#20948,.F.);
#29270=ORIENTED_EDGE('',*,*,#20956,.T.);
#29271=ORIENTED_EDGE('',*,*,#20957,.T.);
#29272=ORIENTED_EDGE('',*,*,#20953,.T.);
#29273=ORIENTED_EDGE('',*,*,#20958,.F.);
#29274=ORIENTED_EDGE('',*,*,#20954,.T.);
#29275=ORIENTED_EDGE('',*,*,#20957,.F.);
#29276=ORIENTED_EDGE('',*,*,#20956,.F.);
#29277=ORIENTED_EDGE('',*,*,#20950,.F.);
#29278=ORIENTED_EDGE('',*,*,#20959,.F.);
#29279=ORIENTED_EDGE('',*,*,#20960,.T.);
#29280=ORIENTED_EDGE('',*,*,#20961,.T.);
#29281=ORIENTED_EDGE('',*,*,#20962,.T.);
#29282=ORIENTED_EDGE('',*,*,#20961,.F.);
#29283=ORIENTED_EDGE('',*,*,#20963,.T.);
#29284=ORIENTED_EDGE('',*,*,#20964,.F.);
#29285=ORIENTED_EDGE('',*,*,#20965,.F.);
#29286=ORIENTED_EDGE('',*,*,#20966,.F.);
#29287=ORIENTED_EDGE('',*,*,#20967,.F.);
#29288=ORIENTED_EDGE('',*,*,#20963,.F.);
#29289=ORIENTED_EDGE('',*,*,#20960,.F.);
#29290=ORIENTED_EDGE('',*,*,#20968,.T.);
#29291=ORIENTED_EDGE('',*,*,#20969,.T.);
#29292=ORIENTED_EDGE('',*,*,#20965,.T.);
#29293=ORIENTED_EDGE('',*,*,#20970,.F.);
#29294=ORIENTED_EDGE('',*,*,#20966,.T.);
#29295=ORIENTED_EDGE('',*,*,#20969,.F.);
#29296=ORIENTED_EDGE('',*,*,#20968,.F.);
#29297=ORIENTED_EDGE('',*,*,#20962,.F.);
#29298=ORIENTED_EDGE('',*,*,#20971,.F.);
#29299=ORIENTED_EDGE('',*,*,#20972,.T.);
#29300=ORIENTED_EDGE('',*,*,#20973,.T.);
#29301=ORIENTED_EDGE('',*,*,#20974,.T.);
#29302=ORIENTED_EDGE('',*,*,#20973,.F.);
#29303=ORIENTED_EDGE('',*,*,#20975,.T.);
#29304=ORIENTED_EDGE('',*,*,#20976,.F.);
#29305=ORIENTED_EDGE('',*,*,#20977,.F.);
#29306=ORIENTED_EDGE('',*,*,#20978,.F.);
#29307=ORIENTED_EDGE('',*,*,#20979,.F.);
#29308=ORIENTED_EDGE('',*,*,#20975,.F.);
#29309=ORIENTED_EDGE('',*,*,#20972,.F.);
#29310=ORIENTED_EDGE('',*,*,#20980,.T.);
#29311=ORIENTED_EDGE('',*,*,#20981,.T.);
#29312=ORIENTED_EDGE('',*,*,#20977,.T.);
#29313=ORIENTED_EDGE('',*,*,#20982,.F.);
#29314=ORIENTED_EDGE('',*,*,#20978,.T.);
#29315=ORIENTED_EDGE('',*,*,#20981,.F.);
#29316=ORIENTED_EDGE('',*,*,#20980,.F.);
#29317=ORIENTED_EDGE('',*,*,#20974,.F.);
#29318=ORIENTED_EDGE('',*,*,#20983,.F.);
#29319=ORIENTED_EDGE('',*,*,#20984,.T.);
#29320=ORIENTED_EDGE('',*,*,#20985,.T.);
#29321=ORIENTED_EDGE('',*,*,#20986,.T.);
#29322=ORIENTED_EDGE('',*,*,#20985,.F.);
#29323=ORIENTED_EDGE('',*,*,#20987,.T.);
#29324=ORIENTED_EDGE('',*,*,#20988,.F.);
#29325=ORIENTED_EDGE('',*,*,#20989,.F.);
#29326=ORIENTED_EDGE('',*,*,#20990,.F.);
#29327=ORIENTED_EDGE('',*,*,#20991,.F.);
#29328=ORIENTED_EDGE('',*,*,#20987,.F.);
#29329=ORIENTED_EDGE('',*,*,#20984,.F.);
#29330=ORIENTED_EDGE('',*,*,#20992,.T.);
#29331=ORIENTED_EDGE('',*,*,#20993,.T.);
#29332=ORIENTED_EDGE('',*,*,#20989,.T.);
#29333=ORIENTED_EDGE('',*,*,#20994,.F.);
#29334=ORIENTED_EDGE('',*,*,#20990,.T.);
#29335=ORIENTED_EDGE('',*,*,#20993,.F.);
#29336=ORIENTED_EDGE('',*,*,#20992,.F.);
#29337=ORIENTED_EDGE('',*,*,#20986,.F.);
#29338=ORIENTED_EDGE('',*,*,#20995,.F.);
#29339=ORIENTED_EDGE('',*,*,#20996,.T.);
#29340=ORIENTED_EDGE('',*,*,#20997,.T.);
#29341=ORIENTED_EDGE('',*,*,#20998,.T.);
#29342=ORIENTED_EDGE('',*,*,#20997,.F.);
#29343=ORIENTED_EDGE('',*,*,#20999,.T.);
#29344=ORIENTED_EDGE('',*,*,#21000,.F.);
#29345=ORIENTED_EDGE('',*,*,#21001,.F.);
#29346=ORIENTED_EDGE('',*,*,#21002,.F.);
#29347=ORIENTED_EDGE('',*,*,#21003,.F.);
#29348=ORIENTED_EDGE('',*,*,#20999,.F.);
#29349=ORIENTED_EDGE('',*,*,#20996,.F.);
#29350=ORIENTED_EDGE('',*,*,#21004,.T.);
#29351=ORIENTED_EDGE('',*,*,#21005,.T.);
#29352=ORIENTED_EDGE('',*,*,#21001,.T.);
#29353=ORIENTED_EDGE('',*,*,#21006,.F.);
#29354=ORIENTED_EDGE('',*,*,#21002,.T.);
#29355=ORIENTED_EDGE('',*,*,#21005,.F.);
#29356=ORIENTED_EDGE('',*,*,#21004,.F.);
#29357=ORIENTED_EDGE('',*,*,#20998,.F.);
#29358=ORIENTED_EDGE('',*,*,#21007,.F.);
#29359=ORIENTED_EDGE('',*,*,#21008,.T.);
#29360=ORIENTED_EDGE('',*,*,#21009,.T.);
#29361=ORIENTED_EDGE('',*,*,#21010,.T.);
#29362=ORIENTED_EDGE('',*,*,#21009,.F.);
#29363=ORIENTED_EDGE('',*,*,#21011,.T.);
#29364=ORIENTED_EDGE('',*,*,#21012,.F.);
#29365=ORIENTED_EDGE('',*,*,#21013,.F.);
#29366=ORIENTED_EDGE('',*,*,#21014,.F.);
#29367=ORIENTED_EDGE('',*,*,#21015,.F.);
#29368=ORIENTED_EDGE('',*,*,#21011,.F.);
#29369=ORIENTED_EDGE('',*,*,#21008,.F.);
#29370=ORIENTED_EDGE('',*,*,#21016,.T.);
#29371=ORIENTED_EDGE('',*,*,#21017,.T.);
#29372=ORIENTED_EDGE('',*,*,#21013,.T.);
#29373=ORIENTED_EDGE('',*,*,#21018,.F.);
#29374=ORIENTED_EDGE('',*,*,#21014,.T.);
#29375=ORIENTED_EDGE('',*,*,#21017,.F.);
#29376=ORIENTED_EDGE('',*,*,#21016,.F.);
#29377=ORIENTED_EDGE('',*,*,#21010,.F.);
#29378=ORIENTED_EDGE('',*,*,#21019,.F.);
#29379=ORIENTED_EDGE('',*,*,#21020,.T.);
#29380=ORIENTED_EDGE('',*,*,#21021,.T.);
#29381=ORIENTED_EDGE('',*,*,#21022,.T.);
#29382=ORIENTED_EDGE('',*,*,#21021,.F.);
#29383=ORIENTED_EDGE('',*,*,#21023,.T.);
#29384=ORIENTED_EDGE('',*,*,#21024,.F.);
#29385=ORIENTED_EDGE('',*,*,#21025,.F.);
#29386=ORIENTED_EDGE('',*,*,#21026,.F.);
#29387=ORIENTED_EDGE('',*,*,#21027,.F.);
#29388=ORIENTED_EDGE('',*,*,#21023,.F.);
#29389=ORIENTED_EDGE('',*,*,#21020,.F.);
#29390=ORIENTED_EDGE('',*,*,#21028,.T.);
#29391=ORIENTED_EDGE('',*,*,#21029,.T.);
#29392=ORIENTED_EDGE('',*,*,#21025,.T.);
#29393=ORIENTED_EDGE('',*,*,#21030,.F.);
#29394=ORIENTED_EDGE('',*,*,#21026,.T.);
#29395=ORIENTED_EDGE('',*,*,#21029,.F.);
#29396=ORIENTED_EDGE('',*,*,#21028,.F.);
#29397=ORIENTED_EDGE('',*,*,#21022,.F.);
#29398=ORIENTED_EDGE('',*,*,#21031,.F.);
#29399=ORIENTED_EDGE('',*,*,#21032,.T.);
#29400=ORIENTED_EDGE('',*,*,#21033,.T.);
#29401=ORIENTED_EDGE('',*,*,#21034,.T.);
#29402=ORIENTED_EDGE('',*,*,#21033,.F.);
#29403=ORIENTED_EDGE('',*,*,#21035,.T.);
#29404=ORIENTED_EDGE('',*,*,#21036,.F.);
#29405=ORIENTED_EDGE('',*,*,#21037,.F.);
#29406=ORIENTED_EDGE('',*,*,#21038,.F.);
#29407=ORIENTED_EDGE('',*,*,#21039,.F.);
#29408=ORIENTED_EDGE('',*,*,#21035,.F.);
#29409=ORIENTED_EDGE('',*,*,#21032,.F.);
#29410=ORIENTED_EDGE('',*,*,#21040,.T.);
#29411=ORIENTED_EDGE('',*,*,#21041,.T.);
#29412=ORIENTED_EDGE('',*,*,#21037,.T.);
#29413=ORIENTED_EDGE('',*,*,#21042,.F.);
#29414=ORIENTED_EDGE('',*,*,#21038,.T.);
#29415=ORIENTED_EDGE('',*,*,#21041,.F.);
#29416=ORIENTED_EDGE('',*,*,#21040,.F.);
#29417=ORIENTED_EDGE('',*,*,#21034,.F.);
#29418=ORIENTED_EDGE('',*,*,#21043,.F.);
#29419=ORIENTED_EDGE('',*,*,#21044,.T.);
#29420=ORIENTED_EDGE('',*,*,#21045,.T.);
#29421=ORIENTED_EDGE('',*,*,#21046,.T.);
#29422=ORIENTED_EDGE('',*,*,#21045,.F.);
#29423=ORIENTED_EDGE('',*,*,#21047,.T.);
#29424=ORIENTED_EDGE('',*,*,#21048,.F.);
#29425=ORIENTED_EDGE('',*,*,#21049,.F.);
#29426=ORIENTED_EDGE('',*,*,#21050,.F.);
#29427=ORIENTED_EDGE('',*,*,#21051,.F.);
#29428=ORIENTED_EDGE('',*,*,#21052,.F.);
#29429=ORIENTED_EDGE('',*,*,#21047,.F.);
#29430=ORIENTED_EDGE('',*,*,#21044,.F.);
#29431=ORIENTED_EDGE('',*,*,#21053,.T.);
#29432=ORIENTED_EDGE('',*,*,#21054,.T.);
#29433=ORIENTED_EDGE('',*,*,#21050,.T.);
#29434=ORIENTED_EDGE('',*,*,#21055,.F.);
#29435=ORIENTED_EDGE('',*,*,#21056,.F.);
#29436=ORIENTED_EDGE('',*,*,#21051,.T.);
#29437=ORIENTED_EDGE('',*,*,#21054,.F.);
#29438=ORIENTED_EDGE('',*,*,#21053,.F.);
#29439=ORIENTED_EDGE('',*,*,#21046,.F.);
#29440=ORIENTED_EDGE('',*,*,#21057,.F.);
#29441=ORIENTED_EDGE('',*,*,#21058,.T.);
#29442=ORIENTED_EDGE('',*,*,#21059,.T.);
#29443=ORIENTED_EDGE('',*,*,#21060,.T.);
#29444=ORIENTED_EDGE('',*,*,#21059,.F.);
#29445=ORIENTED_EDGE('',*,*,#21061,.T.);
#29446=ORIENTED_EDGE('',*,*,#21062,.F.);
#29447=ORIENTED_EDGE('',*,*,#21063,.F.);
#29448=ORIENTED_EDGE('',*,*,#21064,.F.);
#29449=ORIENTED_EDGE('',*,*,#21065,.F.);
#29450=ORIENTED_EDGE('',*,*,#21061,.F.);
#29451=ORIENTED_EDGE('',*,*,#21058,.F.);
#29452=ORIENTED_EDGE('',*,*,#21066,.T.);
#29453=ORIENTED_EDGE('',*,*,#21067,.T.);
#29454=ORIENTED_EDGE('',*,*,#21063,.T.);
#29455=ORIENTED_EDGE('',*,*,#21068,.F.);
#29456=ORIENTED_EDGE('',*,*,#21064,.T.);
#29457=ORIENTED_EDGE('',*,*,#21067,.F.);
#29458=ORIENTED_EDGE('',*,*,#21066,.F.);
#29459=ORIENTED_EDGE('',*,*,#21060,.F.);
#29460=ORIENTED_EDGE('',*,*,#21069,.F.);
#29461=ORIENTED_EDGE('',*,*,#21070,.T.);
#29462=ORIENTED_EDGE('',*,*,#21071,.T.);
#29463=ORIENTED_EDGE('',*,*,#21072,.T.);
#29464=ORIENTED_EDGE('',*,*,#21071,.F.);
#29465=ORIENTED_EDGE('',*,*,#21073,.T.);
#29466=ORIENTED_EDGE('',*,*,#21074,.F.);
#29467=ORIENTED_EDGE('',*,*,#21075,.F.);
#29468=ORIENTED_EDGE('',*,*,#21076,.F.);
#29469=ORIENTED_EDGE('',*,*,#21077,.F.);
#29470=ORIENTED_EDGE('',*,*,#21073,.F.);
#29471=ORIENTED_EDGE('',*,*,#21070,.F.);
#29472=ORIENTED_EDGE('',*,*,#21078,.T.);
#29473=ORIENTED_EDGE('',*,*,#21079,.T.);
#29474=ORIENTED_EDGE('',*,*,#21075,.T.);
#29475=ORIENTED_EDGE('',*,*,#21080,.F.);
#29476=ORIENTED_EDGE('',*,*,#21076,.T.);
#29477=ORIENTED_EDGE('',*,*,#21079,.F.);
#29478=ORIENTED_EDGE('',*,*,#21078,.F.);
#29479=ORIENTED_EDGE('',*,*,#21072,.F.);
#29480=ORIENTED_EDGE('',*,*,#21081,.F.);
#29481=ORIENTED_EDGE('',*,*,#21082,.T.);
#29482=ORIENTED_EDGE('',*,*,#21083,.T.);
#29483=ORIENTED_EDGE('',*,*,#21084,.T.);
#29484=ORIENTED_EDGE('',*,*,#21083,.F.);
#29485=ORIENTED_EDGE('',*,*,#21085,.T.);
#29486=ORIENTED_EDGE('',*,*,#21086,.F.);
#29487=ORIENTED_EDGE('',*,*,#21087,.F.);
#29488=ORIENTED_EDGE('',*,*,#21088,.F.);
#29489=ORIENTED_EDGE('',*,*,#21089,.F.);
#29490=ORIENTED_EDGE('',*,*,#21085,.F.);
#29491=ORIENTED_EDGE('',*,*,#21082,.F.);
#29492=ORIENTED_EDGE('',*,*,#21090,.T.);
#29493=ORIENTED_EDGE('',*,*,#21091,.T.);
#29494=ORIENTED_EDGE('',*,*,#21087,.T.);
#29495=ORIENTED_EDGE('',*,*,#21092,.F.);
#29496=ORIENTED_EDGE('',*,*,#21088,.T.);
#29497=ORIENTED_EDGE('',*,*,#21091,.F.);
#29498=ORIENTED_EDGE('',*,*,#21090,.F.);
#29499=ORIENTED_EDGE('',*,*,#21084,.F.);
#29500=ORIENTED_EDGE('',*,*,#21093,.F.);
#29501=ORIENTED_EDGE('',*,*,#21094,.T.);
#29502=ORIENTED_EDGE('',*,*,#21095,.T.);
#29503=ORIENTED_EDGE('',*,*,#21096,.T.);
#29504=ORIENTED_EDGE('',*,*,#21095,.F.);
#29505=ORIENTED_EDGE('',*,*,#21097,.T.);
#29506=ORIENTED_EDGE('',*,*,#21098,.F.);
#29507=ORIENTED_EDGE('',*,*,#21099,.F.);
#29508=ORIENTED_EDGE('',*,*,#21100,.F.);
#29509=ORIENTED_EDGE('',*,*,#21101,.F.);
#29510=ORIENTED_EDGE('',*,*,#21097,.F.);
#29511=ORIENTED_EDGE('',*,*,#21094,.F.);
#29512=ORIENTED_EDGE('',*,*,#21102,.T.);
#29513=ORIENTED_EDGE('',*,*,#21103,.T.);
#29514=ORIENTED_EDGE('',*,*,#21099,.T.);
#29515=ORIENTED_EDGE('',*,*,#21104,.F.);
#29516=ORIENTED_EDGE('',*,*,#21100,.T.);
#29517=ORIENTED_EDGE('',*,*,#21103,.F.);
#29518=ORIENTED_EDGE('',*,*,#21102,.F.);
#29519=ORIENTED_EDGE('',*,*,#21096,.F.);
#29520=ORIENTED_EDGE('',*,*,#21105,.F.);
#29521=ORIENTED_EDGE('',*,*,#21106,.T.);
#29522=ORIENTED_EDGE('',*,*,#21107,.T.);
#29523=ORIENTED_EDGE('',*,*,#21108,.T.);
#29524=ORIENTED_EDGE('',*,*,#21107,.F.);
#29525=ORIENTED_EDGE('',*,*,#21109,.T.);
#29526=ORIENTED_EDGE('',*,*,#21110,.F.);
#29527=ORIENTED_EDGE('',*,*,#21111,.F.);
#29528=ORIENTED_EDGE('',*,*,#21112,.F.);
#29529=ORIENTED_EDGE('',*,*,#21113,.F.);
#29530=ORIENTED_EDGE('',*,*,#21109,.F.);
#29531=ORIENTED_EDGE('',*,*,#21106,.F.);
#29532=ORIENTED_EDGE('',*,*,#21114,.T.);
#29533=ORIENTED_EDGE('',*,*,#21115,.T.);
#29534=ORIENTED_EDGE('',*,*,#21111,.T.);
#29535=ORIENTED_EDGE('',*,*,#21116,.F.);
#29536=ORIENTED_EDGE('',*,*,#21112,.T.);
#29537=ORIENTED_EDGE('',*,*,#21115,.F.);
#29538=ORIENTED_EDGE('',*,*,#21114,.F.);
#29539=ORIENTED_EDGE('',*,*,#21108,.F.);
#29540=ORIENTED_EDGE('',*,*,#21117,.F.);
#29541=ORIENTED_EDGE('',*,*,#21118,.T.);
#29542=ORIENTED_EDGE('',*,*,#21119,.T.);
#29543=ORIENTED_EDGE('',*,*,#21120,.T.);
#29544=ORIENTED_EDGE('',*,*,#21119,.F.);
#29545=ORIENTED_EDGE('',*,*,#21121,.T.);
#29546=ORIENTED_EDGE('',*,*,#21122,.F.);
#29547=ORIENTED_EDGE('',*,*,#21123,.F.);
#29548=ORIENTED_EDGE('',*,*,#21124,.F.);
#29549=ORIENTED_EDGE('',*,*,#21125,.F.);
#29550=ORIENTED_EDGE('',*,*,#21121,.F.);
#29551=ORIENTED_EDGE('',*,*,#21118,.F.);
#29552=ORIENTED_EDGE('',*,*,#21126,.T.);
#29553=ORIENTED_EDGE('',*,*,#21127,.T.);
#29554=ORIENTED_EDGE('',*,*,#21123,.T.);
#29555=ORIENTED_EDGE('',*,*,#21128,.F.);
#29556=ORIENTED_EDGE('',*,*,#21124,.T.);
#29557=ORIENTED_EDGE('',*,*,#21127,.F.);
#29558=ORIENTED_EDGE('',*,*,#21126,.F.);
#29559=ORIENTED_EDGE('',*,*,#21120,.F.);
#29560=ORIENTED_EDGE('',*,*,#21129,.F.);
#29561=ORIENTED_EDGE('',*,*,#21130,.T.);
#29562=ORIENTED_EDGE('',*,*,#21131,.T.);
#29563=ORIENTED_EDGE('',*,*,#21132,.T.);
#29564=ORIENTED_EDGE('',*,*,#21131,.F.);
#29565=ORIENTED_EDGE('',*,*,#21133,.T.);
#29566=ORIENTED_EDGE('',*,*,#21134,.F.);
#29567=ORIENTED_EDGE('',*,*,#21135,.F.);
#29568=ORIENTED_EDGE('',*,*,#21136,.F.);
#29569=ORIENTED_EDGE('',*,*,#21137,.F.);
#29570=ORIENTED_EDGE('',*,*,#21133,.F.);
#29571=ORIENTED_EDGE('',*,*,#21130,.F.);
#29572=ORIENTED_EDGE('',*,*,#21138,.T.);
#29573=ORIENTED_EDGE('',*,*,#21139,.T.);
#29574=ORIENTED_EDGE('',*,*,#21135,.T.);
#29575=ORIENTED_EDGE('',*,*,#21140,.F.);
#29576=ORIENTED_EDGE('',*,*,#21136,.T.);
#29577=ORIENTED_EDGE('',*,*,#21139,.F.);
#29578=ORIENTED_EDGE('',*,*,#21138,.F.);
#29579=ORIENTED_EDGE('',*,*,#21132,.F.);
#29580=ORIENTED_EDGE('',*,*,#21141,.F.);
#29581=ORIENTED_EDGE('',*,*,#21142,.T.);
#29582=ORIENTED_EDGE('',*,*,#21143,.T.);
#29583=ORIENTED_EDGE('',*,*,#21144,.T.);
#29584=ORIENTED_EDGE('',*,*,#21143,.F.);
#29585=ORIENTED_EDGE('',*,*,#21145,.T.);
#29586=ORIENTED_EDGE('',*,*,#21146,.F.);
#29587=ORIENTED_EDGE('',*,*,#21147,.F.);
#29588=ORIENTED_EDGE('',*,*,#21148,.F.);
#29589=ORIENTED_EDGE('',*,*,#21149,.F.);
#29590=ORIENTED_EDGE('',*,*,#21145,.F.);
#29591=ORIENTED_EDGE('',*,*,#21142,.F.);
#29592=ORIENTED_EDGE('',*,*,#21150,.T.);
#29593=ORIENTED_EDGE('',*,*,#21151,.T.);
#29594=ORIENTED_EDGE('',*,*,#21147,.T.);
#29595=ORIENTED_EDGE('',*,*,#21152,.F.);
#29596=ORIENTED_EDGE('',*,*,#21148,.T.);
#29597=ORIENTED_EDGE('',*,*,#21151,.F.);
#29598=ORIENTED_EDGE('',*,*,#21150,.F.);
#29599=ORIENTED_EDGE('',*,*,#21144,.F.);
#29600=ORIENTED_EDGE('',*,*,#21153,.F.);
#29601=ORIENTED_EDGE('',*,*,#21154,.T.);
#29602=ORIENTED_EDGE('',*,*,#21155,.T.);
#29603=ORIENTED_EDGE('',*,*,#21156,.T.);
#29604=ORIENTED_EDGE('',*,*,#21155,.F.);
#29605=ORIENTED_EDGE('',*,*,#21157,.T.);
#29606=ORIENTED_EDGE('',*,*,#21158,.F.);
#29607=ORIENTED_EDGE('',*,*,#21159,.F.);
#29608=ORIENTED_EDGE('',*,*,#21160,.F.);
#29609=ORIENTED_EDGE('',*,*,#21161,.F.);
#29610=ORIENTED_EDGE('',*,*,#21157,.F.);
#29611=ORIENTED_EDGE('',*,*,#21154,.F.);
#29612=ORIENTED_EDGE('',*,*,#21162,.T.);
#29613=ORIENTED_EDGE('',*,*,#21163,.T.);
#29614=ORIENTED_EDGE('',*,*,#21159,.T.);
#29615=ORIENTED_EDGE('',*,*,#21164,.F.);
#29616=ORIENTED_EDGE('',*,*,#21160,.T.);
#29617=ORIENTED_EDGE('',*,*,#21163,.F.);
#29618=ORIENTED_EDGE('',*,*,#21162,.F.);
#29619=ORIENTED_EDGE('',*,*,#21156,.F.);
#29620=ORIENTED_EDGE('',*,*,#21165,.F.);
#29621=ORIENTED_EDGE('',*,*,#21166,.T.);
#29622=ORIENTED_EDGE('',*,*,#21167,.T.);
#29623=ORIENTED_EDGE('',*,*,#21168,.T.);
#29624=ORIENTED_EDGE('',*,*,#21167,.F.);
#29625=ORIENTED_EDGE('',*,*,#21169,.T.);
#29626=ORIENTED_EDGE('',*,*,#21170,.F.);
#29627=ORIENTED_EDGE('',*,*,#21171,.F.);
#29628=ORIENTED_EDGE('',*,*,#21172,.F.);
#29629=ORIENTED_EDGE('',*,*,#21173,.F.);
#29630=ORIENTED_EDGE('',*,*,#21169,.F.);
#29631=ORIENTED_EDGE('',*,*,#21166,.F.);
#29632=ORIENTED_EDGE('',*,*,#21174,.T.);
#29633=ORIENTED_EDGE('',*,*,#21175,.T.);
#29634=ORIENTED_EDGE('',*,*,#21171,.T.);
#29635=ORIENTED_EDGE('',*,*,#21176,.F.);
#29636=ORIENTED_EDGE('',*,*,#21172,.T.);
#29637=ORIENTED_EDGE('',*,*,#21175,.F.);
#29638=ORIENTED_EDGE('',*,*,#21174,.F.);
#29639=ORIENTED_EDGE('',*,*,#21168,.F.);
#29640=ORIENTED_EDGE('',*,*,#20933,.F.);
#29641=ORIENTED_EDGE('',*,*,#21177,.T.);
#29642=ORIENTED_EDGE('',*,*,#21178,.T.);
#29643=ORIENTED_EDGE('',*,*,#21177,.F.);
#29644=ORIENTED_EDGE('',*,*,#20925,.F.);
#29645=ORIENTED_EDGE('',*,*,#21179,.T.);
#29646=ORIENTED_EDGE('',*,*,#21055,.T.);
#29647=ORIENTED_EDGE('',*,*,#21049,.T.);
#29648=ORIENTED_EDGE('',*,*,#21043,.T.);
#29649=ORIENTED_EDGE('',*,*,#21180,.T.);
#29650=ORIENTED_EDGE('',*,*,#20934,.T.);
#29651=ORIENTED_EDGE('',*,*,#21180,.F.);
#29652=ORIENTED_EDGE('',*,*,#21048,.T.);
#29653=ORIENTED_EDGE('',*,*,#21052,.T.);
#29654=ORIENTED_EDGE('',*,*,#21056,.T.);
#29655=ORIENTED_EDGE('',*,*,#21179,.F.);
#29656=ORIENTED_EDGE('',*,*,#20946,.T.);
#29657=ORIENTED_EDGE('',*,*,#20940,.T.);
#29658=ORIENTED_EDGE('',*,*,#20935,.T.);
#29659=ORIENTED_EDGE('',*,*,#20943,.T.);
#29660=ORIENTED_EDGE('',*,*,#20958,.T.);
#29661=ORIENTED_EDGE('',*,*,#20952,.T.);
#29662=ORIENTED_EDGE('',*,*,#20947,.T.);
#29663=ORIENTED_EDGE('',*,*,#20955,.T.);
#29664=ORIENTED_EDGE('',*,*,#20970,.T.);
#29665=ORIENTED_EDGE('',*,*,#20964,.T.);
#29666=ORIENTED_EDGE('',*,*,#20959,.T.);
#29667=ORIENTED_EDGE('',*,*,#20967,.T.);
#29668=ORIENTED_EDGE('',*,*,#20982,.T.);
#29669=ORIENTED_EDGE('',*,*,#20976,.T.);
#29670=ORIENTED_EDGE('',*,*,#20971,.T.);
#29671=ORIENTED_EDGE('',*,*,#20979,.T.);
#29672=ORIENTED_EDGE('',*,*,#20994,.T.);
#29673=ORIENTED_EDGE('',*,*,#20988,.T.);
#29674=ORIENTED_EDGE('',*,*,#20983,.T.);
#29675=ORIENTED_EDGE('',*,*,#20991,.T.);
#29676=ORIENTED_EDGE('',*,*,#21006,.T.);
#29677=ORIENTED_EDGE('',*,*,#21000,.T.);
#29678=ORIENTED_EDGE('',*,*,#20995,.T.);
#29679=ORIENTED_EDGE('',*,*,#21003,.T.);
#29680=ORIENTED_EDGE('',*,*,#21018,.T.);
#29681=ORIENTED_EDGE('',*,*,#21012,.T.);
#29682=ORIENTED_EDGE('',*,*,#21007,.T.);
#29683=ORIENTED_EDGE('',*,*,#21015,.T.);
#29684=ORIENTED_EDGE('',*,*,#21030,.T.);
#29685=ORIENTED_EDGE('',*,*,#21024,.T.);
#29686=ORIENTED_EDGE('',*,*,#21019,.T.);
#29687=ORIENTED_EDGE('',*,*,#21027,.T.);
#29688=ORIENTED_EDGE('',*,*,#21042,.T.);
#29689=ORIENTED_EDGE('',*,*,#21036,.T.);
#29690=ORIENTED_EDGE('',*,*,#21031,.T.);
#29691=ORIENTED_EDGE('',*,*,#21039,.T.);
#29692=ORIENTED_EDGE('',*,*,#21068,.T.);
#29693=ORIENTED_EDGE('',*,*,#21062,.T.);
#29694=ORIENTED_EDGE('',*,*,#21057,.T.);
#29695=ORIENTED_EDGE('',*,*,#21065,.T.);
#29696=ORIENTED_EDGE('',*,*,#21080,.T.);
#29697=ORIENTED_EDGE('',*,*,#21074,.T.);
#29698=ORIENTED_EDGE('',*,*,#21069,.T.);
#29699=ORIENTED_EDGE('',*,*,#21077,.T.);
#29700=ORIENTED_EDGE('',*,*,#21092,.T.);
#29701=ORIENTED_EDGE('',*,*,#21086,.T.);
#29702=ORIENTED_EDGE('',*,*,#21081,.T.);
#29703=ORIENTED_EDGE('',*,*,#21089,.T.);
#29704=ORIENTED_EDGE('',*,*,#21104,.T.);
#29705=ORIENTED_EDGE('',*,*,#21098,.T.);
#29706=ORIENTED_EDGE('',*,*,#21093,.T.);
#29707=ORIENTED_EDGE('',*,*,#21101,.T.);
#29708=ORIENTED_EDGE('',*,*,#21116,.T.);
#29709=ORIENTED_EDGE('',*,*,#21110,.T.);
#29710=ORIENTED_EDGE('',*,*,#21105,.T.);
#29711=ORIENTED_EDGE('',*,*,#21113,.T.);
#29712=ORIENTED_EDGE('',*,*,#21128,.T.);
#29713=ORIENTED_EDGE('',*,*,#21122,.T.);
#29714=ORIENTED_EDGE('',*,*,#21117,.T.);
#29715=ORIENTED_EDGE('',*,*,#21125,.T.);
#29716=ORIENTED_EDGE('',*,*,#21140,.T.);
#29717=ORIENTED_EDGE('',*,*,#21134,.T.);
#29718=ORIENTED_EDGE('',*,*,#21129,.T.);
#29719=ORIENTED_EDGE('',*,*,#21137,.T.);
#29720=ORIENTED_EDGE('',*,*,#21152,.T.);
#29721=ORIENTED_EDGE('',*,*,#21146,.T.);
#29722=ORIENTED_EDGE('',*,*,#21141,.T.);
#29723=ORIENTED_EDGE('',*,*,#21149,.T.);
#29724=ORIENTED_EDGE('',*,*,#21164,.T.);
#29725=ORIENTED_EDGE('',*,*,#21158,.T.);
#29726=ORIENTED_EDGE('',*,*,#21153,.T.);
#29727=ORIENTED_EDGE('',*,*,#21161,.T.);
#29728=ORIENTED_EDGE('',*,*,#21176,.T.);
#29729=ORIENTED_EDGE('',*,*,#21170,.T.);
#29730=ORIENTED_EDGE('',*,*,#21165,.T.);
#29731=ORIENTED_EDGE('',*,*,#21173,.T.);
#29732=ORIENTED_EDGE('',*,*,#21181,.F.);
#29733=ORIENTED_EDGE('',*,*,#21182,.T.);
#29734=ORIENTED_EDGE('',*,*,#20926,.T.);
#29735=ORIENTED_EDGE('',*,*,#21182,.F.);
#29736=ORIENTED_EDGE('',*,*,#21181,.T.);
#29737=ORIENTED_EDGE('',*,*,#21183,.F.);
#29738=ORIENTED_EDGE('',*,*,#21183,.T.);
#29739=ORIENTED_EDGE('',*,*,#21184,.T.);
#29740=ORIENTED_EDGE('',*,*,#21185,.F.);
#29741=ORIENTED_EDGE('',*,*,#21184,.F.);
#29742=ORIENTED_EDGE('',*,*,#21185,.T.);
#29743=ORIENTED_EDGE('',*,*,#21186,.T.);
#29744=ORIENTED_EDGE('',*,*,#21187,.F.);
#29745=ORIENTED_EDGE('',*,*,#21186,.F.);
#29746=ORIENTED_EDGE('',*,*,#21187,.T.);
#29747=ORIENTED_EDGE('',*,*,#21188,.T.);
#29748=ORIENTED_EDGE('',*,*,#21189,.F.);
#29749=ORIENTED_EDGE('',*,*,#21188,.F.);
#29750=ORIENTED_EDGE('',*,*,#21178,.F.);
#29751=ORIENTED_EDGE('',*,*,#21189,.T.);
#29752=ORIENTED_EDGE('',*,*,#21190,.T.);
#29753=ORIENTED_EDGE('',*,*,#21191,.T.);
#29754=ORIENTED_EDGE('',*,*,#21192,.T.);
#29755=ORIENTED_EDGE('',*,*,#21193,.T.);
#29756=ORIENTED_EDGE('',*,*,#21190,.F.);
#29757=ORIENTED_EDGE('',*,*,#21194,.F.);
#29758=ORIENTED_EDGE('',*,*,#21195,.F.);
#29759=ORIENTED_EDGE('',*,*,#21196,.T.);
#29760=ORIENTED_EDGE('',*,*,#21197,.F.);
#29761=ORIENTED_EDGE('',*,*,#21198,.F.);
#29762=ORIENTED_EDGE('',*,*,#21193,.F.);
#29763=ORIENTED_EDGE('',*,*,#21199,.F.);
#29764=ORIENTED_EDGE('',*,*,#21200,.F.);
#29765=ORIENTED_EDGE('',*,*,#21194,.T.);
#29766=ORIENTED_EDGE('',*,*,#21195,.T.);
#29767=ORIENTED_EDGE('',*,*,#21200,.T.);
#29768=ORIENTED_EDGE('',*,*,#21201,.T.);
#29769=ORIENTED_EDGE('',*,*,#21202,.T.);
#29770=ORIENTED_EDGE('',*,*,#21192,.F.);
#29771=ORIENTED_EDGE('',*,*,#21203,.F.);
#29772=ORIENTED_EDGE('',*,*,#21204,.F.);
#29773=ORIENTED_EDGE('',*,*,#21205,.T.);
#29774=ORIENTED_EDGE('',*,*,#21201,.F.);
#29775=ORIENTED_EDGE('',*,*,#21199,.T.);
#29776=ORIENTED_EDGE('',*,*,#21206,.T.);
#29777=ORIENTED_EDGE('',*,*,#21191,.F.);
#29778=ORIENTED_EDGE('',*,*,#21198,.T.);
#29779=ORIENTED_EDGE('',*,*,#21207,.F.);
#29780=ORIENTED_EDGE('',*,*,#21203,.T.);
#29781=ORIENTED_EDGE('',*,*,#21204,.T.);
#29782=ORIENTED_EDGE('',*,*,#21207,.T.);
#29783=ORIENTED_EDGE('',*,*,#21197,.T.);
#29784=ORIENTED_EDGE('',*,*,#21208,.F.);
#29785=ORIENTED_EDGE('',*,*,#21209,.F.);
#29786=ORIENTED_EDGE('',*,*,#21202,.F.);
#29787=ORIENTED_EDGE('',*,*,#21205,.F.);
#29788=ORIENTED_EDGE('',*,*,#21208,.T.);
#29789=ORIENTED_EDGE('',*,*,#21196,.F.);
#29790=ORIENTED_EDGE('',*,*,#21210,.F.);
#29791=ORIENTED_EDGE('',*,*,#21211,.T.);
#29792=ORIENTED_EDGE('',*,*,#21209,.T.);
#29793=ORIENTED_EDGE('',*,*,#21211,.F.);
#29794=ORIENTED_EDGE('',*,*,#21212,.F.);
#29795=ORIENTED_EDGE('',*,*,#21213,.T.);
#29796=ORIENTED_EDGE('',*,*,#21210,.T.);
#29797=ORIENTED_EDGE('',*,*,#21213,.F.);
#29798=ORIENTED_EDGE('',*,*,#21206,.F.);
#29799=ORIENTED_EDGE('',*,*,#21214,.T.);
#29800=ORIENTED_EDGE('',*,*,#21212,.T.);
#29801=ORIENTED_EDGE('',*,*,#21214,.F.);
#29802=ORIENTED_EDGE('',*,*,#21215,.T.);
#29803=ORIENTED_EDGE('',*,*,#21216,.T.);
#29804=ORIENTED_EDGE('',*,*,#21217,.T.);
#29805=ORIENTED_EDGE('',*,*,#21218,.T.);
#29806=ORIENTED_EDGE('',*,*,#21219,.T.);
#29807=ORIENTED_EDGE('',*,*,#21216,.F.);
#29808=ORIENTED_EDGE('',*,*,#21220,.T.);
#29809=ORIENTED_EDGE('',*,*,#21221,.F.);
#29810=ORIENTED_EDGE('',*,*,#21222,.F.);
#29811=ORIENTED_EDGE('',*,*,#21215,.F.);
#29812=ORIENTED_EDGE('',*,*,#21223,.T.);
#29813=ORIENTED_EDGE('',*,*,#21224,.F.);
#29814=ORIENTED_EDGE('',*,*,#21225,.F.);
#29815=ORIENTED_EDGE('',*,*,#21226,.F.);
#29816=ORIENTED_EDGE('',*,*,#21227,.T.);
#29817=ORIENTED_EDGE('',*,*,#21228,.F.);
#29818=ORIENTED_EDGE('',*,*,#21220,.F.);
#29819=ORIENTED_EDGE('',*,*,#21219,.F.);
#29820=ORIENTED_EDGE('',*,*,#21229,.F.);
#29821=ORIENTED_EDGE('',*,*,#21230,.F.);
#29822=ORIENTED_EDGE('',*,*,#21231,.T.);
#29823=ORIENTED_EDGE('',*,*,#21232,.F.);
#29824=ORIENTED_EDGE('',*,*,#21233,.F.);
#29825=ORIENTED_EDGE('',*,*,#21223,.F.);
#29826=ORIENTED_EDGE('',*,*,#21224,.T.);
#29827=ORIENTED_EDGE('',*,*,#21233,.T.);
#29828=ORIENTED_EDGE('',*,*,#21234,.T.);
#29829=ORIENTED_EDGE('',*,*,#21235,.T.);
#29830=ORIENTED_EDGE('',*,*,#21236,.T.);
#29831=ORIENTED_EDGE('',*,*,#21226,.T.);
#29832=ORIENTED_EDGE('',*,*,#21237,.T.);
#29833=ORIENTED_EDGE('',*,*,#21238,.T.);
#29834=ORIENTED_EDGE('',*,*,#21239,.T.);
#29835=ORIENTED_EDGE('',*,*,#21240,.T.);
#29836=ORIENTED_EDGE('',*,*,#21241,.T.);
#29837=ORIENTED_EDGE('',*,*,#21242,.T.);
#29838=ORIENTED_EDGE('',*,*,#21243,.T.);
#29839=ORIENTED_EDGE('',*,*,#21238,.F.);
#29840=ORIENTED_EDGE('',*,*,#21236,.F.);
#29841=ORIENTED_EDGE('',*,*,#21243,.F.);
#29842=ORIENTED_EDGE('',*,*,#21244,.T.);
#29843=ORIENTED_EDGE('',*,*,#21245,.F.);
#29844=ORIENTED_EDGE('',*,*,#21246,.F.);
#29845=ORIENTED_EDGE('',*,*,#21247,.F.);
#29846=ORIENTED_EDGE('',*,*,#21227,.F.);
#29847=ORIENTED_EDGE('',*,*,#21242,.F.);
#29848=ORIENTED_EDGE('',*,*,#21248,.F.);
#29849=ORIENTED_EDGE('',*,*,#21249,.F.);
#29850=ORIENTED_EDGE('',*,*,#21250,.F.);
#29851=ORIENTED_EDGE('',*,*,#21244,.F.);
#29852=ORIENTED_EDGE('',*,*,#21241,.F.);
#29853=ORIENTED_EDGE('',*,*,#21251,.T.);
#29854=ORIENTED_EDGE('',*,*,#21252,.T.);
#29855=ORIENTED_EDGE('',*,*,#21253,.F.);
#29856=ORIENTED_EDGE('',*,*,#21254,.T.);
#29857=ORIENTED_EDGE('',*,*,#21248,.T.);
#29858=ORIENTED_EDGE('',*,*,#21255,.T.);
#29859=ORIENTED_EDGE('',*,*,#21221,.T.);
#29860=ORIENTED_EDGE('',*,*,#21228,.T.);
#29861=ORIENTED_EDGE('',*,*,#21247,.T.);
#29862=ORIENTED_EDGE('',*,*,#21256,.T.);
#29863=ORIENTED_EDGE('',*,*,#21217,.F.);
#29864=ORIENTED_EDGE('',*,*,#21222,.T.);
#29865=ORIENTED_EDGE('',*,*,#21255,.F.);
#29866=ORIENTED_EDGE('',*,*,#21257,.T.);
#29867=ORIENTED_EDGE('',*,*,#21258,.T.);
#29868=ORIENTED_EDGE('',*,*,#21259,.F.);
#29869=ORIENTED_EDGE('',*,*,#21260,.T.);
#29870=ORIENTED_EDGE('',*,*,#21261,.T.);
#29871=ORIENTED_EDGE('',*,*,#21262,.T.);
#29872=ORIENTED_EDGE('',*,*,#21263,.T.);
#29873=ORIENTED_EDGE('',*,*,#21264,.T.);
#29874=ORIENTED_EDGE('',*,*,#21261,.F.);
#29875=ORIENTED_EDGE('',*,*,#21265,.F.);
#29876=ORIENTED_EDGE('',*,*,#21266,.F.);
#29877=ORIENTED_EDGE('',*,*,#21267,.T.);
#29878=ORIENTED_EDGE('',*,*,#21268,.F.);
#29879=ORIENTED_EDGE('',*,*,#21269,.F.);
#29880=ORIENTED_EDGE('',*,*,#21270,.F.);
#29881=ORIENTED_EDGE('',*,*,#21271,.T.);
#29882=ORIENTED_EDGE('',*,*,#21260,.F.);
#29883=ORIENTED_EDGE('',*,*,#21272,.F.);
#29884=ORIENTED_EDGE('',*,*,#21273,.T.);
#29885=ORIENTED_EDGE('',*,*,#21274,.T.);
#29886=ORIENTED_EDGE('',*,*,#21275,.F.);
#29887=ORIENTED_EDGE('',*,*,#21265,.T.);
#29888=ORIENTED_EDGE('',*,*,#21264,.F.);
#29889=ORIENTED_EDGE('',*,*,#21276,.T.);
#29890=ORIENTED_EDGE('',*,*,#21234,.F.);
#29891=ORIENTED_EDGE('',*,*,#21232,.T.);
#29892=ORIENTED_EDGE('',*,*,#21277,.T.);
#29893=ORIENTED_EDGE('',*,*,#21272,.T.);
#29894=ORIENTED_EDGE('',*,*,#21278,.T.);
#29895=ORIENTED_EDGE('',*,*,#21279,.T.);
#29896=ORIENTED_EDGE('',*,*,#21280,.T.);
#29897=ORIENTED_EDGE('',*,*,#21281,.T.);
#29898=ORIENTED_EDGE('',*,*,#21282,.T.);
#29899=ORIENTED_EDGE('',*,*,#21280,.F.);
#29900=ORIENTED_EDGE('',*,*,#21283,.T.);
#29901=ORIENTED_EDGE('',*,*,#21284,.F.);
#29902=ORIENTED_EDGE('',*,*,#21285,.T.);
#29903=ORIENTED_EDGE('',*,*,#21286,.T.);
#29904=ORIENTED_EDGE('',*,*,#21287,.T.);
#29905=ORIENTED_EDGE('',*,*,#21279,.F.);
#29906=ORIENTED_EDGE('',*,*,#21288,.T.);
#29907=ORIENTED_EDGE('',*,*,#21289,.F.);
#29908=ORIENTED_EDGE('',*,*,#21283,.F.);
#29909=ORIENTED_EDGE('',*,*,#21278,.F.);
#29910=ORIENTED_EDGE('',*,*,#21290,.T.);
#29911=ORIENTED_EDGE('',*,*,#21291,.F.);
#29912=ORIENTED_EDGE('',*,*,#21292,.F.);
#29913=ORIENTED_EDGE('',*,*,#21293,.F.);
#29914=ORIENTED_EDGE('',*,*,#21294,.T.);
#29915=ORIENTED_EDGE('',*,*,#21295,.F.);
#29916=ORIENTED_EDGE('',*,*,#21288,.F.);
#29917=ORIENTED_EDGE('',*,*,#21296,.T.);
#29918=ORIENTED_EDGE('',*,*,#21291,.T.);
#29919=ORIENTED_EDGE('',*,*,#21297,.T.);
#29920=ORIENTED_EDGE('',*,*,#21253,.T.);
#29921=ORIENTED_EDGE('',*,*,#21240,.F.);
#29922=ORIENTED_EDGE('',*,*,#21298,.T.);
#29923=ORIENTED_EDGE('',*,*,#21299,.T.);
#29924=ORIENTED_EDGE('',*,*,#21300,.T.);
#29925=ORIENTED_EDGE('',*,*,#21251,.F.);
#29926=ORIENTED_EDGE('',*,*,#21296,.F.);
#29927=ORIENTED_EDGE('',*,*,#21252,.F.);
#29928=ORIENTED_EDGE('',*,*,#21300,.F.);
#29929=ORIENTED_EDGE('',*,*,#21301,.T.);
#29930=ORIENTED_EDGE('',*,*,#21302,.F.);
#29931=ORIENTED_EDGE('',*,*,#21303,.F.);
#29932=ORIENTED_EDGE('',*,*,#21304,.F.);
#29933=ORIENTED_EDGE('',*,*,#21292,.T.);
#29934=ORIENTED_EDGE('',*,*,#21305,.F.);
#29935=ORIENTED_EDGE('',*,*,#21306,.T.);
#29936=ORIENTED_EDGE('',*,*,#21307,.F.);
#29937=ORIENTED_EDGE('',*,*,#21262,.F.);
#29938=ORIENTED_EDGE('',*,*,#21271,.F.);
#29939=ORIENTED_EDGE('',*,*,#21308,.F.);
#29940=ORIENTED_EDGE('',*,*,#21309,.F.);
#29941=ORIENTED_EDGE('',*,*,#21310,.F.);
#29942=ORIENTED_EDGE('',*,*,#21311,.F.);
#29943=ORIENTED_EDGE('',*,*,#21312,.F.);
#29944=ORIENTED_EDGE('',*,*,#21313,.F.);
#29945=ORIENTED_EDGE('',*,*,#21314,.F.);
#29946=ORIENTED_EDGE('',*,*,#21301,.F.);
#29947=ORIENTED_EDGE('',*,*,#21299,.F.);
#29948=ORIENTED_EDGE('',*,*,#21315,.F.);
#29949=ORIENTED_EDGE('',*,*,#21306,.F.);
#29950=ORIENTED_EDGE('',*,*,#21316,.T.);
#29951=ORIENTED_EDGE('',*,*,#21317,.T.);
#29952=ORIENTED_EDGE('',*,*,#21318,.T.);
#29953=ORIENTED_EDGE('',*,*,#21319,.T.);
#29954=ORIENTED_EDGE('',*,*,#21320,.T.);
#29955=ORIENTED_EDGE('',*,*,#21317,.F.);
#29956=ORIENTED_EDGE('',*,*,#21321,.T.);
#29957=ORIENTED_EDGE('',*,*,#21322,.F.);
#29958=ORIENTED_EDGE('',*,*,#21323,.F.);
#29959=ORIENTED_EDGE('',*,*,#21316,.F.);
#29960=ORIENTED_EDGE('',*,*,#21324,.T.);
#29961=ORIENTED_EDGE('',*,*,#21325,.F.);
#29962=ORIENTED_EDGE('',*,*,#21326,.F.);
#29963=ORIENTED_EDGE('',*,*,#21327,.F.);
#29964=ORIENTED_EDGE('',*,*,#21328,.T.);
#29965=ORIENTED_EDGE('',*,*,#21329,.F.);
#29966=ORIENTED_EDGE('',*,*,#21321,.F.);
#29967=ORIENTED_EDGE('',*,*,#21320,.F.);
#29968=ORIENTED_EDGE('',*,*,#21330,.F.);
#29969=ORIENTED_EDGE('',*,*,#21331,.F.);
#29970=ORIENTED_EDGE('',*,*,#21332,.T.);
#29971=ORIENTED_EDGE('',*,*,#21333,.F.);
#29972=ORIENTED_EDGE('',*,*,#21334,.F.);
#29973=ORIENTED_EDGE('',*,*,#21324,.F.);
#29974=ORIENTED_EDGE('',*,*,#21335,.T.);
#29975=ORIENTED_EDGE('',*,*,#21325,.T.);
#29976=ORIENTED_EDGE('',*,*,#21334,.T.);
#29977=ORIENTED_EDGE('',*,*,#21336,.T.);
#29978=ORIENTED_EDGE('',*,*,#21337,.F.);
#29979=ORIENTED_EDGE('',*,*,#21338,.F.);
#29980=ORIENTED_EDGE('',*,*,#21339,.F.);
#29981=ORIENTED_EDGE('',*,*,#21340,.T.);
#29982=ORIENTED_EDGE('',*,*,#21338,.T.);
#29983=ORIENTED_EDGE('',*,*,#21341,.T.);
#29984=ORIENTED_EDGE('',*,*,#21336,.F.);
#29985=ORIENTED_EDGE('',*,*,#21333,.T.);
#29986=ORIENTED_EDGE('',*,*,#21342,.T.);
#29987=ORIENTED_EDGE('',*,*,#21293,.T.);
#29988=ORIENTED_EDGE('',*,*,#21304,.T.);
#29989=ORIENTED_EDGE('',*,*,#21343,.T.);
#29990=ORIENTED_EDGE('',*,*,#21303,.T.);
#29991=ORIENTED_EDGE('',*,*,#21339,.T.);
#29992=ORIENTED_EDGE('',*,*,#21344,.T.);
#29993=ORIENTED_EDGE('',*,*,#21345,.T.);
#29994=ORIENTED_EDGE('',*,*,#21343,.F.);
#29995=ORIENTED_EDGE('',*,*,#21314,.T.);
#29996=ORIENTED_EDGE('',*,*,#21346,.T.);
#29997=ORIENTED_EDGE('',*,*,#21337,.T.);
#29998=ORIENTED_EDGE('',*,*,#21302,.T.);
#29999=ORIENTED_EDGE('',*,*,#21335,.F.);
#30000=ORIENTED_EDGE('',*,*,#21341,.F.);
#30001=ORIENTED_EDGE('',*,*,#21346,.F.);
#30002=ORIENTED_EDGE('',*,*,#21313,.T.);
#30003=ORIENTED_EDGE('',*,*,#21347,.F.);
#30004=ORIENTED_EDGE('',*,*,#21348,.F.);
#30005=ORIENTED_EDGE('',*,*,#21349,.F.);
#30006=ORIENTED_EDGE('',*,*,#21326,.T.);
#30007=ORIENTED_EDGE('',*,*,#21284,.T.);
#30008=ORIENTED_EDGE('',*,*,#21289,.T.);
#30009=ORIENTED_EDGE('',*,*,#21295,.T.);
#30010=ORIENTED_EDGE('',*,*,#21350,.T.);
#30011=ORIENTED_EDGE('',*,*,#21351,.T.);
#30012=ORIENTED_EDGE('',*,*,#21352,.T.);
#30013=ORIENTED_EDGE('',*,*,#21327,.T.);
#30014=ORIENTED_EDGE('',*,*,#21349,.T.);
#30015=ORIENTED_EDGE('',*,*,#21353,.T.);
#30016=ORIENTED_EDGE('',*,*,#21348,.T.);
#30017=ORIENTED_EDGE('',*,*,#21354,.T.);
#30018=ORIENTED_EDGE('',*,*,#21355,.T.);
#30019=ORIENTED_EDGE('',*,*,#21356,.T.);
#30020=ORIENTED_EDGE('',*,*,#21357,.T.);
#30021=ORIENTED_EDGE('',*,*,#21353,.F.);
#30022=ORIENTED_EDGE('',*,*,#21352,.F.);
#30023=ORIENTED_EDGE('',*,*,#21357,.F.);
#30024=ORIENTED_EDGE('',*,*,#21358,.T.);
#30025=ORIENTED_EDGE('',*,*,#21359,.F.);
#30026=ORIENTED_EDGE('',*,*,#21360,.F.);
#30027=ORIENTED_EDGE('',*,*,#21361,.F.);
#30028=ORIENTED_EDGE('',*,*,#21328,.F.);
#30029=ORIENTED_EDGE('',*,*,#21356,.F.);
#30030=ORIENTED_EDGE('',*,*,#21362,.F.);
#30031=ORIENTED_EDGE('',*,*,#21363,.F.);
#30032=ORIENTED_EDGE('',*,*,#21364,.F.);
#30033=ORIENTED_EDGE('',*,*,#21358,.F.);
#30034=ORIENTED_EDGE('',*,*,#21355,.F.);
#30035=ORIENTED_EDGE('',*,*,#21365,.T.);
#30036=ORIENTED_EDGE('',*,*,#21366,.T.);
#30037=ORIENTED_EDGE('',*,*,#21367,.F.);
#30038=ORIENTED_EDGE('',*,*,#21368,.T.);
#30039=ORIENTED_EDGE('',*,*,#21362,.T.);
#30040=ORIENTED_EDGE('',*,*,#21369,.T.);
#30041=ORIENTED_EDGE('',*,*,#21322,.T.);
#30042=ORIENTED_EDGE('',*,*,#21329,.T.);
#30043=ORIENTED_EDGE('',*,*,#21361,.T.);
#30044=ORIENTED_EDGE('',*,*,#21370,.T.);
#30045=ORIENTED_EDGE('',*,*,#21318,.F.);
#30046=ORIENTED_EDGE('',*,*,#21323,.T.);
#30047=ORIENTED_EDGE('',*,*,#21369,.F.);
#30048=ORIENTED_EDGE('',*,*,#21371,.T.);
#30049=ORIENTED_EDGE('',*,*,#21372,.T.);
#30050=ORIENTED_EDGE('',*,*,#21373,.F.);
#30051=ORIENTED_EDGE('',*,*,#21374,.T.);
#30052=ORIENTED_EDGE('',*,*,#21269,.T.);
#30053=ORIENTED_EDGE('',*,*,#21375,.T.);
#30054=ORIENTED_EDGE('',*,*,#21376,.T.);
#30055=ORIENTED_EDGE('',*,*,#21377,.T.);
#30056=ORIENTED_EDGE('',*,*,#21378,.T.);
#30057=ORIENTED_EDGE('',*,*,#21374,.F.);
#30058=ORIENTED_EDGE('',*,*,#21379,.T.);
#30059=ORIENTED_EDGE('',*,*,#21380,.T.);
#30060=ORIENTED_EDGE('',*,*,#21308,.T.);
#30061=ORIENTED_EDGE('',*,*,#21270,.T.);
#30062=ORIENTED_EDGE('',*,*,#21381,.T.);
#30063=ORIENTED_EDGE('',*,*,#21382,.T.);
#30064=ORIENTED_EDGE('',*,*,#21266,.T.);
#30065=ORIENTED_EDGE('',*,*,#21275,.T.);
#30066=ORIENTED_EDGE('',*,*,#21382,.F.);
#30067=ORIENTED_EDGE('',*,*,#21383,.T.);
#30068=ORIENTED_EDGE('',*,*,#21384,.F.);
#30069=ORIENTED_EDGE('',*,*,#21385,.F.);
#30070=ORIENTED_EDGE('',*,*,#21386,.F.);
#30071=ORIENTED_EDGE('',*,*,#21387,.T.);
#30072=ORIENTED_EDGE('',*,*,#21388,.F.);
#30073=ORIENTED_EDGE('',*,*,#21267,.F.);
#30074=ORIENTED_EDGE('',*,*,#21381,.F.);
#30075=ORIENTED_EDGE('',*,*,#21274,.F.);
#30076=ORIENTED_EDGE('',*,*,#21389,.T.);
#30077=ORIENTED_EDGE('',*,*,#21390,.F.);
#30078=ORIENTED_EDGE('',*,*,#21391,.F.);
#30079=ORIENTED_EDGE('',*,*,#21392,.F.);
#30080=ORIENTED_EDGE('',*,*,#21383,.F.);
#30081=ORIENTED_EDGE('',*,*,#21273,.F.);
#30082=ORIENTED_EDGE('',*,*,#21277,.F.);
#30083=ORIENTED_EDGE('',*,*,#21231,.F.);
#30084=ORIENTED_EDGE('',*,*,#21393,.F.);
#30085=ORIENTED_EDGE('',*,*,#21389,.F.);
#30086=ORIENTED_EDGE('',*,*,#21380,.F.);
#30087=ORIENTED_EDGE('',*,*,#21394,.F.);
#30088=ORIENTED_EDGE('',*,*,#21395,.F.);
#30089=ORIENTED_EDGE('',*,*,#21396,.T.);
#30090=ORIENTED_EDGE('',*,*,#21397,.F.);
#30091=ORIENTED_EDGE('',*,*,#21398,.F.);
#30092=ORIENTED_EDGE('',*,*,#21399,.F.);
#30093=ORIENTED_EDGE('',*,*,#21309,.T.);
#30094=ORIENTED_EDGE('',*,*,#21378,.F.);
#30095=ORIENTED_EDGE('',*,*,#21400,.T.);
#30096=ORIENTED_EDGE('',*,*,#21401,.T.);
#30097=ORIENTED_EDGE('',*,*,#21402,.F.);
#30098=ORIENTED_EDGE('',*,*,#21394,.T.);
#30099=ORIENTED_EDGE('',*,*,#21379,.F.);
#30100=ORIENTED_EDGE('',*,*,#21403,.T.);
#30101=ORIENTED_EDGE('',*,*,#21395,.T.);
#30102=ORIENTED_EDGE('',*,*,#21402,.T.);
#30103=ORIENTED_EDGE('',*,*,#21404,.T.);
#30104=ORIENTED_EDGE('',*,*,#21404,.F.);
#30105=ORIENTED_EDGE('',*,*,#21401,.F.);
#30106=ORIENTED_EDGE('',*,*,#21405,.T.);
#30107=ORIENTED_EDGE('',*,*,#21406,.F.);
#30108=ORIENTED_EDGE('',*,*,#21407,.F.);
#30109=ORIENTED_EDGE('',*,*,#21408,.F.);
#30110=ORIENTED_EDGE('',*,*,#21409,.F.);
#30111=ORIENTED_EDGE('',*,*,#21388,.T.);
#30112=ORIENTED_EDGE('',*,*,#21410,.T.);
#30113=ORIENTED_EDGE('',*,*,#21375,.F.);
#30114=ORIENTED_EDGE('',*,*,#21268,.T.);
#30115=ORIENTED_EDGE('',*,*,#21410,.F.);
#30116=ORIENTED_EDGE('',*,*,#21387,.F.);
#30117=ORIENTED_EDGE('',*,*,#21411,.F.);
#30118=ORIENTED_EDGE('',*,*,#21412,.F.);
#30119=ORIENTED_EDGE('',*,*,#21413,.F.);
#30120=ORIENTED_EDGE('',*,*,#21414,.T.);
#30121=ORIENTED_EDGE('',*,*,#21376,.F.);
#30122=ORIENTED_EDGE('',*,*,#21386,.T.);
#30123=ORIENTED_EDGE('',*,*,#21415,.T.);
#30124=ORIENTED_EDGE('',*,*,#21416,.T.);
#30125=ORIENTED_EDGE('',*,*,#21417,.T.);
#30126=ORIENTED_EDGE('',*,*,#21411,.T.);
#30127=ORIENTED_EDGE('',*,*,#21416,.F.);
#30128=ORIENTED_EDGE('',*,*,#21418,.T.);
#30129=ORIENTED_EDGE('',*,*,#21419,.T.);
#30130=ORIENTED_EDGE('',*,*,#21420,.T.);
#30131=ORIENTED_EDGE('',*,*,#21421,.T.);
#30132=ORIENTED_EDGE('',*,*,#21415,.F.);
#30133=ORIENTED_EDGE('',*,*,#21385,.T.);
#30134=ORIENTED_EDGE('',*,*,#21422,.F.);
#30135=ORIENTED_EDGE('',*,*,#21418,.F.);
#30136=ORIENTED_EDGE('',*,*,#21423,.F.);
#30137=ORIENTED_EDGE('',*,*,#21419,.F.);
#30138=ORIENTED_EDGE('',*,*,#21424,.F.);
#30139=ORIENTED_EDGE('',*,*,#21384,.T.);
#30140=ORIENTED_EDGE('',*,*,#21392,.T.);
#30141=ORIENTED_EDGE('',*,*,#21424,.T.);
#30142=ORIENTED_EDGE('',*,*,#21422,.T.);
#30143=ORIENTED_EDGE('',*,*,#21425,.T.);
#30144=ORIENTED_EDGE('',*,*,#21423,.T.);
#30145=ORIENTED_EDGE('',*,*,#21391,.T.);
#30146=ORIENTED_EDGE('',*,*,#21426,.T.);
#30147=ORIENTED_EDGE('',*,*,#21218,.F.);
#30148=ORIENTED_EDGE('',*,*,#21259,.T.);
#30149=ORIENTED_EDGE('',*,*,#21427,.T.);
#30150=ORIENTED_EDGE('',*,*,#21428,.T.);
#30151=ORIENTED_EDGE('',*,*,#21229,.T.);
#30152=ORIENTED_EDGE('',*,*,#21256,.F.);
#30153=ORIENTED_EDGE('',*,*,#21246,.T.);
#30154=ORIENTED_EDGE('',*,*,#21429,.T.);
#30155=ORIENTED_EDGE('',*,*,#21430,.T.);
#30156=ORIENTED_EDGE('',*,*,#21257,.F.);
#30157=ORIENTED_EDGE('',*,*,#21351,.F.);
#30158=ORIENTED_EDGE('',*,*,#21431,.T.);
#30159=ORIENTED_EDGE('',*,*,#21432,.T.);
#30160=ORIENTED_EDGE('',*,*,#21433,.T.);
#30161=ORIENTED_EDGE('',*,*,#21285,.F.);
#30162=ORIENTED_EDGE('',*,*,#21319,.F.);
#30163=ORIENTED_EDGE('',*,*,#21373,.T.);
#30164=ORIENTED_EDGE('',*,*,#21434,.T.);
#30165=ORIENTED_EDGE('',*,*,#21435,.T.);
#30166=ORIENTED_EDGE('',*,*,#21330,.T.);
#30167=ORIENTED_EDGE('',*,*,#21370,.F.);
#30168=ORIENTED_EDGE('',*,*,#21360,.T.);
#30169=ORIENTED_EDGE('',*,*,#21436,.T.);
#30170=ORIENTED_EDGE('',*,*,#21437,.T.);
#30171=ORIENTED_EDGE('',*,*,#21371,.F.);
#30172=ORIENTED_EDGE('',*,*,#21438,.T.);
#30173=ORIENTED_EDGE('',*,*,#21439,.T.);
#30174=ORIENTED_EDGE('',*,*,#21440,.T.);
#30175=ORIENTED_EDGE('',*,*,#21441,.T.);
#30176=ORIENTED_EDGE('',*,*,#21442,.T.);
#30177=ORIENTED_EDGE('',*,*,#21364,.T.);
#30178=ORIENTED_EDGE('',*,*,#21443,.T.);
#30179=ORIENTED_EDGE('',*,*,#21442,.F.);
#30180=ORIENTED_EDGE('',*,*,#21444,.T.);
#30181=ORIENTED_EDGE('',*,*,#21436,.F.);
#30182=ORIENTED_EDGE('',*,*,#21359,.T.);
#30183=ORIENTED_EDGE('',*,*,#21445,.T.);
#30184=ORIENTED_EDGE('',*,*,#21331,.T.);
#30185=ORIENTED_EDGE('',*,*,#21435,.F.);
#30186=ORIENTED_EDGE('',*,*,#21446,.T.);
#30187=ORIENTED_EDGE('',*,*,#21432,.F.);
#30188=ORIENTED_EDGE('',*,*,#21447,.T.);
#30189=ORIENTED_EDGE('',*,*,#21281,.F.);
#30190=ORIENTED_EDGE('',*,*,#21287,.F.);
#30191=ORIENTED_EDGE('',*,*,#21448,.T.);
#30192=ORIENTED_EDGE('',*,*,#21449,.T.);
#30193=ORIENTED_EDGE('',*,*,#21450,.T.);
#30194=ORIENTED_EDGE('',*,*,#21250,.T.);
#30195=ORIENTED_EDGE('',*,*,#21451,.T.);
#30196=ORIENTED_EDGE('',*,*,#21449,.F.);
#30197=ORIENTED_EDGE('',*,*,#21452,.T.);
#30198=ORIENTED_EDGE('',*,*,#21429,.F.);
#30199=ORIENTED_EDGE('',*,*,#21245,.T.);
#30200=ORIENTED_EDGE('',*,*,#21393,.T.);
#30201=ORIENTED_EDGE('',*,*,#21230,.T.);
#30202=ORIENTED_EDGE('',*,*,#21428,.F.);
#30203=ORIENTED_EDGE('',*,*,#21453,.T.);
#30204=ORIENTED_EDGE('',*,*,#21426,.F.);
#30205=ORIENTED_EDGE('',*,*,#21390,.T.);
#30206=ORIENTED_EDGE('',*,*,#21417,.F.);
#30207=ORIENTED_EDGE('',*,*,#21421,.F.);
#30208=ORIENTED_EDGE('',*,*,#21454,.T.);
#30209=ORIENTED_EDGE('',*,*,#21455,.T.);
#30210=ORIENTED_EDGE('',*,*,#21412,.T.);
#30211=ORIENTED_EDGE('',*,*,#21420,.F.);
#30212=ORIENTED_EDGE('',*,*,#21425,.F.);
#30213=ORIENTED_EDGE('',*,*,#21453,.F.);
#30214=ORIENTED_EDGE('',*,*,#21427,.F.);
#30215=ORIENTED_EDGE('',*,*,#21258,.F.);
#30216=ORIENTED_EDGE('',*,*,#21430,.F.);
#30217=ORIENTED_EDGE('',*,*,#21452,.F.);
#30218=ORIENTED_EDGE('',*,*,#21448,.F.);
#30219=ORIENTED_EDGE('',*,*,#21286,.F.);
#30220=ORIENTED_EDGE('',*,*,#21433,.F.);
#30221=ORIENTED_EDGE('',*,*,#21446,.F.);
#30222=ORIENTED_EDGE('',*,*,#21434,.F.);
#30223=ORIENTED_EDGE('',*,*,#21372,.F.);
#30224=ORIENTED_EDGE('',*,*,#21437,.F.);
#30225=ORIENTED_EDGE('',*,*,#21444,.F.);
#30226=ORIENTED_EDGE('',*,*,#21441,.F.);
#30227=ORIENTED_EDGE('',*,*,#21456,.F.);
#30228=ORIENTED_EDGE('',*,*,#21457,.F.);
#30229=ORIENTED_EDGE('',*,*,#21458,.F.);
#30230=ORIENTED_EDGE('',*,*,#21459,.F.);
#30231=ORIENTED_EDGE('',*,*,#21460,.F.);
#30232=ORIENTED_EDGE('',*,*,#21461,.F.);
#30233=ORIENTED_EDGE('',*,*,#21462,.F.);
#30234=ORIENTED_EDGE('',*,*,#21463,.T.);
#30235=ORIENTED_EDGE('',*,*,#21464,.T.);
#30236=ORIENTED_EDGE('',*,*,#21465,.T.);
#30237=ORIENTED_EDGE('',*,*,#21463,.F.);
#30238=ORIENTED_EDGE('',*,*,#21466,.F.);
#30239=ORIENTED_EDGE('',*,*,#21454,.F.);
#30240=ORIENTED_EDGE('',*,*,#21440,.F.);
#30241=ORIENTED_EDGE('',*,*,#21467,.F.);
#30242=ORIENTED_EDGE('',*,*,#21468,.T.);
#30243=ORIENTED_EDGE('',*,*,#21469,.T.);
#30244=ORIENTED_EDGE('',*,*,#21456,.T.);
#30245=ORIENTED_EDGE('',*,*,#21439,.F.);
#30246=ORIENTED_EDGE('',*,*,#21470,.T.);
#30247=ORIENTED_EDGE('',*,*,#21471,.T.);
#30248=ORIENTED_EDGE('',*,*,#21472,.T.);
#30249=ORIENTED_EDGE('',*,*,#21467,.T.);
#30250=ORIENTED_EDGE('',*,*,#21473,.T.);
#30251=ORIENTED_EDGE('',*,*,#21474,.T.);
#30252=ORIENTED_EDGE('',*,*,#21475,.T.);
#30253=ORIENTED_EDGE('',*,*,#21367,.T.);
#30254=ORIENTED_EDGE('',*,*,#21354,.F.);
#30255=ORIENTED_EDGE('',*,*,#21347,.T.);
#30256=ORIENTED_EDGE('',*,*,#21312,.T.);
#30257=ORIENTED_EDGE('',*,*,#21476,.T.);
#30258=ORIENTED_EDGE('',*,*,#21365,.F.);
#30259=ORIENTED_EDGE('',*,*,#21474,.F.);
#30260=ORIENTED_EDGE('',*,*,#21477,.F.);
#30261=ORIENTED_EDGE('',*,*,#21478,.F.);
#30262=ORIENTED_EDGE('',*,*,#21479,.T.);
#30263=ORIENTED_EDGE('',*,*,#21480,.F.);
#30264=ORIENTED_EDGE('',*,*,#21481,.F.);
#30265=ORIENTED_EDGE('',*,*,#21471,.F.);
#30266=ORIENTED_EDGE('',*,*,#21482,.T.);
#30267=ORIENTED_EDGE('',*,*,#21473,.F.);
#30268=ORIENTED_EDGE('',*,*,#21366,.F.);
#30269=ORIENTED_EDGE('',*,*,#21476,.F.);
#30270=ORIENTED_EDGE('',*,*,#21311,.T.);
#30271=ORIENTED_EDGE('',*,*,#21483,.F.);
#30272=ORIENTED_EDGE('',*,*,#21484,.F.);
#30273=ORIENTED_EDGE('',*,*,#21485,.F.);
#30274=ORIENTED_EDGE('',*,*,#21477,.T.);
#30275=ORIENTED_EDGE('',*,*,#21486,.F.);
#30276=ORIENTED_EDGE('',*,*,#21487,.F.);
#30277=ORIENTED_EDGE('',*,*,#21488,.F.);
#30278=ORIENTED_EDGE('',*,*,#21489,.F.);
#30279=ORIENTED_EDGE('',*,*,#21490,.F.);
#30280=ORIENTED_EDGE('',*,*,#21491,.F.);
#30281=ORIENTED_EDGE('',*,*,#21492,.T.);
#30282=ORIENTED_EDGE('',*,*,#21490,.T.);
#30283=ORIENTED_EDGE('',*,*,#21459,.T.);
#30284=ORIENTED_EDGE('',*,*,#21493,.T.);
#30285=ORIENTED_EDGE('',*,*,#21494,.F.);
#30286=ORIENTED_EDGE('',*,*,#21469,.F.);
#30287=ORIENTED_EDGE('',*,*,#21495,.F.);
#30288=ORIENTED_EDGE('',*,*,#21480,.T.);
#30289=ORIENTED_EDGE('',*,*,#21496,.T.);
#30290=ORIENTED_EDGE('',*,*,#21495,.T.);
#30291=ORIENTED_EDGE('',*,*,#21497,.T.);
#30292=ORIENTED_EDGE('',*,*,#21457,.T.);
#30293=ORIENTED_EDGE('',*,*,#21494,.T.);
#30294=ORIENTED_EDGE('',*,*,#21498,.T.);
#30295=ORIENTED_EDGE('',*,*,#21499,.T.);
#30296=ORIENTED_EDGE('',*,*,#21458,.T.);
#30297=ORIENTED_EDGE('',*,*,#21499,.F.);
#30298=ORIENTED_EDGE('',*,*,#21500,.T.);
#30299=ORIENTED_EDGE('',*,*,#21501,.T.);
#30300=ORIENTED_EDGE('',*,*,#21502,.T.);
#30301=ORIENTED_EDGE('',*,*,#21493,.F.);
#30302=ORIENTED_EDGE('',*,*,#21503,.T.);
#30303=ORIENTED_EDGE('',*,*,#21504,.T.);
#30304=ORIENTED_EDGE('',*,*,#21491,.T.);
#30305=ORIENTED_EDGE('',*,*,#21505,.T.);
#30306=ORIENTED_EDGE('',*,*,#21489,.T.);
#30307=ORIENTED_EDGE('',*,*,#21506,.T.);
#30308=ORIENTED_EDGE('',*,*,#21487,.T.);
#30309=ORIENTED_EDGE('',*,*,#21460,.T.);
#30310=ORIENTED_EDGE('',*,*,#21507,.T.);
#30311=ORIENTED_EDGE('',*,*,#21408,.T.);
#30312=ORIENTED_EDGE('',*,*,#21488,.T.);
#30313=ORIENTED_EDGE('',*,*,#21508,.T.);
#30314=ORIENTED_EDGE('',*,*,#21461,.T.);
#30315=ORIENTED_EDGE('',*,*,#21486,.T.);
#30316=ORIENTED_EDGE('',*,*,#21407,.T.);
#30317=ORIENTED_EDGE('',*,*,#21509,.T.);
#30318=ORIENTED_EDGE('',*,*,#21466,.T.);
#30319=ORIENTED_EDGE('',*,*,#21462,.T.);
#30320=ORIENTED_EDGE('',*,*,#21509,.F.);
#30321=ORIENTED_EDGE('',*,*,#21406,.T.);
#30322=ORIENTED_EDGE('',*,*,#21510,.T.);
#30323=ORIENTED_EDGE('',*,*,#21413,.T.);
#30324=ORIENTED_EDGE('',*,*,#21455,.F.);
#30325=ORIENTED_EDGE('',*,*,#21438,.F.);
#30326=ORIENTED_EDGE('',*,*,#21443,.F.);
#30327=ORIENTED_EDGE('',*,*,#21363,.T.);
#30328=ORIENTED_EDGE('',*,*,#21368,.F.);
#30329=ORIENTED_EDGE('',*,*,#21475,.F.);
#30330=ORIENTED_EDGE('',*,*,#21482,.F.);
#30331=ORIENTED_EDGE('',*,*,#21470,.F.);
#30332=ORIENTED_EDGE('',*,*,#21377,.F.);
#30333=ORIENTED_EDGE('',*,*,#21414,.F.);
#30334=ORIENTED_EDGE('',*,*,#21510,.F.);
#30335=ORIENTED_EDGE('',*,*,#21405,.F.);
#30336=ORIENTED_EDGE('',*,*,#21400,.F.);
#30337=ORIENTED_EDGE('',*,*,#21397,.T.);
#30338=ORIENTED_EDGE('',*,*,#21511,.T.);
#30339=ORIENTED_EDGE('',*,*,#21512,.T.);
#30340=ORIENTED_EDGE('',*,*,#21513,.T.);
#30341=ORIENTED_EDGE('',*,*,#21514,.F.);
#30342=ORIENTED_EDGE('',*,*,#21515,.F.);
#30343=ORIENTED_EDGE('',*,*,#21516,.F.);
#30344=ORIENTED_EDGE('',*,*,#21517,.T.);
#30345=ORIENTED_EDGE('',*,*,#21515,.T.);
#30346=ORIENTED_EDGE('',*,*,#21398,.T.);
#30347=ORIENTED_EDGE('',*,*,#21513,.F.);
#30348=ORIENTED_EDGE('',*,*,#21518,.T.);
#30349=ORIENTED_EDGE('',*,*,#21519,.T.);
#30350=ORIENTED_EDGE('',*,*,#21478,.T.);
#30351=ORIENTED_EDGE('',*,*,#21485,.T.);
#30352=ORIENTED_EDGE('',*,*,#21520,.T.);
#30353=ORIENTED_EDGE('',*,*,#21484,.T.);
#30354=ORIENTED_EDGE('',*,*,#21516,.T.);
#30355=ORIENTED_EDGE('',*,*,#21521,.T.);
#30356=ORIENTED_EDGE('',*,*,#21522,.T.);
#30357=ORIENTED_EDGE('',*,*,#21520,.F.);
#30358=ORIENTED_EDGE('',*,*,#21310,.T.);
#30359=ORIENTED_EDGE('',*,*,#21399,.T.);
#30360=ORIENTED_EDGE('',*,*,#21514,.T.);
#30361=ORIENTED_EDGE('',*,*,#21483,.T.);
#30362=ORIENTED_EDGE('',*,*,#21403,.F.);
#30363=ORIENTED_EDGE('',*,*,#21409,.T.);
#30364=ORIENTED_EDGE('',*,*,#21507,.F.);
#30365=ORIENTED_EDGE('',*,*,#21523,.F.);
#30366=ORIENTED_EDGE('',*,*,#21503,.F.);
#30367=ORIENTED_EDGE('',*,*,#21524,.T.);
#30368=ORIENTED_EDGE('',*,*,#21511,.F.);
#30369=ORIENTED_EDGE('',*,*,#21396,.F.);
#30370=ORIENTED_EDGE('',*,*,#21525,.F.);
#30371=ORIENTED_EDGE('',*,*,#21526,.T.);
#30372=ORIENTED_EDGE('',*,*,#21464,.F.);
#30373=ORIENTED_EDGE('',*,*,#21465,.F.);
#30374=ORIENTED_EDGE('',*,*,#21526,.F.);
#30375=ORIENTED_EDGE('',*,*,#21496,.F.);
#30376=ORIENTED_EDGE('',*,*,#21479,.F.);
#30377=ORIENTED_EDGE('',*,*,#21519,.F.);
#30378=ORIENTED_EDGE('',*,*,#21522,.F.);
#30379=ORIENTED_EDGE('',*,*,#21527,.T.);
#30380=ORIENTED_EDGE('',*,*,#21500,.F.);
#30381=ORIENTED_EDGE('',*,*,#21498,.F.);
#30382=ORIENTED_EDGE('',*,*,#21492,.F.);
#30383=ORIENTED_EDGE('',*,*,#21502,.F.);
#30384=ORIENTED_EDGE('',*,*,#21528,.T.);
#30385=ORIENTED_EDGE('',*,*,#21518,.F.);
#30386=ORIENTED_EDGE('',*,*,#21512,.F.);
#30387=ORIENTED_EDGE('',*,*,#21524,.F.);
#30388=ORIENTED_EDGE('',*,*,#21505,.F.);
#30389=ORIENTED_EDGE('',*,*,#21501,.F.);
#30390=ORIENTED_EDGE('',*,*,#21527,.F.);
#30391=ORIENTED_EDGE('',*,*,#21521,.F.);
#30392=ORIENTED_EDGE('',*,*,#21517,.F.);
#30393=ORIENTED_EDGE('',*,*,#21528,.F.);
#30394=ORIENTED_EDGE('',*,*,#21504,.F.);
#30395=ORIENTED_EDGE('',*,*,#21523,.T.);
#30396=ORIENTED_EDGE('',*,*,#21508,.F.);
#30397=ORIENTED_EDGE('',*,*,#21506,.F.);
#30398=ORIENTED_EDGE('',*,*,#21472,.F.);
#30399=ORIENTED_EDGE('',*,*,#21481,.T.);
#30400=ORIENTED_EDGE('',*,*,#21497,.F.);
#30401=ORIENTED_EDGE('',*,*,#21468,.F.);
#30402=ORIENTED_EDGE('',*,*,#21342,.F.);
#30403=ORIENTED_EDGE('',*,*,#21345,.F.);
#30404=ORIENTED_EDGE('',*,*,#21529,.T.);
#30405=ORIENTED_EDGE('',*,*,#21447,.F.);
#30406=ORIENTED_EDGE('',*,*,#21431,.F.);
#30407=ORIENTED_EDGE('',*,*,#21350,.F.);
#30408=ORIENTED_EDGE('',*,*,#21294,.F.);
#30409=ORIENTED_EDGE('',*,*,#21340,.F.);
#30410=ORIENTED_EDGE('',*,*,#21332,.F.);
#30411=ORIENTED_EDGE('',*,*,#21445,.F.);
#30412=ORIENTED_EDGE('',*,*,#21529,.F.);
#30413=ORIENTED_EDGE('',*,*,#21344,.F.);
#30414=ORIENTED_EDGE('',*,*,#21282,.F.);
#30415=ORIENTED_EDGE('',*,*,#21450,.F.);
#30416=ORIENTED_EDGE('',*,*,#21451,.F.);
#30417=ORIENTED_EDGE('',*,*,#21249,.T.);
#30418=ORIENTED_EDGE('',*,*,#21254,.F.);
#30419=ORIENTED_EDGE('',*,*,#21297,.F.);
#30420=ORIENTED_EDGE('',*,*,#21290,.F.);
#30421=ORIENTED_EDGE('',*,*,#21276,.F.);
#30422=ORIENTED_EDGE('',*,*,#21263,.F.);
#30423=ORIENTED_EDGE('',*,*,#21307,.T.);
#30424=ORIENTED_EDGE('',*,*,#21315,.T.);
#30425=ORIENTED_EDGE('',*,*,#21298,.F.);
#30426=ORIENTED_EDGE('',*,*,#21239,.F.);
#30427=ORIENTED_EDGE('',*,*,#21237,.F.);
#30428=ORIENTED_EDGE('',*,*,#21225,.T.);
#30429=ORIENTED_EDGE('',*,*,#21235,.F.);
#30430=ORIENTED_EDGE('',*,*,#21305,.T.);
#30431=ORIENTED_EDGE('',*,*,#21525,.T.);
#30432=ORIENTED_EDGE('',*,*,#21530,.T.);
#30433=ORIENTED_EDGE('',*,*,#21531,.T.);
#30434=ORIENTED_EDGE('',*,*,#21532,.T.);
#30435=ORIENTED_EDGE('',*,*,#21533,.T.);
#30436=ORIENTED_EDGE('',*,*,#21534,.T.);
#30437=ORIENTED_EDGE('',*,*,#21531,.F.);
#30438=ORIENTED_EDGE('',*,*,#21535,.T.);
#30439=ORIENTED_EDGE('',*,*,#21532,.F.);
#30440=ORIENTED_EDGE('',*,*,#21536,.T.);
#30441=ORIENTED_EDGE('',*,*,#21537,.T.);
#30442=ORIENTED_EDGE('',*,*,#21538,.F.);
#30443=ORIENTED_EDGE('',*,*,#21539,.F.);
#30444=ORIENTED_EDGE('',*,*,#21540,.F.);
#30445=ORIENTED_EDGE('',*,*,#21541,.T.);
#30446=ORIENTED_EDGE('',*,*,#21542,.F.);
#30447=ORIENTED_EDGE('',*,*,#21543,.F.);
#30448=ORIENTED_EDGE('',*,*,#21544,.F.);
#30449=ORIENTED_EDGE('',*,*,#21545,.T.);
#30450=ORIENTED_EDGE('',*,*,#21536,.F.);
#30451=ORIENTED_EDGE('',*,*,#21546,.T.);
#30452=ORIENTED_EDGE('',*,*,#21538,.T.);
#30453=ORIENTED_EDGE('',*,*,#21547,.T.);
#30454=ORIENTED_EDGE('',*,*,#21548,.T.);
#30455=ORIENTED_EDGE('',*,*,#21549,.T.);
#30456=ORIENTED_EDGE('',*,*,#21546,.F.);
#30457=ORIENTED_EDGE('',*,*,#21550,.T.);
#30458=ORIENTED_EDGE('',*,*,#21551,.T.);
#30459=ORIENTED_EDGE('',*,*,#21552,.F.);
#30460=ORIENTED_EDGE('',*,*,#21553,.F.);
#30461=ORIENTED_EDGE('',*,*,#21539,.T.);
#30462=ORIENTED_EDGE('',*,*,#21549,.F.);
#30463=ORIENTED_EDGE('',*,*,#21554,.T.);
#30464=ORIENTED_EDGE('',*,*,#21555,.F.);
#30465=ORIENTED_EDGE('',*,*,#21552,.T.);
#30466=ORIENTED_EDGE('',*,*,#21556,.T.);
#30467=ORIENTED_EDGE('',*,*,#21550,.F.);
#30468=ORIENTED_EDGE('',*,*,#21548,.F.);
#30469=ORIENTED_EDGE('',*,*,#21557,.T.);
#30470=ORIENTED_EDGE('',*,*,#21558,.F.);
#30471=ORIENTED_EDGE('',*,*,#21554,.F.);
#30472=ORIENTED_EDGE('',*,*,#21559,.T.);
#30473=ORIENTED_EDGE('',*,*,#21560,.T.);
#30474=ORIENTED_EDGE('',*,*,#21561,.T.);
#30475=ORIENTED_EDGE('',*,*,#21544,.T.);
#30476=ORIENTED_EDGE('',*,*,#21562,.T.);
#30477=ORIENTED_EDGE('',*,*,#21560,.F.);
#30478=ORIENTED_EDGE('',*,*,#21563,.F.);
#30479=ORIENTED_EDGE('',*,*,#21564,.F.);
#30480=ORIENTED_EDGE('',*,*,#21565,.T.);
#30481=ORIENTED_EDGE('',*,*,#21559,.F.);
#30482=ORIENTED_EDGE('',*,*,#21566,.F.);
#30483=ORIENTED_EDGE('',*,*,#21567,.T.);
#30484=ORIENTED_EDGE('',*,*,#21568,.F.);
#30485=ORIENTED_EDGE('',*,*,#21569,.F.);
#30486=ORIENTED_EDGE('',*,*,#21563,.T.);
#30487=ORIENTED_EDGE('',*,*,#21570,.T.);
#30488=ORIENTED_EDGE('',*,*,#21542,.T.);
#30489=ORIENTED_EDGE('',*,*,#21571,.T.);
#30490=ORIENTED_EDGE('',*,*,#21564,.T.);
#30491=ORIENTED_EDGE('',*,*,#21569,.T.);
#30492=ORIENTED_EDGE('',*,*,#21555,.T.);
#30493=ORIENTED_EDGE('',*,*,#21558,.T.);
#30494=ORIENTED_EDGE('',*,*,#21572,.T.);
#30495=ORIENTED_EDGE('',*,*,#21540,.T.);
#30496=ORIENTED_EDGE('',*,*,#21553,.T.);
#30497=ORIENTED_EDGE('',*,*,#21551,.F.);
#30498=ORIENTED_EDGE('',*,*,#21556,.F.);
#30499=ORIENTED_EDGE('',*,*,#21562,.F.);
#30500=ORIENTED_EDGE('',*,*,#21543,.T.);
#30501=ORIENTED_EDGE('',*,*,#21570,.F.);
#30502=ORIENTED_EDGE('',*,*,#21568,.T.);
#30503=ORIENTED_EDGE('',*,*,#21573,.T.);
#30504=ORIENTED_EDGE('',*,*,#21566,.T.);
#30505=ORIENTED_EDGE('',*,*,#21573,.F.);
#30506=ORIENTED_EDGE('',*,*,#21567,.F.);
#30507=ORIENTED_EDGE('',*,*,#21541,.F.);
#30508=ORIENTED_EDGE('',*,*,#21572,.F.);
#30509=ORIENTED_EDGE('',*,*,#21557,.F.);
#30510=ORIENTED_EDGE('',*,*,#21547,.F.);
#30511=ORIENTED_EDGE('',*,*,#21537,.F.);
#30512=ORIENTED_EDGE('',*,*,#21545,.F.);
#30513=ORIENTED_EDGE('',*,*,#21561,.F.);
#30514=ORIENTED_EDGE('',*,*,#21565,.F.);
#30515=ORIENTED_EDGE('',*,*,#21571,.F.);
#30516=ORIENTED_EDGE('',*,*,#21574,.F.);
#30517=ORIENTED_EDGE('',*,*,#21575,.T.);
#30518=ORIENTED_EDGE('',*,*,#21574,.T.);
#30519=ORIENTED_EDGE('',*,*,#21575,.F.);
#30520=ORIENTED_EDGE('',*,*,#21576,.F.);
#30521=ORIENTED_EDGE('',*,*,#21533,.F.);
#30522=ORIENTED_EDGE('',*,*,#21535,.F.);
#30523=ORIENTED_EDGE('',*,*,#21530,.F.);
#30524=ORIENTED_EDGE('',*,*,#21534,.F.);
#30525=ORIENTED_EDGE('',*,*,#21576,.T.);
#30526=ORIENTED_EDGE('',*,*,#21577,.T.);
#30527=ORIENTED_EDGE('',*,*,#21578,.T.);
#30528=ORIENTED_EDGE('',*,*,#21579,.T.);
#30529=ORIENTED_EDGE('',*,*,#21580,.T.);
#30530=ORIENTED_EDGE('',*,*,#21581,.T.);
#30531=ORIENTED_EDGE('',*,*,#21579,.F.);
#30532=ORIENTED_EDGE('',*,*,#21580,.F.);
#30533=ORIENTED_EDGE('',*,*,#21581,.F.);
#30534=ORIENTED_EDGE('',*,*,#21582,.T.);
#30535=ORIENTED_EDGE('',*,*,#21583,.F.);
#30536=ORIENTED_EDGE('',*,*,#21584,.F.);
#30537=ORIENTED_EDGE('',*,*,#21582,.F.);
#30538=ORIENTED_EDGE('',*,*,#21585,.F.);
#30539=ORIENTED_EDGE('',*,*,#21586,.T.);
#30540=ORIENTED_EDGE('',*,*,#21577,.F.);
#30541=ORIENTED_EDGE('',*,*,#21578,.F.);
#30542=ORIENTED_EDGE('',*,*,#21586,.F.);
#30543=ORIENTED_EDGE('',*,*,#21583,.T.);
#30544=ORIENTED_EDGE('',*,*,#21584,.T.);
#30545=ORIENTED_EDGE('',*,*,#21587,.T.);
#30546=ORIENTED_EDGE('',*,*,#21588,.T.);
#30547=ORIENTED_EDGE('',*,*,#21589,.T.);
#30548=ORIENTED_EDGE('',*,*,#21587,.F.);
#30549=ORIENTED_EDGE('',*,*,#21588,.F.);
#30550=ORIENTED_EDGE('',*,*,#21589,.F.);
#30551=ORIENTED_EDGE('',*,*,#21590,.T.);
#30552=ORIENTED_EDGE('',*,*,#21591,.F.);
#30553=ORIENTED_EDGE('',*,*,#21592,.F.);
#30554=ORIENTED_EDGE('',*,*,#21590,.F.);
#30555=ORIENTED_EDGE('',*,*,#21591,.T.);
#30556=ORIENTED_EDGE('',*,*,#21592,.T.);
#30557=ORIENTED_EDGE('',*,*,#21593,.T.);
#30558=ORIENTED_EDGE('',*,*,#21594,.T.);
#30559=ORIENTED_EDGE('',*,*,#21595,.T.);
#30560=ORIENTED_EDGE('',*,*,#21593,.F.);
#30561=ORIENTED_EDGE('',*,*,#21594,.F.);
#30562=ORIENTED_EDGE('',*,*,#21595,.F.);
#30563=ORIENTED_EDGE('',*,*,#21596,.T.);
#30564=ORIENTED_EDGE('',*,*,#21597,.F.);
#30565=ORIENTED_EDGE('',*,*,#21598,.F.);
#30566=ORIENTED_EDGE('',*,*,#21596,.F.);
#30567=ORIENTED_EDGE('',*,*,#21597,.T.);
#30568=ORIENTED_EDGE('',*,*,#21598,.T.);
#30569=ORIENTED_EDGE('',*,*,#21599,.T.);
#30570=ORIENTED_EDGE('',*,*,#21600,.T.);
#30571=ORIENTED_EDGE('',*,*,#21601,.T.);
#30572=ORIENTED_EDGE('',*,*,#21599,.F.);
#30573=ORIENTED_EDGE('',*,*,#21600,.F.);
#30574=ORIENTED_EDGE('',*,*,#21601,.F.);
#30575=ORIENTED_EDGE('',*,*,#21602,.T.);
#30576=ORIENTED_EDGE('',*,*,#21603,.T.);
#30577=ORIENTED_EDGE('',*,*,#21602,.F.);
#30578=ORIENTED_EDGE('',*,*,#21604,.F.);
#30579=ORIENTED_EDGE('',*,*,#21605,.T.);
#30580=ORIENTED_EDGE('',*,*,#21606,.F.);
#30581=ORIENTED_EDGE('',*,*,#21607,.T.);
#30582=ORIENTED_EDGE('',*,*,#21604,.T.);
#30583=ORIENTED_EDGE('',*,*,#21607,.F.);
#30584=ORIENTED_EDGE('',*,*,#21608,.F.);
#30585=ORIENTED_EDGE('',*,*,#21609,.T.);
#30586=ORIENTED_EDGE('',*,*,#21606,.T.);
#30587=ORIENTED_EDGE('',*,*,#21609,.F.);
#30588=ORIENTED_EDGE('',*,*,#21610,.F.);
#30589=ORIENTED_EDGE('',*,*,#21608,.T.);
#30590=ORIENTED_EDGE('',*,*,#21611,.F.);
#30591=ORIENTED_EDGE('',*,*,#21612,.T.);
#30592=ORIENTED_EDGE('',*,*,#21610,.T.);
#30593=ORIENTED_EDGE('',*,*,#21612,.F.);
#30594=ORIENTED_EDGE('',*,*,#21603,.F.);
#30595=ORIENTED_EDGE('',*,*,#21613,.T.);
#30596=ORIENTED_EDGE('',*,*,#21611,.T.);
#30597=ORIENTED_EDGE('',*,*,#21613,.F.);
#30598=ORIENTED_EDGE('',*,*,#21585,.T.);
#30599=ORIENTED_EDGE('',*,*,#21614,.F.);
#30600=ORIENTED_EDGE('',*,*,#21614,.T.);
#30601=ORIENTED_EDGE('',*,*,#21615,.T.);
#30602=ORIENTED_EDGE('',*,*,#21616,.F.);
#30603=ORIENTED_EDGE('',*,*,#21615,.F.);
#30604=ORIENTED_EDGE('',*,*,#21616,.T.);
#30605=ORIENTED_EDGE('',*,*,#21617,.T.);
#30606=ORIENTED_EDGE('',*,*,#21618,.F.);
#30607=ORIENTED_EDGE('',*,*,#21617,.F.);
#30608=ORIENTED_EDGE('',*,*,#21618,.T.);
#30609=ORIENTED_EDGE('',*,*,#21619,.T.);
#30610=ORIENTED_EDGE('',*,*,#21620,.F.);
#30611=ORIENTED_EDGE('',*,*,#21619,.F.);
#30612=ORIENTED_EDGE('',*,*,#21620,.T.);
#30613=ORIENTED_EDGE('',*,*,#21621,.T.);
#30614=ORIENTED_EDGE('',*,*,#21622,.F.);
#30615=ORIENTED_EDGE('',*,*,#21621,.F.);
#30616=ORIENTED_EDGE('',*,*,#21622,.T.);
#30617=ORIENTED_EDGE('',*,*,#21623,.T.);
#30618=ORIENTED_EDGE('',*,*,#21624,.F.);
#30619=ORIENTED_EDGE('',*,*,#21623,.F.);
#30620=ORIENTED_EDGE('',*,*,#21624,.T.);
#30621=ORIENTED_EDGE('',*,*,#21625,.T.);
#30622=ORIENTED_EDGE('',*,*,#21605,.F.);
#30623=ORIENTED_EDGE('',*,*,#21625,.F.);
#30624=ORIENTED_EDGE('',*,*,#21626,.F.);
#30625=ORIENTED_EDGE('',*,*,#21627,.T.);
#30626=ORIENTED_EDGE('',*,*,#21628,.T.);
#30627=ORIENTED_EDGE('',*,*,#21629,.T.);
#30628=ORIENTED_EDGE('',*,*,#21630,.F.);
#30629=ORIENTED_EDGE('',*,*,#21631,.T.);
#30630=ORIENTED_EDGE('',*,*,#21626,.T.);
#30631=ORIENTED_EDGE('',*,*,#21632,.T.);
#30632=ORIENTED_EDGE('',*,*,#21633,.F.);
#30633=ORIENTED_EDGE('',*,*,#21634,.T.);
#30634=ORIENTED_EDGE('',*,*,#21630,.T.);
#30635=ORIENTED_EDGE('',*,*,#21635,.T.);
#30636=ORIENTED_EDGE('',*,*,#21636,.F.);
#30637=ORIENTED_EDGE('',*,*,#21637,.T.);
#30638=ORIENTED_EDGE('',*,*,#21633,.T.);
#30639=ORIENTED_EDGE('',*,*,#21638,.T.);
#30640=ORIENTED_EDGE('',*,*,#21639,.F.);
#30641=ORIENTED_EDGE('',*,*,#21640,.T.);
#30642=ORIENTED_EDGE('',*,*,#21636,.T.);
#30643=ORIENTED_EDGE('',*,*,#21641,.T.);
#30644=ORIENTED_EDGE('',*,*,#21642,.F.);
#30645=ORIENTED_EDGE('',*,*,#21643,.T.);
#30646=ORIENTED_EDGE('',*,*,#21639,.T.);
#30647=ORIENTED_EDGE('',*,*,#21644,.T.);
#30648=ORIENTED_EDGE('',*,*,#21645,.F.);
#30649=ORIENTED_EDGE('',*,*,#21646,.T.);
#30650=ORIENTED_EDGE('',*,*,#21642,.T.);
#30651=ORIENTED_EDGE('',*,*,#21647,.T.);
#30652=ORIENTED_EDGE('',*,*,#21648,.F.);
#30653=ORIENTED_EDGE('',*,*,#21649,.T.);
#30654=ORIENTED_EDGE('',*,*,#21645,.T.);
#30655=ORIENTED_EDGE('',*,*,#21650,.T.);
#30656=ORIENTED_EDGE('',*,*,#21651,.F.);
#30657=ORIENTED_EDGE('',*,*,#21652,.T.);
#30658=ORIENTED_EDGE('',*,*,#21648,.T.);
#30659=ORIENTED_EDGE('',*,*,#21653,.T.);
#30660=ORIENTED_EDGE('',*,*,#21654,.F.);
#30661=ORIENTED_EDGE('',*,*,#21655,.T.);
#30662=ORIENTED_EDGE('',*,*,#21651,.T.);
#30663=ORIENTED_EDGE('',*,*,#21656,.T.);
#30664=ORIENTED_EDGE('',*,*,#21657,.F.);
#30665=ORIENTED_EDGE('',*,*,#21658,.T.);
#30666=ORIENTED_EDGE('',*,*,#21654,.T.);
#30667=ORIENTED_EDGE('',*,*,#21659,.T.);
#30668=ORIENTED_EDGE('',*,*,#21660,.F.);
#30669=ORIENTED_EDGE('',*,*,#21661,.T.);
#30670=ORIENTED_EDGE('',*,*,#21657,.T.);
#30671=ORIENTED_EDGE('',*,*,#21662,.T.);
#30672=ORIENTED_EDGE('',*,*,#21663,.F.);
#30673=ORIENTED_EDGE('',*,*,#21664,.T.);
#30674=ORIENTED_EDGE('',*,*,#21660,.T.);
#30675=ORIENTED_EDGE('',*,*,#21665,.T.);
#30676=ORIENTED_EDGE('',*,*,#21666,.F.);
#30677=ORIENTED_EDGE('',*,*,#21667,.T.);
#30678=ORIENTED_EDGE('',*,*,#21663,.T.);
#30679=ORIENTED_EDGE('',*,*,#21668,.T.);
#30680=ORIENTED_EDGE('',*,*,#21669,.F.);
#30681=ORIENTED_EDGE('',*,*,#21670,.T.);
#30682=ORIENTED_EDGE('',*,*,#21666,.T.);
#30683=ORIENTED_EDGE('',*,*,#21671,.T.);
#30684=ORIENTED_EDGE('',*,*,#21672,.F.);
#30685=ORIENTED_EDGE('',*,*,#21673,.T.);
#30686=ORIENTED_EDGE('',*,*,#21669,.T.);
#30687=ORIENTED_EDGE('',*,*,#21674,.T.);
#30688=ORIENTED_EDGE('',*,*,#21675,.F.);
#30689=ORIENTED_EDGE('',*,*,#21676,.T.);
#30690=ORIENTED_EDGE('',*,*,#21672,.T.);
#30691=ORIENTED_EDGE('',*,*,#21677,.T.);
#30692=ORIENTED_EDGE('',*,*,#21678,.F.);
#30693=ORIENTED_EDGE('',*,*,#21679,.T.);
#30694=ORIENTED_EDGE('',*,*,#21675,.T.);
#30695=ORIENTED_EDGE('',*,*,#21680,.T.);
#30696=ORIENTED_EDGE('',*,*,#21681,.F.);
#30697=ORIENTED_EDGE('',*,*,#21682,.T.);
#30698=ORIENTED_EDGE('',*,*,#21678,.T.);
#30699=ORIENTED_EDGE('',*,*,#21683,.T.);
#30700=ORIENTED_EDGE('',*,*,#21684,.F.);
#30701=ORIENTED_EDGE('',*,*,#21685,.T.);
#30702=ORIENTED_EDGE('',*,*,#21681,.T.);
#30703=ORIENTED_EDGE('',*,*,#21686,.T.);
#30704=ORIENTED_EDGE('',*,*,#21687,.F.);
#30705=ORIENTED_EDGE('',*,*,#21688,.T.);
#30706=ORIENTED_EDGE('',*,*,#21684,.T.);
#30707=ORIENTED_EDGE('',*,*,#21689,.T.);
#30708=ORIENTED_EDGE('',*,*,#21690,.F.);
#30709=ORIENTED_EDGE('',*,*,#21691,.T.);
#30710=ORIENTED_EDGE('',*,*,#21687,.T.);
#30711=ORIENTED_EDGE('',*,*,#21692,.T.);
#30712=ORIENTED_EDGE('',*,*,#21693,.F.);
#30713=ORIENTED_EDGE('',*,*,#21694,.T.);
#30714=ORIENTED_EDGE('',*,*,#21690,.T.);
#30715=ORIENTED_EDGE('',*,*,#21695,.T.);
#30716=ORIENTED_EDGE('',*,*,#21696,.F.);
#30717=ORIENTED_EDGE('',*,*,#21697,.T.);
#30718=ORIENTED_EDGE('',*,*,#21693,.T.);
#30719=ORIENTED_EDGE('',*,*,#21698,.T.);
#30720=ORIENTED_EDGE('',*,*,#21699,.F.);
#30721=ORIENTED_EDGE('',*,*,#21700,.T.);
#30722=ORIENTED_EDGE('',*,*,#21696,.T.);
#30723=ORIENTED_EDGE('',*,*,#21701,.T.);
#30724=ORIENTED_EDGE('',*,*,#21702,.F.);
#30725=ORIENTED_EDGE('',*,*,#21703,.T.);
#30726=ORIENTED_EDGE('',*,*,#21699,.T.);
#30727=ORIENTED_EDGE('',*,*,#21704,.T.);
#30728=ORIENTED_EDGE('',*,*,#21705,.F.);
#30729=ORIENTED_EDGE('',*,*,#21706,.T.);
#30730=ORIENTED_EDGE('',*,*,#21702,.T.);
#30731=ORIENTED_EDGE('',*,*,#21707,.T.);
#30732=ORIENTED_EDGE('',*,*,#21708,.F.);
#30733=ORIENTED_EDGE('',*,*,#21709,.T.);
#30734=ORIENTED_EDGE('',*,*,#21705,.T.);
#30735=ORIENTED_EDGE('',*,*,#21710,.T.);
#30736=ORIENTED_EDGE('',*,*,#21711,.F.);
#30737=ORIENTED_EDGE('',*,*,#21712,.T.);
#30738=ORIENTED_EDGE('',*,*,#21708,.T.);
#30739=ORIENTED_EDGE('',*,*,#21713,.T.);
#30740=ORIENTED_EDGE('',*,*,#21714,.F.);
#30741=ORIENTED_EDGE('',*,*,#21715,.T.);
#30742=ORIENTED_EDGE('',*,*,#21716,.F.);
#30743=ORIENTED_EDGE('',*,*,#21717,.F.);
#30744=ORIENTED_EDGE('',*,*,#21718,.T.);
#30745=ORIENTED_EDGE('',*,*,#21714,.T.);
#30746=ORIENTED_EDGE('',*,*,#21719,.F.);
#30747=ORIENTED_EDGE('',*,*,#21720,.F.);
#30748=ORIENTED_EDGE('',*,*,#21721,.F.);
#30749=ORIENTED_EDGE('',*,*,#21722,.T.);
#30750=ORIENTED_EDGE('',*,*,#21717,.T.);
#30751=ORIENTED_EDGE('',*,*,#21723,.F.);
#30752=ORIENTED_EDGE('',*,*,#21724,.F.);
#30753=ORIENTED_EDGE('',*,*,#21725,.T.);
#30754=ORIENTED_EDGE('',*,*,#21721,.T.);
#30755=ORIENTED_EDGE('',*,*,#21726,.F.);
#30756=ORIENTED_EDGE('',*,*,#21727,.F.);
#30757=ORIENTED_EDGE('',*,*,#21728,.T.);
#30758=ORIENTED_EDGE('',*,*,#21724,.T.);
#30759=ORIENTED_EDGE('',*,*,#21729,.F.);
#30760=ORIENTED_EDGE('',*,*,#21730,.F.);
#30761=ORIENTED_EDGE('',*,*,#21731,.T.);
#30762=ORIENTED_EDGE('',*,*,#21727,.T.);
#30763=ORIENTED_EDGE('',*,*,#21732,.F.);
#30764=ORIENTED_EDGE('',*,*,#21733,.F.);
#30765=ORIENTED_EDGE('',*,*,#21734,.T.);
#30766=ORIENTED_EDGE('',*,*,#21730,.T.);
#30767=ORIENTED_EDGE('',*,*,#21735,.F.);
#30768=ORIENTED_EDGE('',*,*,#21736,.F.);
#30769=ORIENTED_EDGE('',*,*,#21737,.T.);
#30770=ORIENTED_EDGE('',*,*,#21733,.T.);
#30771=ORIENTED_EDGE('',*,*,#21738,.F.);
#30772=ORIENTED_EDGE('',*,*,#21739,.F.);
#30773=ORIENTED_EDGE('',*,*,#21740,.T.);
#30774=ORIENTED_EDGE('',*,*,#21736,.T.);
#30775=ORIENTED_EDGE('',*,*,#21741,.F.);
#30776=ORIENTED_EDGE('',*,*,#21742,.F.);
#30777=ORIENTED_EDGE('',*,*,#21743,.T.);
#30778=ORIENTED_EDGE('',*,*,#21739,.T.);
#30779=ORIENTED_EDGE('',*,*,#21744,.F.);
#30780=ORIENTED_EDGE('',*,*,#21745,.F.);
#30781=ORIENTED_EDGE('',*,*,#21746,.T.);
#30782=ORIENTED_EDGE('',*,*,#21742,.T.);
#30783=ORIENTED_EDGE('',*,*,#21747,.F.);
#30784=ORIENTED_EDGE('',*,*,#21748,.F.);
#30785=ORIENTED_EDGE('',*,*,#21749,.T.);
#30786=ORIENTED_EDGE('',*,*,#21745,.T.);
#30787=ORIENTED_EDGE('',*,*,#21750,.F.);
#30788=ORIENTED_EDGE('',*,*,#21751,.F.);
#30789=ORIENTED_EDGE('',*,*,#21752,.T.);
#30790=ORIENTED_EDGE('',*,*,#21748,.T.);
#30791=ORIENTED_EDGE('',*,*,#21753,.F.);
#30792=ORIENTED_EDGE('',*,*,#21754,.F.);
#30793=ORIENTED_EDGE('',*,*,#21755,.T.);
#30794=ORIENTED_EDGE('',*,*,#21751,.T.);
#30795=ORIENTED_EDGE('',*,*,#21756,.F.);
#30796=ORIENTED_EDGE('',*,*,#21757,.F.);
#30797=ORIENTED_EDGE('',*,*,#21758,.T.);
#30798=ORIENTED_EDGE('',*,*,#21754,.T.);
#30799=ORIENTED_EDGE('',*,*,#21759,.F.);
#30800=ORIENTED_EDGE('',*,*,#21760,.F.);
#30801=ORIENTED_EDGE('',*,*,#21761,.T.);
#30802=ORIENTED_EDGE('',*,*,#21757,.T.);
#30803=ORIENTED_EDGE('',*,*,#21762,.F.);
#30804=ORIENTED_EDGE('',*,*,#21763,.F.);
#30805=ORIENTED_EDGE('',*,*,#21764,.T.);
#30806=ORIENTED_EDGE('',*,*,#21760,.T.);
#30807=ORIENTED_EDGE('',*,*,#21765,.F.);
#30808=ORIENTED_EDGE('',*,*,#21766,.F.);
#30809=ORIENTED_EDGE('',*,*,#21767,.T.);
#30810=ORIENTED_EDGE('',*,*,#21763,.T.);
#30811=ORIENTED_EDGE('',*,*,#21768,.F.);
#30812=ORIENTED_EDGE('',*,*,#21769,.F.);
#30813=ORIENTED_EDGE('',*,*,#21770,.T.);
#30814=ORIENTED_EDGE('',*,*,#21766,.T.);
#30815=ORIENTED_EDGE('',*,*,#21771,.F.);
#30816=ORIENTED_EDGE('',*,*,#21772,.F.);
#30817=ORIENTED_EDGE('',*,*,#21773,.T.);
#30818=ORIENTED_EDGE('',*,*,#21769,.T.);
#30819=ORIENTED_EDGE('',*,*,#21774,.F.);
#30820=ORIENTED_EDGE('',*,*,#21775,.F.);
#30821=ORIENTED_EDGE('',*,*,#21776,.T.);
#30822=ORIENTED_EDGE('',*,*,#21772,.T.);
#30823=ORIENTED_EDGE('',*,*,#21777,.F.);
#30824=ORIENTED_EDGE('',*,*,#21778,.F.);
#30825=ORIENTED_EDGE('',*,*,#21779,.T.);
#30826=ORIENTED_EDGE('',*,*,#21775,.T.);
#30827=ORIENTED_EDGE('',*,*,#21780,.F.);
#30828=ORIENTED_EDGE('',*,*,#21781,.F.);
#30829=ORIENTED_EDGE('',*,*,#21782,.T.);
#30830=ORIENTED_EDGE('',*,*,#21778,.T.);
#30831=ORIENTED_EDGE('',*,*,#21783,.F.);
#30832=ORIENTED_EDGE('',*,*,#21784,.F.);
#30833=ORIENTED_EDGE('',*,*,#21785,.T.);
#30834=ORIENTED_EDGE('',*,*,#21781,.T.);
#30835=ORIENTED_EDGE('',*,*,#21786,.F.);
#30836=ORIENTED_EDGE('',*,*,#21787,.F.);
#30837=ORIENTED_EDGE('',*,*,#21788,.T.);
#30838=ORIENTED_EDGE('',*,*,#21784,.T.);
#30839=ORIENTED_EDGE('',*,*,#21789,.F.);
#30840=ORIENTED_EDGE('',*,*,#21790,.F.);
#30841=ORIENTED_EDGE('',*,*,#21791,.T.);
#30842=ORIENTED_EDGE('',*,*,#21787,.T.);
#30843=ORIENTED_EDGE('',*,*,#21792,.F.);
#30844=ORIENTED_EDGE('',*,*,#21793,.F.);
#30845=ORIENTED_EDGE('',*,*,#21794,.T.);
#30846=ORIENTED_EDGE('',*,*,#21790,.T.);
#30847=ORIENTED_EDGE('',*,*,#21795,.F.);
#30848=ORIENTED_EDGE('',*,*,#21796,.F.);
#30849=ORIENTED_EDGE('',*,*,#21797,.T.);
#30850=ORIENTED_EDGE('',*,*,#21793,.T.);
#30851=ORIENTED_EDGE('',*,*,#21798,.F.);
#30852=ORIENTED_EDGE('',*,*,#21799,.F.);
#30853=ORIENTED_EDGE('',*,*,#21800,.T.);
#30854=ORIENTED_EDGE('',*,*,#21796,.T.);
#30855=ORIENTED_EDGE('',*,*,#21801,.F.);
#30856=ORIENTED_EDGE('',*,*,#21802,.T.);
#30857=ORIENTED_EDGE('',*,*,#21803,.T.);
#30858=ORIENTED_EDGE('',*,*,#21804,.T.);
#30859=ORIENTED_EDGE('',*,*,#21805,.T.);
#30860=ORIENTED_EDGE('',*,*,#21803,.F.);
#30861=ORIENTED_EDGE('',*,*,#21804,.F.);
#30862=ORIENTED_EDGE('',*,*,#21805,.F.);
#30863=ORIENTED_EDGE('',*,*,#21806,.T.);
#30864=ORIENTED_EDGE('',*,*,#21807,.T.);
#30865=ORIENTED_EDGE('',*,*,#21808,.T.);
#30866=ORIENTED_EDGE('',*,*,#21809,.T.);
#30867=ORIENTED_EDGE('',*,*,#21806,.F.);
#30868=ORIENTED_EDGE('',*,*,#21802,.F.);
#30869=ORIENTED_EDGE('',*,*,#21810,.T.);
#30870=ORIENTED_EDGE('',*,*,#21811,.T.);
#30871=ORIENTED_EDGE('',*,*,#21812,.T.);
#30872=ORIENTED_EDGE('',*,*,#21813,.T.);
#30873=ORIENTED_EDGE('',*,*,#21814,.T.);
#30874=ORIENTED_EDGE('',*,*,#21815,.T.);
#30875=ORIENTED_EDGE('',*,*,#21811,.F.);
#30876=ORIENTED_EDGE('',*,*,#21816,.T.);
#30877=ORIENTED_EDGE('',*,*,#21817,.F.);
#30878=ORIENTED_EDGE('',*,*,#21815,.F.);
#30879=ORIENTED_EDGE('',*,*,#21818,.T.);
#30880=ORIENTED_EDGE('',*,*,#21819,.T.);
#30881=ORIENTED_EDGE('',*,*,#21820,.T.);
#30882=ORIENTED_EDGE('',*,*,#21821,.T.);
#30883=ORIENTED_EDGE('',*,*,#21822,.T.);
#30884=ORIENTED_EDGE('',*,*,#21821,.F.);
#30885=ORIENTED_EDGE('',*,*,#21823,.T.);
#30886=ORIENTED_EDGE('',*,*,#21824,.F.);
#30887=ORIENTED_EDGE('',*,*,#21825,.F.);
#30888=ORIENTED_EDGE('',*,*,#21820,.F.);
#30889=ORIENTED_EDGE('',*,*,#21826,.F.);
#30890=ORIENTED_EDGE('',*,*,#21827,.T.);
#30891=ORIENTED_EDGE('',*,*,#21828,.F.);
#30892=ORIENTED_EDGE('',*,*,#21829,.F.);
#30893=ORIENTED_EDGE('',*,*,#21823,.F.);
#30894=ORIENTED_EDGE('',*,*,#21819,.F.);
#30895=ORIENTED_EDGE('',*,*,#21830,.T.);
#30896=ORIENTED_EDGE('',*,*,#21831,.T.);
#30897=ORIENTED_EDGE('',*,*,#21828,.T.);
#30898=ORIENTED_EDGE('',*,*,#21832,.T.);
#30899=ORIENTED_EDGE('',*,*,#21826,.T.);
#30900=ORIENTED_EDGE('',*,*,#21814,.F.);
#30901=ORIENTED_EDGE('',*,*,#21833,.F.);
#30902=ORIENTED_EDGE('',*,*,#21830,.F.);
#30903=ORIENTED_EDGE('',*,*,#21818,.F.);
#30904=ORIENTED_EDGE('',*,*,#21832,.F.);
#30905=ORIENTED_EDGE('',*,*,#21827,.F.);
#30906=ORIENTED_EDGE('',*,*,#21813,.F.);
#30907=ORIENTED_EDGE('',*,*,#21834,.T.);
#30908=ORIENTED_EDGE('',*,*,#21824,.T.);
#30909=ORIENTED_EDGE('',*,*,#21829,.T.);
#30910=ORIENTED_EDGE('',*,*,#21831,.F.);
#30911=ORIENTED_EDGE('',*,*,#21833,.T.);
#30912=ORIENTED_EDGE('',*,*,#21812,.F.);
#30913=ORIENTED_EDGE('',*,*,#21816,.F.);
#30914=ORIENTED_EDGE('',*,*,#21810,.F.);
#30915=ORIENTED_EDGE('',*,*,#21822,.F.);
#30916=ORIENTED_EDGE('',*,*,#21825,.T.);
#30917=ORIENTED_EDGE('',*,*,#21834,.F.);
#30918=ORIENTED_EDGE('',*,*,#21719,.T.);
#30919=ORIENTED_EDGE('',*,*,#21716,.T.);
#30920=ORIENTED_EDGE('',*,*,#21835,.T.);
#30921=ORIENTED_EDGE('',*,*,#21807,.F.);
#30922=ORIENTED_EDGE('',*,*,#21809,.F.);
#30923=ORIENTED_EDGE('',*,*,#21836,.T.);
#30924=ORIENTED_EDGE('',*,*,#21836,.F.);
#30925=ORIENTED_EDGE('',*,*,#21837,.F.);
#30926=ORIENTED_EDGE('',*,*,#21713,.F.);
#30927=ORIENTED_EDGE('',*,*,#21710,.F.);
#30928=ORIENTED_EDGE('',*,*,#21707,.F.);
#30929=ORIENTED_EDGE('',*,*,#21704,.F.);
#30930=ORIENTED_EDGE('',*,*,#21701,.F.);
#30931=ORIENTED_EDGE('',*,*,#21698,.F.);
#30932=ORIENTED_EDGE('',*,*,#21695,.F.);
#30933=ORIENTED_EDGE('',*,*,#21692,.F.);
#30934=ORIENTED_EDGE('',*,*,#21689,.F.);
#30935=ORIENTED_EDGE('',*,*,#21686,.F.);
#30936=ORIENTED_EDGE('',*,*,#21683,.F.);
#30937=ORIENTED_EDGE('',*,*,#21680,.F.);
#30938=ORIENTED_EDGE('',*,*,#21677,.F.);
#30939=ORIENTED_EDGE('',*,*,#21674,.F.);
#30940=ORIENTED_EDGE('',*,*,#21671,.F.);
#30941=ORIENTED_EDGE('',*,*,#21668,.F.);
#30942=ORIENTED_EDGE('',*,*,#21665,.F.);
#30943=ORIENTED_EDGE('',*,*,#21662,.F.);
#30944=ORIENTED_EDGE('',*,*,#21659,.F.);
#30945=ORIENTED_EDGE('',*,*,#21656,.F.);
#30946=ORIENTED_EDGE('',*,*,#21653,.F.);
#30947=ORIENTED_EDGE('',*,*,#21650,.F.);
#30948=ORIENTED_EDGE('',*,*,#21647,.F.);
#30949=ORIENTED_EDGE('',*,*,#21644,.F.);
#30950=ORIENTED_EDGE('',*,*,#21641,.F.);
#30951=ORIENTED_EDGE('',*,*,#21638,.F.);
#30952=ORIENTED_EDGE('',*,*,#21635,.F.);
#30953=ORIENTED_EDGE('',*,*,#21632,.F.);
#30954=ORIENTED_EDGE('',*,*,#21629,.F.);
#30955=ORIENTED_EDGE('',*,*,#21838,.F.);
#30956=ORIENTED_EDGE('',*,*,#21839,.T.);
#30957=ORIENTED_EDGE('',*,*,#21801,.T.);
#30958=ORIENTED_EDGE('',*,*,#21798,.T.);
#30959=ORIENTED_EDGE('',*,*,#21795,.T.);
#30960=ORIENTED_EDGE('',*,*,#21792,.T.);
#30961=ORIENTED_EDGE('',*,*,#21789,.T.);
#30962=ORIENTED_EDGE('',*,*,#21786,.T.);
#30963=ORIENTED_EDGE('',*,*,#21783,.T.);
#30964=ORIENTED_EDGE('',*,*,#21780,.T.);
#30965=ORIENTED_EDGE('',*,*,#21777,.T.);
#30966=ORIENTED_EDGE('',*,*,#21774,.T.);
#30967=ORIENTED_EDGE('',*,*,#21771,.T.);
#30968=ORIENTED_EDGE('',*,*,#21768,.T.);
#30969=ORIENTED_EDGE('',*,*,#21765,.T.);
#30970=ORIENTED_EDGE('',*,*,#21762,.T.);
#30971=ORIENTED_EDGE('',*,*,#21759,.T.);
#30972=ORIENTED_EDGE('',*,*,#21756,.T.);
#30973=ORIENTED_EDGE('',*,*,#21753,.T.);
#30974=ORIENTED_EDGE('',*,*,#21750,.T.);
#30975=ORIENTED_EDGE('',*,*,#21747,.T.);
#30976=ORIENTED_EDGE('',*,*,#21744,.T.);
#30977=ORIENTED_EDGE('',*,*,#21741,.T.);
#30978=ORIENTED_EDGE('',*,*,#21738,.T.);
#30979=ORIENTED_EDGE('',*,*,#21735,.T.);
#30980=ORIENTED_EDGE('',*,*,#21732,.T.);
#30981=ORIENTED_EDGE('',*,*,#21729,.T.);
#30982=ORIENTED_EDGE('',*,*,#21726,.T.);
#30983=ORIENTED_EDGE('',*,*,#21723,.T.);
#30984=ORIENTED_EDGE('',*,*,#21720,.T.);
#30985=ORIENTED_EDGE('',*,*,#21840,.T.);
#30986=ORIENTED_EDGE('',*,*,#21841,.T.);
#30987=ORIENTED_EDGE('',*,*,#21842,.T.);
#30988=ORIENTED_EDGE('',*,*,#21843,.T.);
#30989=ORIENTED_EDGE('',*,*,#21838,.T.);
#30990=ORIENTED_EDGE('',*,*,#21799,.T.);
#30991=ORIENTED_EDGE('',*,*,#21839,.F.);
#30992=ORIENTED_EDGE('',*,*,#21843,.F.);
#30993=ORIENTED_EDGE('',*,*,#21844,.T.);
#30994=ORIENTED_EDGE('',*,*,#21835,.F.);
#30995=ORIENTED_EDGE('',*,*,#21715,.F.);
#30996=ORIENTED_EDGE('',*,*,#21718,.F.);
#30997=ORIENTED_EDGE('',*,*,#21722,.F.);
#30998=ORIENTED_EDGE('',*,*,#21725,.F.);
#30999=ORIENTED_EDGE('',*,*,#21728,.F.);
#31000=ORIENTED_EDGE('',*,*,#21731,.F.);
#31001=ORIENTED_EDGE('',*,*,#21734,.F.);
#31002=ORIENTED_EDGE('',*,*,#21737,.F.);
#31003=ORIENTED_EDGE('',*,*,#21740,.F.);
#31004=ORIENTED_EDGE('',*,*,#21743,.F.);
#31005=ORIENTED_EDGE('',*,*,#21746,.F.);
#31006=ORIENTED_EDGE('',*,*,#21749,.F.);
#31007=ORIENTED_EDGE('',*,*,#21752,.F.);
#31008=ORIENTED_EDGE('',*,*,#21755,.F.);
#31009=ORIENTED_EDGE('',*,*,#21758,.F.);
#31010=ORIENTED_EDGE('',*,*,#21761,.F.);
#31011=ORIENTED_EDGE('',*,*,#21764,.F.);
#31012=ORIENTED_EDGE('',*,*,#21767,.F.);
#31013=ORIENTED_EDGE('',*,*,#21770,.F.);
#31014=ORIENTED_EDGE('',*,*,#21773,.F.);
#31015=ORIENTED_EDGE('',*,*,#21776,.F.);
#31016=ORIENTED_EDGE('',*,*,#21779,.F.);
#31017=ORIENTED_EDGE('',*,*,#21782,.F.);
#31018=ORIENTED_EDGE('',*,*,#21785,.F.);
#31019=ORIENTED_EDGE('',*,*,#21788,.F.);
#31020=ORIENTED_EDGE('',*,*,#21791,.F.);
#31021=ORIENTED_EDGE('',*,*,#21794,.F.);
#31022=ORIENTED_EDGE('',*,*,#21797,.F.);
#31023=ORIENTED_EDGE('',*,*,#21800,.F.);
#31024=ORIENTED_EDGE('',*,*,#21844,.F.);
#31025=ORIENTED_EDGE('',*,*,#21842,.F.);
#31026=ORIENTED_EDGE('',*,*,#21627,.F.);
#31027=ORIENTED_EDGE('',*,*,#21631,.F.);
#31028=ORIENTED_EDGE('',*,*,#21634,.F.);
#31029=ORIENTED_EDGE('',*,*,#21637,.F.);
#31030=ORIENTED_EDGE('',*,*,#21640,.F.);
#31031=ORIENTED_EDGE('',*,*,#21643,.F.);
#31032=ORIENTED_EDGE('',*,*,#21646,.F.);
#31033=ORIENTED_EDGE('',*,*,#21649,.F.);
#31034=ORIENTED_EDGE('',*,*,#21652,.F.);
#31035=ORIENTED_EDGE('',*,*,#21655,.F.);
#31036=ORIENTED_EDGE('',*,*,#21658,.F.);
#31037=ORIENTED_EDGE('',*,*,#21661,.F.);
#31038=ORIENTED_EDGE('',*,*,#21664,.F.);
#31039=ORIENTED_EDGE('',*,*,#21667,.F.);
#31040=ORIENTED_EDGE('',*,*,#21670,.F.);
#31041=ORIENTED_EDGE('',*,*,#21673,.F.);
#31042=ORIENTED_EDGE('',*,*,#21676,.F.);
#31043=ORIENTED_EDGE('',*,*,#21679,.F.);
#31044=ORIENTED_EDGE('',*,*,#21682,.F.);
#31045=ORIENTED_EDGE('',*,*,#21685,.F.);
#31046=ORIENTED_EDGE('',*,*,#21688,.F.);
#31047=ORIENTED_EDGE('',*,*,#21691,.F.);
#31048=ORIENTED_EDGE('',*,*,#21694,.F.);
#31049=ORIENTED_EDGE('',*,*,#21697,.F.);
#31050=ORIENTED_EDGE('',*,*,#21700,.F.);
#31051=ORIENTED_EDGE('',*,*,#21703,.F.);
#31052=ORIENTED_EDGE('',*,*,#21706,.F.);
#31053=ORIENTED_EDGE('',*,*,#21709,.F.);
#31054=ORIENTED_EDGE('',*,*,#21712,.F.);
#31055=ORIENTED_EDGE('',*,*,#21845,.F.);
#31056=ORIENTED_EDGE('',*,*,#21711,.T.);
#31057=ORIENTED_EDGE('',*,*,#21837,.T.);
#31058=ORIENTED_EDGE('',*,*,#21808,.F.);
#31059=ORIENTED_EDGE('',*,*,#21845,.T.);
#31060=ORIENTED_EDGE('',*,*,#21846,.F.);
#31061=ORIENTED_EDGE('',*,*,#21847,.T.);
#31062=ORIENTED_EDGE('',*,*,#21848,.F.);
#31063=ORIENTED_EDGE('',*,*,#21849,.F.);
#31064=ORIENTED_EDGE('',*,*,#21850,.F.);
#31065=ORIENTED_EDGE('',*,*,#21849,.T.);
#31066=ORIENTED_EDGE('',*,*,#21851,.T.);
#31067=ORIENTED_EDGE('',*,*,#21852,.F.);
#31068=ORIENTED_EDGE('',*,*,#21851,.F.);
#31069=ORIENTED_EDGE('',*,*,#21848,.T.);
#31070=ORIENTED_EDGE('',*,*,#21853,.T.);
#31071=ORIENTED_EDGE('',*,*,#21854,.F.);
#31072=ORIENTED_EDGE('',*,*,#21853,.F.);
#31073=ORIENTED_EDGE('',*,*,#21847,.F.);
#31074=ORIENTED_EDGE('',*,*,#21855,.F.);
#31075=ORIENTED_EDGE('',*,*,#21856,.T.);
#31076=ORIENTED_EDGE('',*,*,#21857,.F.);
#31077=ORIENTED_EDGE('',*,*,#21858,.F.);
#31078=ORIENTED_EDGE('',*,*,#21859,.F.);
#31079=ORIENTED_EDGE('',*,*,#21858,.T.);
#31080=ORIENTED_EDGE('',*,*,#21860,.T.);
#31081=ORIENTED_EDGE('',*,*,#21861,.F.);
#31082=ORIENTED_EDGE('',*,*,#21860,.F.);
#31083=ORIENTED_EDGE('',*,*,#21857,.T.);
#31084=ORIENTED_EDGE('',*,*,#21862,.T.);
#31085=ORIENTED_EDGE('',*,*,#21863,.F.);
#31086=ORIENTED_EDGE('',*,*,#21862,.F.);
#31087=ORIENTED_EDGE('',*,*,#21856,.F.);
#31088=ORIENTED_EDGE('',*,*,#21864,.F.);
#31089=ORIENTED_EDGE('',*,*,#21865,.T.);
#31090=ORIENTED_EDGE('',*,*,#21866,.F.);
#31091=ORIENTED_EDGE('',*,*,#21867,.F.);
#31092=ORIENTED_EDGE('',*,*,#21868,.F.);
#31093=ORIENTED_EDGE('',*,*,#21867,.T.);
#31094=ORIENTED_EDGE('',*,*,#21869,.T.);
#31095=ORIENTED_EDGE('',*,*,#21870,.F.);
#31096=ORIENTED_EDGE('',*,*,#21869,.F.);
#31097=ORIENTED_EDGE('',*,*,#21866,.T.);
#31098=ORIENTED_EDGE('',*,*,#21871,.T.);
#31099=ORIENTED_EDGE('',*,*,#21872,.F.);
#31100=ORIENTED_EDGE('',*,*,#21871,.F.);
#31101=ORIENTED_EDGE('',*,*,#21865,.F.);
#31102=ORIENTED_EDGE('',*,*,#21873,.F.);
#31103=ORIENTED_EDGE('',*,*,#21874,.T.);
#31104=ORIENTED_EDGE('',*,*,#21875,.F.);
#31105=ORIENTED_EDGE('',*,*,#21876,.F.);
#31106=ORIENTED_EDGE('',*,*,#21877,.F.);
#31107=ORIENTED_EDGE('',*,*,#21876,.T.);
#31108=ORIENTED_EDGE('',*,*,#21878,.T.);
#31109=ORIENTED_EDGE('',*,*,#21879,.F.);
#31110=ORIENTED_EDGE('',*,*,#21878,.F.);
#31111=ORIENTED_EDGE('',*,*,#21875,.T.);
#31112=ORIENTED_EDGE('',*,*,#21880,.T.);
#31113=ORIENTED_EDGE('',*,*,#21881,.F.);
#31114=ORIENTED_EDGE('',*,*,#21880,.F.);
#31115=ORIENTED_EDGE('',*,*,#21874,.F.);
#31116=ORIENTED_EDGE('',*,*,#21882,.F.);
#31117=ORIENTED_EDGE('',*,*,#21883,.T.);
#31118=ORIENTED_EDGE('',*,*,#21884,.F.);
#31119=ORIENTED_EDGE('',*,*,#21885,.F.);
#31120=ORIENTED_EDGE('',*,*,#21886,.F.);
#31121=ORIENTED_EDGE('',*,*,#21885,.T.);
#31122=ORIENTED_EDGE('',*,*,#21887,.T.);
#31123=ORIENTED_EDGE('',*,*,#21888,.F.);
#31124=ORIENTED_EDGE('',*,*,#21887,.F.);
#31125=ORIENTED_EDGE('',*,*,#21884,.T.);
#31126=ORIENTED_EDGE('',*,*,#21889,.T.);
#31127=ORIENTED_EDGE('',*,*,#21890,.F.);
#31128=ORIENTED_EDGE('',*,*,#21889,.F.);
#31129=ORIENTED_EDGE('',*,*,#21883,.F.);
#31130=ORIENTED_EDGE('',*,*,#21891,.F.);
#31131=ORIENTED_EDGE('',*,*,#21892,.T.);
#31132=ORIENTED_EDGE('',*,*,#21893,.F.);
#31133=ORIENTED_EDGE('',*,*,#21894,.F.);
#31134=ORIENTED_EDGE('',*,*,#21895,.F.);
#31135=ORIENTED_EDGE('',*,*,#21894,.T.);
#31136=ORIENTED_EDGE('',*,*,#21896,.T.);
#31137=ORIENTED_EDGE('',*,*,#21897,.F.);
#31138=ORIENTED_EDGE('',*,*,#21896,.F.);
#31139=ORIENTED_EDGE('',*,*,#21893,.T.);
#31140=ORIENTED_EDGE('',*,*,#21898,.T.);
#31141=ORIENTED_EDGE('',*,*,#21899,.F.);
#31142=ORIENTED_EDGE('',*,*,#21898,.F.);
#31143=ORIENTED_EDGE('',*,*,#21892,.F.);
#31144=ORIENTED_EDGE('',*,*,#21900,.F.);
#31145=ORIENTED_EDGE('',*,*,#21901,.T.);
#31146=ORIENTED_EDGE('',*,*,#21902,.F.);
#31147=ORIENTED_EDGE('',*,*,#21903,.F.);
#31148=ORIENTED_EDGE('',*,*,#21904,.F.);
#31149=ORIENTED_EDGE('',*,*,#21903,.T.);
#31150=ORIENTED_EDGE('',*,*,#21905,.T.);
#31151=ORIENTED_EDGE('',*,*,#21906,.F.);
#31152=ORIENTED_EDGE('',*,*,#21905,.F.);
#31153=ORIENTED_EDGE('',*,*,#21902,.T.);
#31154=ORIENTED_EDGE('',*,*,#21907,.T.);
#31155=ORIENTED_EDGE('',*,*,#21908,.F.);
#31156=ORIENTED_EDGE('',*,*,#21907,.F.);
#31157=ORIENTED_EDGE('',*,*,#21901,.F.);
#31158=ORIENTED_EDGE('',*,*,#21909,.F.);
#31159=ORIENTED_EDGE('',*,*,#21910,.T.);
#31160=ORIENTED_EDGE('',*,*,#21911,.F.);
#31161=ORIENTED_EDGE('',*,*,#21912,.F.);
#31162=ORIENTED_EDGE('',*,*,#21913,.F.);
#31163=ORIENTED_EDGE('',*,*,#21912,.T.);
#31164=ORIENTED_EDGE('',*,*,#21914,.T.);
#31165=ORIENTED_EDGE('',*,*,#21915,.F.);
#31166=ORIENTED_EDGE('',*,*,#21914,.F.);
#31167=ORIENTED_EDGE('',*,*,#21911,.T.);
#31168=ORIENTED_EDGE('',*,*,#21916,.T.);
#31169=ORIENTED_EDGE('',*,*,#21917,.F.);
#31170=ORIENTED_EDGE('',*,*,#21916,.F.);
#31171=ORIENTED_EDGE('',*,*,#21910,.F.);
#31172=ORIENTED_EDGE('',*,*,#21918,.F.);
#31173=ORIENTED_EDGE('',*,*,#21919,.T.);
#31174=ORIENTED_EDGE('',*,*,#21920,.F.);
#31175=ORIENTED_EDGE('',*,*,#21921,.F.);
#31176=ORIENTED_EDGE('',*,*,#21922,.F.);
#31177=ORIENTED_EDGE('',*,*,#21921,.T.);
#31178=ORIENTED_EDGE('',*,*,#21923,.T.);
#31179=ORIENTED_EDGE('',*,*,#21924,.F.);
#31180=ORIENTED_EDGE('',*,*,#21923,.F.);
#31181=ORIENTED_EDGE('',*,*,#21920,.T.);
#31182=ORIENTED_EDGE('',*,*,#21925,.T.);
#31183=ORIENTED_EDGE('',*,*,#21926,.F.);
#31184=ORIENTED_EDGE('',*,*,#21925,.F.);
#31185=ORIENTED_EDGE('',*,*,#21919,.F.);
#31186=ORIENTED_EDGE('',*,*,#21927,.F.);
#31187=ORIENTED_EDGE('',*,*,#21928,.T.);
#31188=ORIENTED_EDGE('',*,*,#21929,.F.);
#31189=ORIENTED_EDGE('',*,*,#21930,.F.);
#31190=ORIENTED_EDGE('',*,*,#21931,.F.);
#31191=ORIENTED_EDGE('',*,*,#21930,.T.);
#31192=ORIENTED_EDGE('',*,*,#21932,.T.);
#31193=ORIENTED_EDGE('',*,*,#21933,.F.);
#31194=ORIENTED_EDGE('',*,*,#21932,.F.);
#31195=ORIENTED_EDGE('',*,*,#21929,.T.);
#31196=ORIENTED_EDGE('',*,*,#21934,.T.);
#31197=ORIENTED_EDGE('',*,*,#21935,.F.);
#31198=ORIENTED_EDGE('',*,*,#21934,.F.);
#31199=ORIENTED_EDGE('',*,*,#21928,.F.);
#31200=ORIENTED_EDGE('',*,*,#21936,.F.);
#31201=ORIENTED_EDGE('',*,*,#21937,.T.);
#31202=ORIENTED_EDGE('',*,*,#21938,.F.);
#31203=ORIENTED_EDGE('',*,*,#21939,.F.);
#31204=ORIENTED_EDGE('',*,*,#21940,.F.);
#31205=ORIENTED_EDGE('',*,*,#21939,.T.);
#31206=ORIENTED_EDGE('',*,*,#21941,.T.);
#31207=ORIENTED_EDGE('',*,*,#21942,.F.);
#31208=ORIENTED_EDGE('',*,*,#21941,.F.);
#31209=ORIENTED_EDGE('',*,*,#21938,.T.);
#31210=ORIENTED_EDGE('',*,*,#21943,.T.);
#31211=ORIENTED_EDGE('',*,*,#21944,.F.);
#31212=ORIENTED_EDGE('',*,*,#21943,.F.);
#31213=ORIENTED_EDGE('',*,*,#21937,.F.);
#31214=ORIENTED_EDGE('',*,*,#21945,.F.);
#31215=ORIENTED_EDGE('',*,*,#21946,.T.);
#31216=ORIENTED_EDGE('',*,*,#21947,.F.);
#31217=ORIENTED_EDGE('',*,*,#21948,.F.);
#31218=ORIENTED_EDGE('',*,*,#21949,.F.);
#31219=ORIENTED_EDGE('',*,*,#21948,.T.);
#31220=ORIENTED_EDGE('',*,*,#21950,.T.);
#31221=ORIENTED_EDGE('',*,*,#21951,.F.);
#31222=ORIENTED_EDGE('',*,*,#21950,.F.);
#31223=ORIENTED_EDGE('',*,*,#21947,.T.);
#31224=ORIENTED_EDGE('',*,*,#21952,.T.);
#31225=ORIENTED_EDGE('',*,*,#21953,.F.);
#31226=ORIENTED_EDGE('',*,*,#21952,.F.);
#31227=ORIENTED_EDGE('',*,*,#21946,.F.);
#31228=ORIENTED_EDGE('',*,*,#21954,.F.);
#31229=ORIENTED_EDGE('',*,*,#21955,.T.);
#31230=ORIENTED_EDGE('',*,*,#21956,.F.);
#31231=ORIENTED_EDGE('',*,*,#21957,.F.);
#31232=ORIENTED_EDGE('',*,*,#21958,.F.);
#31233=ORIENTED_EDGE('',*,*,#21957,.T.);
#31234=ORIENTED_EDGE('',*,*,#21959,.T.);
#31235=ORIENTED_EDGE('',*,*,#21960,.F.);
#31236=ORIENTED_EDGE('',*,*,#21959,.F.);
#31237=ORIENTED_EDGE('',*,*,#21956,.T.);
#31238=ORIENTED_EDGE('',*,*,#21961,.T.);
#31239=ORIENTED_EDGE('',*,*,#21962,.F.);
#31240=ORIENTED_EDGE('',*,*,#21961,.F.);
#31241=ORIENTED_EDGE('',*,*,#21955,.F.);
#31242=ORIENTED_EDGE('',*,*,#21963,.F.);
#31243=ORIENTED_EDGE('',*,*,#21964,.T.);
#31244=ORIENTED_EDGE('',*,*,#21965,.F.);
#31245=ORIENTED_EDGE('',*,*,#21966,.F.);
#31246=ORIENTED_EDGE('',*,*,#21967,.F.);
#31247=ORIENTED_EDGE('',*,*,#21966,.T.);
#31248=ORIENTED_EDGE('',*,*,#21968,.T.);
#31249=ORIENTED_EDGE('',*,*,#21969,.F.);
#31250=ORIENTED_EDGE('',*,*,#21968,.F.);
#31251=ORIENTED_EDGE('',*,*,#21965,.T.);
#31252=ORIENTED_EDGE('',*,*,#21970,.T.);
#31253=ORIENTED_EDGE('',*,*,#21971,.F.);
#31254=ORIENTED_EDGE('',*,*,#21970,.F.);
#31255=ORIENTED_EDGE('',*,*,#21964,.F.);
#31256=ORIENTED_EDGE('',*,*,#21972,.F.);
#31257=ORIENTED_EDGE('',*,*,#21973,.T.);
#31258=ORIENTED_EDGE('',*,*,#21974,.F.);
#31259=ORIENTED_EDGE('',*,*,#21975,.F.);
#31260=ORIENTED_EDGE('',*,*,#21976,.F.);
#31261=ORIENTED_EDGE('',*,*,#21975,.T.);
#31262=ORIENTED_EDGE('',*,*,#21977,.T.);
#31263=ORIENTED_EDGE('',*,*,#21978,.F.);
#31264=ORIENTED_EDGE('',*,*,#21977,.F.);
#31265=ORIENTED_EDGE('',*,*,#21974,.T.);
#31266=ORIENTED_EDGE('',*,*,#21979,.T.);
#31267=ORIENTED_EDGE('',*,*,#21980,.F.);
#31268=ORIENTED_EDGE('',*,*,#21979,.F.);
#31269=ORIENTED_EDGE('',*,*,#21973,.F.);
#31270=ORIENTED_EDGE('',*,*,#21981,.F.);
#31271=ORIENTED_EDGE('',*,*,#21982,.T.);
#31272=ORIENTED_EDGE('',*,*,#21983,.F.);
#31273=ORIENTED_EDGE('',*,*,#21984,.F.);
#31274=ORIENTED_EDGE('',*,*,#21985,.F.);
#31275=ORIENTED_EDGE('',*,*,#21984,.T.);
#31276=ORIENTED_EDGE('',*,*,#21986,.T.);
#31277=ORIENTED_EDGE('',*,*,#21987,.F.);
#31278=ORIENTED_EDGE('',*,*,#21986,.F.);
#31279=ORIENTED_EDGE('',*,*,#21983,.T.);
#31280=ORIENTED_EDGE('',*,*,#21988,.T.);
#31281=ORIENTED_EDGE('',*,*,#21989,.F.);
#31282=ORIENTED_EDGE('',*,*,#21988,.F.);
#31283=ORIENTED_EDGE('',*,*,#21982,.F.);
#31284=ORIENTED_EDGE('',*,*,#21990,.F.);
#31285=ORIENTED_EDGE('',*,*,#21991,.T.);
#31286=ORIENTED_EDGE('',*,*,#21992,.F.);
#31287=ORIENTED_EDGE('',*,*,#21993,.F.);
#31288=ORIENTED_EDGE('',*,*,#21994,.F.);
#31289=ORIENTED_EDGE('',*,*,#21993,.T.);
#31290=ORIENTED_EDGE('',*,*,#21995,.T.);
#31291=ORIENTED_EDGE('',*,*,#21996,.F.);
#31292=ORIENTED_EDGE('',*,*,#21995,.F.);
#31293=ORIENTED_EDGE('',*,*,#21992,.T.);
#31294=ORIENTED_EDGE('',*,*,#21997,.T.);
#31295=ORIENTED_EDGE('',*,*,#21998,.F.);
#31296=ORIENTED_EDGE('',*,*,#21997,.F.);
#31297=ORIENTED_EDGE('',*,*,#21991,.F.);
#31298=ORIENTED_EDGE('',*,*,#21999,.F.);
#31299=ORIENTED_EDGE('',*,*,#22000,.T.);
#31300=ORIENTED_EDGE('',*,*,#22001,.F.);
#31301=ORIENTED_EDGE('',*,*,#22002,.F.);
#31302=ORIENTED_EDGE('',*,*,#22003,.F.);
#31303=ORIENTED_EDGE('',*,*,#22002,.T.);
#31304=ORIENTED_EDGE('',*,*,#22004,.T.);
#31305=ORIENTED_EDGE('',*,*,#22005,.F.);
#31306=ORIENTED_EDGE('',*,*,#22006,.F.);
#31307=ORIENTED_EDGE('',*,*,#22004,.F.);
#31308=ORIENTED_EDGE('',*,*,#22001,.T.);
#31309=ORIENTED_EDGE('',*,*,#22007,.T.);
#31310=ORIENTED_EDGE('',*,*,#22008,.F.);
#31311=ORIENTED_EDGE('',*,*,#22007,.F.);
#31312=ORIENTED_EDGE('',*,*,#22000,.F.);
#31313=ORIENTED_EDGE('',*,*,#22009,.F.);
#31314=ORIENTED_EDGE('',*,*,#22010,.F.);
#31315=ORIENTED_EDGE('',*,*,#22011,.T.);
#31316=ORIENTED_EDGE('',*,*,#22012,.F.);
#31317=ORIENTED_EDGE('',*,*,#22013,.F.);
#31318=ORIENTED_EDGE('',*,*,#22014,.F.);
#31319=ORIENTED_EDGE('',*,*,#22013,.T.);
#31320=ORIENTED_EDGE('',*,*,#22015,.T.);
#31321=ORIENTED_EDGE('',*,*,#22016,.F.);
#31322=ORIENTED_EDGE('',*,*,#22015,.F.);
#31323=ORIENTED_EDGE('',*,*,#22012,.T.);
#31324=ORIENTED_EDGE('',*,*,#22017,.T.);
#31325=ORIENTED_EDGE('',*,*,#22018,.F.);
#31326=ORIENTED_EDGE('',*,*,#22017,.F.);
#31327=ORIENTED_EDGE('',*,*,#22011,.F.);
#31328=ORIENTED_EDGE('',*,*,#22019,.F.);
#31329=ORIENTED_EDGE('',*,*,#22020,.T.);
#31330=ORIENTED_EDGE('',*,*,#22021,.F.);
#31331=ORIENTED_EDGE('',*,*,#22022,.F.);
#31332=ORIENTED_EDGE('',*,*,#22023,.F.);
#31333=ORIENTED_EDGE('',*,*,#22022,.T.);
#31334=ORIENTED_EDGE('',*,*,#22024,.T.);
#31335=ORIENTED_EDGE('',*,*,#22025,.F.);
#31336=ORIENTED_EDGE('',*,*,#22024,.F.);
#31337=ORIENTED_EDGE('',*,*,#22021,.T.);
#31338=ORIENTED_EDGE('',*,*,#22026,.T.);
#31339=ORIENTED_EDGE('',*,*,#22027,.F.);
#31340=ORIENTED_EDGE('',*,*,#22026,.F.);
#31341=ORIENTED_EDGE('',*,*,#22020,.F.);
#31342=ORIENTED_EDGE('',*,*,#22028,.F.);
#31343=ORIENTED_EDGE('',*,*,#22029,.T.);
#31344=ORIENTED_EDGE('',*,*,#22030,.F.);
#31345=ORIENTED_EDGE('',*,*,#22031,.F.);
#31346=ORIENTED_EDGE('',*,*,#22032,.F.);
#31347=ORIENTED_EDGE('',*,*,#22031,.T.);
#31348=ORIENTED_EDGE('',*,*,#22033,.T.);
#31349=ORIENTED_EDGE('',*,*,#22034,.F.);
#31350=ORIENTED_EDGE('',*,*,#22033,.F.);
#31351=ORIENTED_EDGE('',*,*,#22030,.T.);
#31352=ORIENTED_EDGE('',*,*,#22035,.T.);
#31353=ORIENTED_EDGE('',*,*,#22036,.F.);
#31354=ORIENTED_EDGE('',*,*,#22035,.F.);
#31355=ORIENTED_EDGE('',*,*,#22029,.F.);
#31356=ORIENTED_EDGE('',*,*,#22037,.F.);
#31357=ORIENTED_EDGE('',*,*,#22038,.T.);
#31358=ORIENTED_EDGE('',*,*,#22039,.F.);
#31359=ORIENTED_EDGE('',*,*,#22040,.F.);
#31360=ORIENTED_EDGE('',*,*,#22041,.F.);
#31361=ORIENTED_EDGE('',*,*,#22040,.T.);
#31362=ORIENTED_EDGE('',*,*,#22042,.T.);
#31363=ORIENTED_EDGE('',*,*,#22043,.F.);
#31364=ORIENTED_EDGE('',*,*,#22042,.F.);
#31365=ORIENTED_EDGE('',*,*,#22039,.T.);
#31366=ORIENTED_EDGE('',*,*,#22044,.T.);
#31367=ORIENTED_EDGE('',*,*,#22045,.F.);
#31368=ORIENTED_EDGE('',*,*,#22044,.F.);
#31369=ORIENTED_EDGE('',*,*,#22038,.F.);
#31370=ORIENTED_EDGE('',*,*,#22046,.F.);
#31371=ORIENTED_EDGE('',*,*,#22047,.T.);
#31372=ORIENTED_EDGE('',*,*,#22048,.F.);
#31373=ORIENTED_EDGE('',*,*,#22049,.F.);
#31374=ORIENTED_EDGE('',*,*,#22050,.F.);
#31375=ORIENTED_EDGE('',*,*,#22049,.T.);
#31376=ORIENTED_EDGE('',*,*,#22051,.T.);
#31377=ORIENTED_EDGE('',*,*,#22052,.F.);
#31378=ORIENTED_EDGE('',*,*,#22051,.F.);
#31379=ORIENTED_EDGE('',*,*,#22048,.T.);
#31380=ORIENTED_EDGE('',*,*,#22053,.T.);
#31381=ORIENTED_EDGE('',*,*,#22054,.F.);
#31382=ORIENTED_EDGE('',*,*,#22053,.F.);
#31383=ORIENTED_EDGE('',*,*,#22047,.F.);
#31384=ORIENTED_EDGE('',*,*,#22055,.F.);
#31385=ORIENTED_EDGE('',*,*,#22056,.T.);
#31386=ORIENTED_EDGE('',*,*,#22057,.F.);
#31387=ORIENTED_EDGE('',*,*,#22058,.F.);
#31388=ORIENTED_EDGE('',*,*,#22059,.F.);
#31389=ORIENTED_EDGE('',*,*,#22058,.T.);
#31390=ORIENTED_EDGE('',*,*,#22060,.T.);
#31391=ORIENTED_EDGE('',*,*,#22061,.F.);
#31392=ORIENTED_EDGE('',*,*,#22060,.F.);
#31393=ORIENTED_EDGE('',*,*,#22057,.T.);
#31394=ORIENTED_EDGE('',*,*,#22062,.T.);
#31395=ORIENTED_EDGE('',*,*,#22063,.F.);
#31396=ORIENTED_EDGE('',*,*,#22062,.F.);
#31397=ORIENTED_EDGE('',*,*,#22056,.F.);
#31398=ORIENTED_EDGE('',*,*,#22064,.F.);
#31399=ORIENTED_EDGE('',*,*,#22065,.T.);
#31400=ORIENTED_EDGE('',*,*,#22066,.F.);
#31401=ORIENTED_EDGE('',*,*,#22067,.F.);
#31402=ORIENTED_EDGE('',*,*,#22068,.F.);
#31403=ORIENTED_EDGE('',*,*,#22067,.T.);
#31404=ORIENTED_EDGE('',*,*,#22069,.T.);
#31405=ORIENTED_EDGE('',*,*,#22070,.F.);
#31406=ORIENTED_EDGE('',*,*,#22069,.F.);
#31407=ORIENTED_EDGE('',*,*,#22066,.T.);
#31408=ORIENTED_EDGE('',*,*,#22071,.T.);
#31409=ORIENTED_EDGE('',*,*,#22072,.F.);
#31410=ORIENTED_EDGE('',*,*,#22071,.F.);
#31411=ORIENTED_EDGE('',*,*,#22065,.F.);
#31412=ORIENTED_EDGE('',*,*,#22073,.F.);
#31413=ORIENTED_EDGE('',*,*,#22074,.T.);
#31414=ORIENTED_EDGE('',*,*,#22075,.F.);
#31415=ORIENTED_EDGE('',*,*,#22076,.F.);
#31416=ORIENTED_EDGE('',*,*,#22077,.F.);
#31417=ORIENTED_EDGE('',*,*,#22076,.T.);
#31418=ORIENTED_EDGE('',*,*,#22078,.T.);
#31419=ORIENTED_EDGE('',*,*,#22079,.F.);
#31420=ORIENTED_EDGE('',*,*,#22078,.F.);
#31421=ORIENTED_EDGE('',*,*,#22075,.T.);
#31422=ORIENTED_EDGE('',*,*,#22080,.T.);
#31423=ORIENTED_EDGE('',*,*,#22081,.F.);
#31424=ORIENTED_EDGE('',*,*,#22080,.F.);
#31425=ORIENTED_EDGE('',*,*,#22074,.F.);
#31426=ORIENTED_EDGE('',*,*,#22082,.F.);
#31427=ORIENTED_EDGE('',*,*,#22083,.T.);
#31428=ORIENTED_EDGE('',*,*,#22084,.F.);
#31429=ORIENTED_EDGE('',*,*,#22085,.F.);
#31430=ORIENTED_EDGE('',*,*,#22086,.F.);
#31431=ORIENTED_EDGE('',*,*,#22085,.T.);
#31432=ORIENTED_EDGE('',*,*,#22087,.T.);
#31433=ORIENTED_EDGE('',*,*,#22088,.F.);
#31434=ORIENTED_EDGE('',*,*,#22087,.F.);
#31435=ORIENTED_EDGE('',*,*,#22084,.T.);
#31436=ORIENTED_EDGE('',*,*,#22089,.T.);
#31437=ORIENTED_EDGE('',*,*,#22090,.F.);
#31438=ORIENTED_EDGE('',*,*,#22089,.F.);
#31439=ORIENTED_EDGE('',*,*,#22083,.F.);
#31440=ORIENTED_EDGE('',*,*,#22091,.F.);
#31441=ORIENTED_EDGE('',*,*,#22092,.T.);
#31442=ORIENTED_EDGE('',*,*,#22093,.F.);
#31443=ORIENTED_EDGE('',*,*,#22094,.F.);
#31444=ORIENTED_EDGE('',*,*,#22095,.F.);
#31445=ORIENTED_EDGE('',*,*,#22094,.T.);
#31446=ORIENTED_EDGE('',*,*,#22096,.T.);
#31447=ORIENTED_EDGE('',*,*,#22097,.F.);
#31448=ORIENTED_EDGE('',*,*,#22096,.F.);
#31449=ORIENTED_EDGE('',*,*,#22093,.T.);
#31450=ORIENTED_EDGE('',*,*,#22098,.T.);
#31451=ORIENTED_EDGE('',*,*,#22099,.F.);
#31452=ORIENTED_EDGE('',*,*,#22098,.F.);
#31453=ORIENTED_EDGE('',*,*,#22092,.F.);
#31454=ORIENTED_EDGE('',*,*,#22100,.F.);
#31455=ORIENTED_EDGE('',*,*,#22101,.T.);
#31456=ORIENTED_EDGE('',*,*,#22102,.F.);
#31457=ORIENTED_EDGE('',*,*,#22103,.F.);
#31458=ORIENTED_EDGE('',*,*,#22104,.F.);
#31459=ORIENTED_EDGE('',*,*,#22103,.T.);
#31460=ORIENTED_EDGE('',*,*,#22105,.T.);
#31461=ORIENTED_EDGE('',*,*,#22106,.F.);
#31462=ORIENTED_EDGE('',*,*,#22105,.F.);
#31463=ORIENTED_EDGE('',*,*,#22102,.T.);
#31464=ORIENTED_EDGE('',*,*,#22107,.T.);
#31465=ORIENTED_EDGE('',*,*,#22108,.F.);
#31466=ORIENTED_EDGE('',*,*,#22107,.F.);
#31467=ORIENTED_EDGE('',*,*,#22101,.F.);
#31468=ORIENTED_EDGE('',*,*,#22109,.F.);
#31469=ORIENTED_EDGE('',*,*,#22110,.T.);
#31470=ORIENTED_EDGE('',*,*,#22111,.F.);
#31471=ORIENTED_EDGE('',*,*,#22112,.F.);
#31472=ORIENTED_EDGE('',*,*,#22113,.F.);
#31473=ORIENTED_EDGE('',*,*,#22112,.T.);
#31474=ORIENTED_EDGE('',*,*,#22114,.T.);
#31475=ORIENTED_EDGE('',*,*,#22115,.F.);
#31476=ORIENTED_EDGE('',*,*,#22114,.F.);
#31477=ORIENTED_EDGE('',*,*,#22111,.T.);
#31478=ORIENTED_EDGE('',*,*,#22116,.T.);
#31479=ORIENTED_EDGE('',*,*,#22117,.F.);
#31480=ORIENTED_EDGE('',*,*,#22116,.F.);
#31481=ORIENTED_EDGE('',*,*,#22110,.F.);
#31482=ORIENTED_EDGE('',*,*,#22118,.F.);
#31483=ORIENTED_EDGE('',*,*,#22119,.T.);
#31484=ORIENTED_EDGE('',*,*,#22120,.F.);
#31485=ORIENTED_EDGE('',*,*,#22121,.F.);
#31486=ORIENTED_EDGE('',*,*,#22122,.F.);
#31487=ORIENTED_EDGE('',*,*,#22121,.T.);
#31488=ORIENTED_EDGE('',*,*,#22123,.T.);
#31489=ORIENTED_EDGE('',*,*,#22124,.F.);
#31490=ORIENTED_EDGE('',*,*,#22123,.F.);
#31491=ORIENTED_EDGE('',*,*,#22120,.T.);
#31492=ORIENTED_EDGE('',*,*,#22125,.T.);
#31493=ORIENTED_EDGE('',*,*,#22126,.F.);
#31494=ORIENTED_EDGE('',*,*,#22125,.F.);
#31495=ORIENTED_EDGE('',*,*,#22119,.F.);
#31496=ORIENTED_EDGE('',*,*,#22127,.F.);
#31497=ORIENTED_EDGE('',*,*,#22128,.T.);
#31498=ORIENTED_EDGE('',*,*,#22129,.F.);
#31499=ORIENTED_EDGE('',*,*,#22130,.F.);
#31500=ORIENTED_EDGE('',*,*,#22131,.F.);
#31501=ORIENTED_EDGE('',*,*,#22130,.T.);
#31502=ORIENTED_EDGE('',*,*,#22132,.T.);
#31503=ORIENTED_EDGE('',*,*,#22133,.F.);
#31504=ORIENTED_EDGE('',*,*,#22132,.F.);
#31505=ORIENTED_EDGE('',*,*,#22129,.T.);
#31506=ORIENTED_EDGE('',*,*,#22134,.T.);
#31507=ORIENTED_EDGE('',*,*,#22135,.F.);
#31508=ORIENTED_EDGE('',*,*,#22134,.F.);
#31509=ORIENTED_EDGE('',*,*,#22128,.F.);
#31510=ORIENTED_EDGE('',*,*,#22136,.F.);
#31511=ORIENTED_EDGE('',*,*,#22137,.T.);
#31512=ORIENTED_EDGE('',*,*,#22138,.F.);
#31513=ORIENTED_EDGE('',*,*,#22139,.F.);
#31514=ORIENTED_EDGE('',*,*,#22140,.F.);
#31515=ORIENTED_EDGE('',*,*,#22139,.T.);
#31516=ORIENTED_EDGE('',*,*,#22141,.T.);
#31517=ORIENTED_EDGE('',*,*,#22142,.F.);
#31518=ORIENTED_EDGE('',*,*,#22141,.F.);
#31519=ORIENTED_EDGE('',*,*,#22138,.T.);
#31520=ORIENTED_EDGE('',*,*,#22143,.T.);
#31521=ORIENTED_EDGE('',*,*,#22144,.F.);
#31522=ORIENTED_EDGE('',*,*,#22143,.F.);
#31523=ORIENTED_EDGE('',*,*,#22137,.F.);
#31524=ORIENTED_EDGE('',*,*,#22145,.F.);
#31525=ORIENTED_EDGE('',*,*,#22146,.T.);
#31526=ORIENTED_EDGE('',*,*,#22147,.F.);
#31527=ORIENTED_EDGE('',*,*,#22148,.F.);
#31528=ORIENTED_EDGE('',*,*,#22149,.F.);
#31529=ORIENTED_EDGE('',*,*,#22148,.T.);
#31530=ORIENTED_EDGE('',*,*,#22150,.T.);
#31531=ORIENTED_EDGE('',*,*,#22151,.F.);
#31532=ORIENTED_EDGE('',*,*,#22150,.F.);
#31533=ORIENTED_EDGE('',*,*,#22147,.T.);
#31534=ORIENTED_EDGE('',*,*,#22152,.T.);
#31535=ORIENTED_EDGE('',*,*,#22153,.F.);
#31536=ORIENTED_EDGE('',*,*,#22152,.F.);
#31537=ORIENTED_EDGE('',*,*,#22146,.F.);
#31538=ORIENTED_EDGE('',*,*,#22154,.F.);
#31539=ORIENTED_EDGE('',*,*,#22155,.T.);
#31540=ORIENTED_EDGE('',*,*,#22156,.F.);
#31541=ORIENTED_EDGE('',*,*,#22157,.F.);
#31542=ORIENTED_EDGE('',*,*,#22158,.F.);
#31543=ORIENTED_EDGE('',*,*,#22157,.T.);
#31544=ORIENTED_EDGE('',*,*,#22159,.T.);
#31545=ORIENTED_EDGE('',*,*,#22160,.F.);
#31546=ORIENTED_EDGE('',*,*,#22159,.F.);
#31547=ORIENTED_EDGE('',*,*,#22156,.T.);
#31548=ORIENTED_EDGE('',*,*,#22161,.T.);
#31549=ORIENTED_EDGE('',*,*,#22162,.F.);
#31550=ORIENTED_EDGE('',*,*,#22161,.F.);
#31551=ORIENTED_EDGE('',*,*,#22155,.F.);
#31552=ORIENTED_EDGE('',*,*,#22163,.F.);
#31553=ORIENTED_EDGE('',*,*,#22164,.T.);
#31554=ORIENTED_EDGE('',*,*,#22165,.F.);
#31555=ORIENTED_EDGE('',*,*,#22166,.F.);
#31556=ORIENTED_EDGE('',*,*,#22167,.F.);
#31557=ORIENTED_EDGE('',*,*,#22166,.T.);
#31558=ORIENTED_EDGE('',*,*,#22168,.T.);
#31559=ORIENTED_EDGE('',*,*,#22169,.F.);
#31560=ORIENTED_EDGE('',*,*,#22168,.F.);
#31561=ORIENTED_EDGE('',*,*,#22165,.T.);
#31562=ORIENTED_EDGE('',*,*,#22170,.T.);
#31563=ORIENTED_EDGE('',*,*,#22171,.F.);
#31564=ORIENTED_EDGE('',*,*,#22170,.F.);
#31565=ORIENTED_EDGE('',*,*,#22164,.F.);
#31566=ORIENTED_EDGE('',*,*,#22172,.F.);
#31567=ORIENTED_EDGE('',*,*,#22173,.T.);
#31568=ORIENTED_EDGE('',*,*,#22009,.T.);
#31569=ORIENTED_EDGE('',*,*,#21999,.T.);
#31570=ORIENTED_EDGE('',*,*,#22003,.T.);
#31571=ORIENTED_EDGE('',*,*,#22174,.T.);
#31572=ORIENTED_EDGE('',*,*,#21817,.T.);
#31573=ORIENTED_EDGE('',*,*,#22174,.F.);
#31574=ORIENTED_EDGE('',*,*,#22005,.T.);
#31575=ORIENTED_EDGE('',*,*,#22006,.T.);
#31576=ORIENTED_EDGE('',*,*,#22008,.T.);
#31577=ORIENTED_EDGE('',*,*,#22173,.F.);
#31578=ORIENTED_EDGE('',*,*,#21852,.T.);
#31579=ORIENTED_EDGE('',*,*,#21854,.T.);
#31580=ORIENTED_EDGE('',*,*,#21846,.T.);
#31581=ORIENTED_EDGE('',*,*,#21850,.T.);
#31582=ORIENTED_EDGE('',*,*,#21861,.T.);
#31583=ORIENTED_EDGE('',*,*,#21863,.T.);
#31584=ORIENTED_EDGE('',*,*,#21855,.T.);
#31585=ORIENTED_EDGE('',*,*,#21859,.T.);
#31586=ORIENTED_EDGE('',*,*,#21870,.T.);
#31587=ORIENTED_EDGE('',*,*,#21872,.T.);
#31588=ORIENTED_EDGE('',*,*,#21864,.T.);
#31589=ORIENTED_EDGE('',*,*,#21868,.T.);
#31590=ORIENTED_EDGE('',*,*,#21879,.T.);
#31591=ORIENTED_EDGE('',*,*,#21881,.T.);
#31592=ORIENTED_EDGE('',*,*,#21873,.T.);
#31593=ORIENTED_EDGE('',*,*,#21877,.T.);
#31594=ORIENTED_EDGE('',*,*,#21888,.T.);
#31595=ORIENTED_EDGE('',*,*,#21890,.T.);
#31596=ORIENTED_EDGE('',*,*,#21882,.T.);
#31597=ORIENTED_EDGE('',*,*,#21886,.T.);
#31598=ORIENTED_EDGE('',*,*,#21897,.T.);
#31599=ORIENTED_EDGE('',*,*,#21899,.T.);
#31600=ORIENTED_EDGE('',*,*,#21891,.T.);
#31601=ORIENTED_EDGE('',*,*,#21895,.T.);
#31602=ORIENTED_EDGE('',*,*,#21906,.T.);
#31603=ORIENTED_EDGE('',*,*,#21908,.T.);
#31604=ORIENTED_EDGE('',*,*,#21900,.T.);
#31605=ORIENTED_EDGE('',*,*,#21904,.T.);
#31606=ORIENTED_EDGE('',*,*,#21915,.T.);
#31607=ORIENTED_EDGE('',*,*,#21917,.T.);
#31608=ORIENTED_EDGE('',*,*,#21909,.T.);
#31609=ORIENTED_EDGE('',*,*,#21913,.T.);
#31610=ORIENTED_EDGE('',*,*,#21924,.T.);
#31611=ORIENTED_EDGE('',*,*,#21926,.T.);
#31612=ORIENTED_EDGE('',*,*,#21918,.T.);
#31613=ORIENTED_EDGE('',*,*,#21922,.T.);
#31614=ORIENTED_EDGE('',*,*,#21933,.T.);
#31615=ORIENTED_EDGE('',*,*,#21935,.T.);
#31616=ORIENTED_EDGE('',*,*,#21927,.T.);
#31617=ORIENTED_EDGE('',*,*,#21931,.T.);
#31618=ORIENTED_EDGE('',*,*,#21942,.T.);
#31619=ORIENTED_EDGE('',*,*,#21944,.T.);
#31620=ORIENTED_EDGE('',*,*,#21936,.T.);
#31621=ORIENTED_EDGE('',*,*,#21940,.T.);
#31622=ORIENTED_EDGE('',*,*,#21951,.T.);
#31623=ORIENTED_EDGE('',*,*,#21953,.T.);
#31624=ORIENTED_EDGE('',*,*,#21945,.T.);
#31625=ORIENTED_EDGE('',*,*,#21949,.T.);
#31626=ORIENTED_EDGE('',*,*,#21960,.T.);
#31627=ORIENTED_EDGE('',*,*,#21962,.T.);
#31628=ORIENTED_EDGE('',*,*,#21954,.T.);
#31629=ORIENTED_EDGE('',*,*,#21958,.T.);
#31630=ORIENTED_EDGE('',*,*,#21969,.T.);
#31631=ORIENTED_EDGE('',*,*,#21971,.T.);
#31632=ORIENTED_EDGE('',*,*,#21963,.T.);
#31633=ORIENTED_EDGE('',*,*,#21967,.T.);
#31634=ORIENTED_EDGE('',*,*,#21978,.T.);
#31635=ORIENTED_EDGE('',*,*,#21980,.T.);
#31636=ORIENTED_EDGE('',*,*,#21972,.T.);
#31637=ORIENTED_EDGE('',*,*,#21976,.T.);
#31638=ORIENTED_EDGE('',*,*,#21987,.T.);
#31639=ORIENTED_EDGE('',*,*,#21989,.T.);
#31640=ORIENTED_EDGE('',*,*,#21981,.T.);
#31641=ORIENTED_EDGE('',*,*,#21985,.T.);
#31642=ORIENTED_EDGE('',*,*,#21996,.T.);
#31643=ORIENTED_EDGE('',*,*,#21998,.T.);
#31644=ORIENTED_EDGE('',*,*,#21990,.T.);
#31645=ORIENTED_EDGE('',*,*,#21994,.T.);
#31646=ORIENTED_EDGE('',*,*,#22016,.T.);
#31647=ORIENTED_EDGE('',*,*,#22018,.T.);
#31648=ORIENTED_EDGE('',*,*,#22010,.T.);
#31649=ORIENTED_EDGE('',*,*,#22014,.T.);
#31650=ORIENTED_EDGE('',*,*,#22025,.T.);
#31651=ORIENTED_EDGE('',*,*,#22027,.T.);
#31652=ORIENTED_EDGE('',*,*,#22019,.T.);
#31653=ORIENTED_EDGE('',*,*,#22023,.T.);
#31654=ORIENTED_EDGE('',*,*,#22034,.T.);
#31655=ORIENTED_EDGE('',*,*,#22036,.T.);
#31656=ORIENTED_EDGE('',*,*,#22028,.T.);
#31657=ORIENTED_EDGE('',*,*,#22032,.T.);
#31658=ORIENTED_EDGE('',*,*,#22043,.T.);
#31659=ORIENTED_EDGE('',*,*,#22045,.T.);
#31660=ORIENTED_EDGE('',*,*,#22037,.T.);
#31661=ORIENTED_EDGE('',*,*,#22041,.T.);
#31662=ORIENTED_EDGE('',*,*,#22052,.T.);
#31663=ORIENTED_EDGE('',*,*,#22054,.T.);
#31664=ORIENTED_EDGE('',*,*,#22046,.T.);
#31665=ORIENTED_EDGE('',*,*,#22050,.T.);
#31666=ORIENTED_EDGE('',*,*,#22061,.T.);
#31667=ORIENTED_EDGE('',*,*,#22063,.T.);
#31668=ORIENTED_EDGE('',*,*,#22055,.T.);
#31669=ORIENTED_EDGE('',*,*,#22059,.T.);
#31670=ORIENTED_EDGE('',*,*,#22070,.T.);
#31671=ORIENTED_EDGE('',*,*,#22072,.T.);
#31672=ORIENTED_EDGE('',*,*,#22064,.T.);
#31673=ORIENTED_EDGE('',*,*,#22068,.T.);
#31674=ORIENTED_EDGE('',*,*,#22079,.T.);
#31675=ORIENTED_EDGE('',*,*,#22081,.T.);
#31676=ORIENTED_EDGE('',*,*,#22073,.T.);
#31677=ORIENTED_EDGE('',*,*,#22077,.T.);
#31678=ORIENTED_EDGE('',*,*,#22088,.T.);
#31679=ORIENTED_EDGE('',*,*,#22090,.T.);
#31680=ORIENTED_EDGE('',*,*,#22082,.T.);
#31681=ORIENTED_EDGE('',*,*,#22086,.T.);
#31682=ORIENTED_EDGE('',*,*,#22097,.T.);
#31683=ORIENTED_EDGE('',*,*,#22099,.T.);
#31684=ORIENTED_EDGE('',*,*,#22091,.T.);
#31685=ORIENTED_EDGE('',*,*,#22095,.T.);
#31686=ORIENTED_EDGE('',*,*,#22106,.T.);
#31687=ORIENTED_EDGE('',*,*,#22108,.T.);
#31688=ORIENTED_EDGE('',*,*,#22100,.T.);
#31689=ORIENTED_EDGE('',*,*,#22104,.T.);
#31690=ORIENTED_EDGE('',*,*,#22115,.T.);
#31691=ORIENTED_EDGE('',*,*,#22117,.T.);
#31692=ORIENTED_EDGE('',*,*,#22109,.T.);
#31693=ORIENTED_EDGE('',*,*,#22113,.T.);
#31694=ORIENTED_EDGE('',*,*,#22124,.T.);
#31695=ORIENTED_EDGE('',*,*,#22126,.T.);
#31696=ORIENTED_EDGE('',*,*,#22118,.T.);
#31697=ORIENTED_EDGE('',*,*,#22122,.T.);
#31698=ORIENTED_EDGE('',*,*,#22133,.T.);
#31699=ORIENTED_EDGE('',*,*,#22135,.T.);
#31700=ORIENTED_EDGE('',*,*,#22127,.T.);
#31701=ORIENTED_EDGE('',*,*,#22131,.T.);
#31702=ORIENTED_EDGE('',*,*,#22142,.T.);
#31703=ORIENTED_EDGE('',*,*,#22144,.T.);
#31704=ORIENTED_EDGE('',*,*,#22136,.T.);
#31705=ORIENTED_EDGE('',*,*,#22140,.T.);
#31706=ORIENTED_EDGE('',*,*,#22151,.T.);
#31707=ORIENTED_EDGE('',*,*,#22153,.T.);
#31708=ORIENTED_EDGE('',*,*,#22145,.T.);
#31709=ORIENTED_EDGE('',*,*,#22149,.T.);
#31710=ORIENTED_EDGE('',*,*,#22160,.T.);
#31711=ORIENTED_EDGE('',*,*,#22162,.T.);
#31712=ORIENTED_EDGE('',*,*,#22154,.T.);
#31713=ORIENTED_EDGE('',*,*,#22158,.T.);
#31714=ORIENTED_EDGE('',*,*,#22169,.T.);
#31715=ORIENTED_EDGE('',*,*,#22171,.T.);
#31716=ORIENTED_EDGE('',*,*,#22163,.T.);
#31717=ORIENTED_EDGE('',*,*,#22167,.T.);
#31718=ORIENTED_EDGE('',*,*,#21840,.F.);
#31719=ORIENTED_EDGE('',*,*,#21628,.F.);
#31720=ORIENTED_EDGE('',*,*,#21841,.F.);
#31721=ORIENTED_EDGE('',*,*,#22175,.T.);
#31722=ORIENTED_EDGE('',*,*,#22172,.T.);
#31723=ORIENTED_EDGE('',*,*,#22175,.F.);
#31724=ORIENTED_EDGE('',*,*,#22176,.T.);
#31725=ORIENTED_EDGE('',*,*,#22177,.T.);
#31726=ORIENTED_EDGE('',*,*,#22178,.T.);
#31727=ORIENTED_EDGE('',*,*,#22179,.T.);
#31728=ORIENTED_EDGE('',*,*,#22180,.T.);
#31729=ORIENTED_EDGE('',*,*,#22181,.T.);
#31730=ORIENTED_EDGE('',*,*,#22182,.T.);
#31731=ORIENTED_EDGE('',*,*,#22183,.T.);
#31732=ORIENTED_EDGE('',*,*,#22184,.T.);
#31733=ORIENTED_EDGE('',*,*,#22185,.T.);
#31734=ORIENTED_EDGE('',*,*,#22186,.T.);
#31735=ORIENTED_EDGE('',*,*,#22187,.T.);
#31736=ORIENTED_EDGE('',*,*,#22188,.T.);
#31737=ORIENTED_EDGE('',*,*,#22189,.T.);
#31738=ORIENTED_EDGE('',*,*,#22190,.T.);
#31739=ORIENTED_EDGE('',*,*,#22177,.F.);
#31740=ORIENTED_EDGE('',*,*,#22180,.F.);
#31741=ORIENTED_EDGE('',*,*,#22191,.T.);
#31742=ORIENTED_EDGE('',*,*,#22192,.T.);
#31743=ORIENTED_EDGE('',*,*,#22193,.T.);
#31744=ORIENTED_EDGE('',*,*,#22194,.T.);
#31745=ORIENTED_EDGE('',*,*,#22195,.T.);
#31746=ORIENTED_EDGE('',*,*,#22190,.F.);
#31747=ORIENTED_EDGE('',*,*,#22196,.T.);
#31748=ORIENTED_EDGE('',*,*,#22197,.T.);
#31749=ORIENTED_EDGE('',*,*,#22198,.T.);
#31750=ORIENTED_EDGE('',*,*,#22199,.T.);
#31751=ORIENTED_EDGE('',*,*,#22200,.T.);
#31752=ORIENTED_EDGE('',*,*,#22178,.F.);
#31753=ORIENTED_EDGE('',*,*,#22179,.F.);
#31754=ORIENTED_EDGE('',*,*,#22200,.F.);
#31755=ORIENTED_EDGE('',*,*,#22191,.F.);
#31756=ORIENTED_EDGE('',*,*,#22189,.F.);
#31757=ORIENTED_EDGE('',*,*,#22201,.F.);
#31758=ORIENTED_EDGE('',*,*,#22196,.F.);
#31759=ORIENTED_EDGE('',*,*,#22187,.F.);
#31760=ORIENTED_EDGE('',*,*,#22202,.F.);
#31761=ORIENTED_EDGE('',*,*,#22203,.F.);
#31762=ORIENTED_EDGE('',*,*,#22185,.F.);
#31763=ORIENTED_EDGE('',*,*,#22204,.F.);
#31764=ORIENTED_EDGE('',*,*,#22205,.F.);
#31765=ORIENTED_EDGE('',*,*,#22183,.F.);
#31766=ORIENTED_EDGE('',*,*,#22206,.F.);
#31767=ORIENTED_EDGE('',*,*,#22207,.F.);
#31768=ORIENTED_EDGE('',*,*,#22181,.F.);
#31769=ORIENTED_EDGE('',*,*,#22195,.F.);
#31770=ORIENTED_EDGE('',*,*,#22208,.F.);
#31771=ORIENTED_EDGE('',*,*,#22188,.F.);
#31772=ORIENTED_EDGE('',*,*,#22203,.T.);
#31773=ORIENTED_EDGE('',*,*,#22209,.T.);
#31774=ORIENTED_EDGE('',*,*,#22210,.T.);
#31775=ORIENTED_EDGE('',*,*,#22211,.T.);
#31776=ORIENTED_EDGE('',*,*,#22201,.T.);
#31777=ORIENTED_EDGE('',*,*,#22176,.F.);
#31778=ORIENTED_EDGE('',*,*,#22212,.T.);
#31779=ORIENTED_EDGE('',*,*,#22213,.F.);
#31780=ORIENTED_EDGE('',*,*,#22214,.F.);
#31781=ORIENTED_EDGE('',*,*,#22215,.F.);
#31782=ORIENTED_EDGE('',*,*,#22216,.F.);
#31783=ORIENTED_EDGE('',*,*,#22217,.F.);
#31784=ORIENTED_EDGE('',*,*,#22218,.F.);
#31785=ORIENTED_EDGE('',*,*,#22219,.F.);
#31786=ORIENTED_EDGE('',*,*,#22220,.F.);
#31787=ORIENTED_EDGE('',*,*,#22221,.F.);
#31788=ORIENTED_EDGE('',*,*,#22220,.T.);
#31789=ORIENTED_EDGE('',*,*,#22222,.T.);
#31790=ORIENTED_EDGE('',*,*,#22215,.T.);
#31791=ORIENTED_EDGE('',*,*,#22223,.T.);
#31792=ORIENTED_EDGE('',*,*,#22224,.F.);
#31793=ORIENTED_EDGE('',*,*,#22197,.F.);
#31794=ORIENTED_EDGE('',*,*,#22211,.F.);
#31795=ORIENTED_EDGE('',*,*,#22225,.F.);
#31796=ORIENTED_EDGE('',*,*,#22226,.F.);
#31797=ORIENTED_EDGE('',*,*,#22227,.F.);
#31798=ORIENTED_EDGE('',*,*,#22209,.F.);
#31799=ORIENTED_EDGE('',*,*,#22228,.F.);
#31800=ORIENTED_EDGE('',*,*,#22229,.F.);
#31801=ORIENTED_EDGE('',*,*,#22230,.F.);
#31802=ORIENTED_EDGE('',*,*,#22231,.F.);
#31803=ORIENTED_EDGE('',*,*,#22232,.F.);
#31804=ORIENTED_EDGE('',*,*,#22231,.T.);
#31805=ORIENTED_EDGE('',*,*,#22233,.T.);
#31806=ORIENTED_EDGE('',*,*,#22221,.T.);
#31807=ORIENTED_EDGE('',*,*,#22234,.T.);
#31808=ORIENTED_EDGE('',*,*,#22235,.F.);
#31809=ORIENTED_EDGE('',*,*,#22192,.F.);
#31810=ORIENTED_EDGE('',*,*,#22199,.F.);
#31811=ORIENTED_EDGE('',*,*,#22236,.F.);
#31812=ORIENTED_EDGE('',*,*,#22237,.F.);
#31813=ORIENTED_EDGE('',*,*,#22238,.F.);
#31814=ORIENTED_EDGE('',*,*,#22226,.T.);
#31815=ORIENTED_EDGE('',*,*,#22239,.T.);
#31816=ORIENTED_EDGE('',*,*,#22237,.T.);
#31817=ORIENTED_EDGE('',*,*,#22240,.T.);
#31818=ORIENTED_EDGE('',*,*,#22241,.F.);
#31819=ORIENTED_EDGE('',*,*,#22242,.F.);
#31820=ORIENTED_EDGE('',*,*,#22243,.F.);
#31821=ORIENTED_EDGE('',*,*,#22244,.F.);
#31822=ORIENTED_EDGE('',*,*,#22245,.F.);
#31823=ORIENTED_EDGE('',*,*,#22194,.F.);
#31824=ORIENTED_EDGE('',*,*,#22246,.F.);
#31825=ORIENTED_EDGE('',*,*,#22247,.F.);
#31826=ORIENTED_EDGE('',*,*,#22248,.F.);
#31827=ORIENTED_EDGE('',*,*,#22182,.F.);
#31828=ORIENTED_EDGE('',*,*,#22208,.T.);
#31829=ORIENTED_EDGE('',*,*,#22245,.T.);
#31830=ORIENTED_EDGE('',*,*,#22249,.T.);
#31831=ORIENTED_EDGE('',*,*,#22247,.T.);
#31832=ORIENTED_EDGE('',*,*,#22206,.T.);
#31833=ORIENTED_EDGE('',*,*,#22248,.T.);
#31834=ORIENTED_EDGE('',*,*,#22250,.T.);
#31835=ORIENTED_EDGE('',*,*,#22238,.T.);
#31836=ORIENTED_EDGE('',*,*,#22251,.T.);
#31837=ORIENTED_EDGE('',*,*,#22184,.F.);
#31838=ORIENTED_EDGE('',*,*,#22207,.T.);
#31839=ORIENTED_EDGE('',*,*,#22246,.T.);
#31840=ORIENTED_EDGE('',*,*,#22252,.T.);
#31841=ORIENTED_EDGE('',*,*,#22242,.T.);
#31842=ORIENTED_EDGE('',*,*,#22204,.T.);
#31843=ORIENTED_EDGE('',*,*,#22244,.T.);
#31844=ORIENTED_EDGE('',*,*,#22253,.T.);
#31845=ORIENTED_EDGE('',*,*,#22230,.T.);
#31846=ORIENTED_EDGE('',*,*,#22254,.T.);
#31847=ORIENTED_EDGE('',*,*,#22243,.T.);
#31848=ORIENTED_EDGE('',*,*,#22255,.T.);
#31849=ORIENTED_EDGE('',*,*,#22225,.T.);
#31850=ORIENTED_EDGE('',*,*,#22256,.T.);
#31851=ORIENTED_EDGE('',*,*,#22186,.F.);
#31852=ORIENTED_EDGE('',*,*,#22205,.T.);
#31853=ORIENTED_EDGE('',*,*,#22241,.T.);
#31854=ORIENTED_EDGE('',*,*,#22257,.T.);
#31855=ORIENTED_EDGE('',*,*,#22228,.T.);
#31856=ORIENTED_EDGE('',*,*,#22202,.T.);
#31857=ORIENTED_EDGE('',*,*,#22236,.T.);
#31858=ORIENTED_EDGE('',*,*,#22258,.T.);
#31859=ORIENTED_EDGE('',*,*,#22232,.T.);
#31860=ORIENTED_EDGE('',*,*,#22259,.T.);
#31861=ORIENTED_EDGE('',*,*,#22235,.T.);
#31862=ORIENTED_EDGE('',*,*,#22260,.T.);
#31863=ORIENTED_EDGE('',*,*,#22219,.T.);
#31864=ORIENTED_EDGE('',*,*,#22261,.T.);
#31865=ORIENTED_EDGE('',*,*,#22229,.T.);
#31866=ORIENTED_EDGE('',*,*,#22262,.T.);
#31867=ORIENTED_EDGE('',*,*,#22216,.T.);
#31868=ORIENTED_EDGE('',*,*,#22263,.T.);
#31869=ORIENTED_EDGE('',*,*,#22217,.T.);
#31870=ORIENTED_EDGE('',*,*,#22264,.T.);
#31871=ORIENTED_EDGE('',*,*,#22227,.T.);
#31872=ORIENTED_EDGE('',*,*,#22265,.T.);
#31873=ORIENTED_EDGE('',*,*,#22224,.T.);
#31874=ORIENTED_EDGE('',*,*,#22266,.T.);
#31875=ORIENTED_EDGE('',*,*,#22213,.T.);
#31876=ORIENTED_EDGE('',*,*,#22267,.T.);
#31877=ORIENTED_EDGE('',*,*,#22214,.T.);
#31878=ORIENTED_EDGE('',*,*,#22268,.T.);
#31879=ORIENTED_EDGE('',*,*,#22218,.T.);
#31880=ORIENTED_EDGE('',*,*,#22269,.T.);
#31881=ORIENTED_EDGE('',*,*,#22239,.F.);
#31882=ORIENTED_EDGE('',*,*,#22255,.F.);
#31883=ORIENTED_EDGE('',*,*,#22252,.F.);
#31884=ORIENTED_EDGE('',*,*,#22251,.F.);
#31885=ORIENTED_EDGE('',*,*,#22240,.F.);
#31886=ORIENTED_EDGE('',*,*,#22259,.F.);
#31887=ORIENTED_EDGE('',*,*,#22234,.F.);
#31888=ORIENTED_EDGE('',*,*,#22223,.F.);
#31889=ORIENTED_EDGE('',*,*,#22269,.F.);
#31890=ORIENTED_EDGE('',*,*,#22265,.F.);
#31891=ORIENTED_EDGE('',*,*,#22270,.T.);
#31892=ORIENTED_EDGE('',*,*,#22249,.F.);
#31893=ORIENTED_EDGE('',*,*,#22254,.F.);
#31894=ORIENTED_EDGE('',*,*,#22258,.F.);
#31895=ORIENTED_EDGE('',*,*,#22250,.F.);
#31896=ORIENTED_EDGE('',*,*,#22193,.F.);
#31897=ORIENTED_EDGE('',*,*,#22261,.F.);
#31898=ORIENTED_EDGE('',*,*,#22233,.F.);
#31899=ORIENTED_EDGE('',*,*,#22253,.F.);
#31900=ORIENTED_EDGE('',*,*,#22256,.F.);
#31901=ORIENTED_EDGE('',*,*,#22264,.F.);
#31902=ORIENTED_EDGE('',*,*,#22262,.F.);
#31903=ORIENTED_EDGE('',*,*,#22257,.F.);
#31904=ORIENTED_EDGE('',*,*,#22198,.F.);
#31905=ORIENTED_EDGE('',*,*,#22267,.F.);
#31906=ORIENTED_EDGE('',*,*,#22222,.F.);
#31907=ORIENTED_EDGE('',*,*,#22260,.F.);
#31908=ORIENTED_EDGE('',*,*,#22263,.F.);
#31909=ORIENTED_EDGE('',*,*,#22268,.F.);
#31910=ORIENTED_EDGE('',*,*,#22266,.F.);
#31911=ORIENTED_EDGE('',*,*,#22210,.F.);
#31912=ORIENTED_EDGE('',*,*,#22271,.F.);
#31913=ORIENTED_EDGE('',*,*,#22272,.T.);
#31914=ORIENTED_EDGE('',*,*,#22212,.F.);
#31915=ORIENTED_EDGE('',*,*,#22272,.F.);
#31916=ORIENTED_EDGE('',*,*,#22273,.F.);
#31917=ORIENTED_EDGE('',*,*,#22270,.F.);
#31918=ORIENTED_EDGE('',*,*,#22274,.T.);
#31919=ORIENTED_EDGE('',*,*,#22275,.T.);
#31920=ORIENTED_EDGE('',*,*,#22274,.F.);
#31921=ORIENTED_EDGE('',*,*,#22275,.F.);
#31922=ORIENTED_EDGE('',*,*,#22276,.T.);
#31923=ORIENTED_EDGE('',*,*,#22271,.T.);
#31924=ORIENTED_EDGE('',*,*,#22277,.T.);
#31925=ORIENTED_EDGE('',*,*,#22276,.F.);
#31926=ORIENTED_EDGE('',*,*,#22277,.F.);
#31927=ORIENTED_EDGE('',*,*,#22273,.T.);
#31928=CONICAL_SURFACE('',#34367,39.77639320225,0.553574358897046);
#31929=CONICAL_SURFACE('',#34372,38.5,1.10714871779409);
#31930=CONICAL_SURFACE('',#34377,36.97360679775,1.33897252229449);
#31931=CONICAL_SURFACE('',#34381,26.25,0.785398163397448);
#31932=CONICAL_SURFACE('',#34389,31.9267766952966,1.17809724509617);
#31933=CONICAL_SURFACE('',#34393,33.,0.78539816339745);
#31934=CONICAL_SURFACE('',#34398,33.8502380998955,0.44683437712894);
#31935=CONICAL_SURFACE('',#34401,35.25,0.108270590860456);
#31936=CONICAL_SURFACE('',#34403,126.961414092626,1.19422068631379);
#31937=CONICAL_SURFACE('',#34408,129.25,0.98279372324733);
#31938=CONICAL_SURFACE('',#34411,124.,1.40564764938027);
#31939=CONICAL_SURFACE('',#34413,131.441987426416,0.813147416020307);
#31940=CONICAL_SURFACE('',#34416,133.,0.643501108793283);
#31941=CONICAL_SURFACE('',#34419,134.437780860397,0.501135889531925);
#31942=CONICAL_SURFACE('',#34422,135.25,0.358770670270573);
#31943=CONICAL_SURFACE('',#34425,135.912219139603,0.17938533513529);
#31944=CONICAL_SURFACE('',#34864,51.75,0.785398163397448);
#31945=CONICAL_SURFACE('',#34867,14.75,0.785398163397448);
#31946=CONICAL_SURFACE('',#34870,51.75,0.785398163397457);
#31947=CONICAL_SURFACE('',#34873,14.75,0.785398163397448);
#31948=CONICAL_SURFACE('',#34876,51.75,0.785398163397457);
#31949=CONICAL_SURFACE('',#34879,14.75,0.785398163397448);
#31950=CONICAL_SURFACE('',#34882,51.75,0.785398163397448);
#31951=CONICAL_SURFACE('',#34885,14.75,0.785398163397453);
#31952=CONICAL_SURFACE('',#34888,51.75,0.785398163397448);
#31953=CONICAL_SURFACE('',#34891,14.75,0.785398163397453);
#31954=CONICAL_SURFACE('',#35920,127.185823536562,0.418990612504199);
#31955=CONICAL_SURFACE('',#35925,128.,0.837981225008393);
#31956=CONICAL_SURFACE('',#35960,138.753401519042,0.70282382469014);
#31957=CONICAL_SURFACE('',#35968,137.5,1.40564764938027);
#31958=CONICAL_SURFACE('',#35969,129.064176463438,1.20438877590164);
#31959=CONICAL_SURFACE('',#35973,138.823223304703,0.392699081698721);
#31960=CONICAL_SURFACE('',#35975,138.5,0.785398163397447);
#31961=CONICAL_SURFACE('',#35977,137.926776695297,1.17809724509618);
#31962=CONICAL_SURFACE('',#36132,25.,1.10714871779409);
#31963=CONICAL_SURFACE('',#36158,32.9,0.785398163397449);
#31964=CONICAL_SURFACE('',#36159,43.,0.785398163397448);
#31965=CONICAL_SURFACE('',#36163,124.75,1.05165021254837);
#31966=CONICAL_SURFACE('',#36165,126.75,1.10714871779408);
#31967=CONICAL_SURFACE('',#36177,3.02920176969664,1.10124348056693);
#31968=CONICAL_SURFACE('',#36180,1.5,0.631690634338971);
#31969=CONICAL_SURFACE('',#36218,7.,0.785398163397446);
#31970=CONICAL_SURFACE('',#36228,7.,0.785398163397446);
#31971=CONICAL_SURFACE('',#36232,7.,0.785398163397446);
#31972=CONICAL_SURFACE('',#36236,7.,0.785398163397446);
#31973=CONICAL_SURFACE('',#36240,7.,0.785398163397448);
#31974=CONICAL_SURFACE('',#36247,7.,0.785398163397448);
#31975=CONICAL_SURFACE('',#36248,7.,0.785398163397448);
#31976=CONICAL_SURFACE('',#36249,7.,0.785398163397448);
#31977=CONICAL_SURFACE('',#36256,25.2232233047034,0.392699081698712);
#31978=CONICAL_SURFACE('',#36261,25.,0.785398163397448);
#31979=CONICAL_SURFACE('',#36265,24.5267766952966,1.17809724509617);
#31980=CONICAL_SURFACE('',#36312,23.61565,1.17289539365476);
#31981=CONICAL_SURFACE('',#36318,17.72,0.785398163397448);
#31982=CONICAL_SURFACE('',#36322,15.72,0.610725964389208);
#31983=CONICAL_SURFACE('',#36324,13.72,0.785398163397451);
#31984=CONICAL_SURFACE('',#36337,12.3,1.01219701145133);
#31985=CONICAL_SURFACE('',#36338,12.35,0.785398163397447);
#31986=CONICAL_SURFACE('',#36342,24.69,0.785398163397445);
#31987=CONICAL_SURFACE('',#36350,29.59,0.785398163397446);
#31988=CONICAL_SURFACE('',#36364,32.385,0.785398163397449);
#31989=CONICAL_SURFACE('',#36368,32.385,0.785398163397448);
#31990=CONICAL_SURFACE('',#36369,23.95,0.548549402450529);
#31991=CONICAL_SURFACE('',#36371,22.62065,0.687037904785236);
#31992=CONICAL_SURFACE('',#36375,22.77065,0.801440737031442);
#31993=CONICAL_SURFACE('',#36378,29.1655,0.785398163397449);
#31994=CONICAL_SURFACE('',#36383,29.2655,0.78539816339745);
#31995=CONICAL_SURFACE('',#36387,28.358778116497,0.785398163397452);
#31996=CONICAL_SURFACE('',#36389,27.3267351683296,0.157079632679489);
#31997=CONICAL_SURFACE('',#36391,26.6550961100811,0.699606280388882);
#31998=CONICAL_SURFACE('',#36395,25.6346416389917,0.785398163397446);
#31999=CONICAL_SURFACE('',#36403,22.5243990607509,0.785398163397447);
#32000=CONICAL_SURFACE('',#36416,2.7,0.0349065850398862);
#32001=CONICAL_SURFACE('',#36429,2.7,0.0349065850398862);
#32002=CONICAL_SURFACE('',#36442,2.7,0.0349065850398862);
#32003=CONICAL_SURFACE('',#36455,2.7,0.0349065850398862);
#32004=CONICAL_SURFACE('',#36468,2.7,0.0349065850398862);
#32005=CONICAL_SURFACE('',#36481,2.7,0.0349065850398862);
#32006=CONICAL_SURFACE('',#36494,2.7,0.0349065850398862);
#32007=CONICAL_SURFACE('',#36507,2.7,0.0349065850398862);
#32008=CONICAL_SURFACE('',#36520,2.7,0.0349065850398862);
#32009=CONICAL_SURFACE('',#36533,2.7,0.0349065850398862);
#32010=CONICAL_SURFACE('',#36546,2.7,0.0349065850398862);
#32011=CONICAL_SURFACE('',#36559,2.7,0.0349065850398862);
#32012=CONICAL_SURFACE('',#36572,2.7,0.0349065850398862);
#32013=CONICAL_SURFACE('',#36585,2.7,0.0349065850398862);
#32014=CONICAL_SURFACE('',#36598,2.7,0.0349065850398862);
#32015=CONICAL_SURFACE('',#36611,2.7,0.0349065850398862);
#32016=CONICAL_SURFACE('',#36624,2.7,0.0349065850398862);
#32017=CONICAL_SURFACE('',#36637,2.7,0.0349065850398862);
#32018=CONICAL_SURFACE('',#36650,2.7,0.0349065850398862);
#32019=CONICAL_SURFACE('',#36663,2.7,0.0349065850398862);
#32020=CONICAL_SURFACE('',#36676,2.7,0.0349065850398862);
#32021=CONICAL_SURFACE('',#36689,2.7,0.0349065850398862);
#32022=CONICAL_SURFACE('',#36697,22.5743990607509,0.785398163397443);
#32023=CONICAL_SURFACE('',#36699,22.011553150687,0.0872664625997167);
#32024=CONICAL_SURFACE('',#36700,25.6346416389917,0.785398163397448);
#32025=CONICAL_SURFACE('',#36704,17.894,0.785398163397448);
#32026=CONICAL_SURFACE('',#36708,17.794,0.785398163397449);
#32027=CONICAL_SURFACE('',#36712,24.746,0.785398163397449);
#32028=CONICAL_SURFACE('',#36717,24.846,0.785398163397448);
#32029=CONICAL_SURFACE('',#36721,23.9381298772848,0.785398163397445);
#32030=CONICAL_SURFACE('',#36723,23.0066610487235,0.15707963267949);
#32031=CONICAL_SURFACE('',#36725,22.4355961100811,0.699606280388887);
#32032=CONICAL_SURFACE('',#36729,21.4356897166516,0.785398163397446);
#32033=CONICAL_SURFACE('',#36737,18.568471118769,0.785398163397449);
#32034=CONICAL_SURFACE('',#36750,2.5,0.0349065850398875);
#32035=CONICAL_SURFACE('',#36763,2.5,0.0349065850398875);
#32036=CONICAL_SURFACE('',#36776,2.5,0.0349065850398875);
#32037=CONICAL_SURFACE('',#36789,2.5,0.0349065850398875);
#32038=CONICAL_SURFACE('',#36802,2.5,0.0349065850398875);
#32039=CONICAL_SURFACE('',#36815,2.5,0.0349065850398875);
#32040=CONICAL_SURFACE('',#36828,2.5,0.0349065850398875);
#32041=CONICAL_SURFACE('',#36841,2.5,0.0349065850398875);
#32042=CONICAL_SURFACE('',#36854,2.5,0.0349065850398875);
#32043=CONICAL_SURFACE('',#36867,2.5,0.0349065850398875);
#32044=CONICAL_SURFACE('',#36880,2.5,0.0349065850398875);
#32045=CONICAL_SURFACE('',#36893,2.5,0.0349065850398875);
#32046=CONICAL_SURFACE('',#36906,2.5,0.0349065850398875);
#32047=CONICAL_SURFACE('',#36919,2.5,0.0349065850398875);
#32048=CONICAL_SURFACE('',#36932,2.5,0.0349065850398875);
#32049=CONICAL_SURFACE('',#36945,2.5,0.0349065850398875);
#32050=CONICAL_SURFACE('',#36958,2.5,0.0349065850398875);
#32051=CONICAL_SURFACE('',#36971,2.5,0.0349065850398875);
#32052=CONICAL_SURFACE('',#36984,2.5,0.0349065850398875);
#32053=CONICAL_SURFACE('',#36997,2.5,0.0349065850398875);
#32054=CONICAL_SURFACE('',#37005,18.618471118769,0.785398163397446);
#32055=CONICAL_SURFACE('',#37007,18.0894454950083,0.0872664625997163);
#32056=CONICAL_SURFACE('',#37008,21.4356897166516,0.785398163397451);
#32057=CONICAL_SURFACE('',#37012,13.894,0.785398163397448);
#32058=CONICAL_SURFACE('',#37016,13.794,0.785398163397449);
#32059=CONICAL_SURFACE('',#37032,20.35,0.982793723247326);
#32060=CONICAL_SURFACE('',#37036,20.35,0.982793723247327);
#32061=CONICAL_SURFACE('',#37042,19.8,1.20210042413685);
#32062=CONICAL_SURFACE('',#37052,13.,0.785398163397448);
#32063=CONICAL_SURFACE('',#37059,13.,0.785398163397448);
#32064=CONICAL_SURFACE('',#37064,19.8,1.20210042413685);
#32065=CONICAL_SURFACE('',#37068,19.8,1.20210042413685);
#32066=CONICAL_SURFACE('',#37074,19.8,1.20210042413685);
#32067=CONICAL_SURFACE('',#37091,13.,0.785398163397448);
#32068=CONICAL_SURFACE('',#37096,19.8,1.20210042413685);
#32069=CONICAL_SURFACE('',#37108,13.,0.785398163397446);
#32070=CONICAL_SURFACE('',#37121,13.,0.785398163397448);
#32071=CONICAL_SURFACE('',#37123,13.,0.785398163397448);
#32072=CONICAL_SURFACE('',#37127,13.,0.785398163397448);
#32073=CONICAL_SURFACE('',#37129,13.,0.785398163397448);
#32074=CONICAL_SURFACE('',#37140,13.,0.785398163397448);
#32075=CONICAL_SURFACE('',#37145,19.8,1.20210042413685);
#32076=CONICAL_SURFACE('',#37154,13.,0.785398163397448);
#32077=CONICAL_SURFACE('',#37157,13.,0.785398163397448);
#32078=CONICAL_SURFACE('',#37161,13.,0.785398163397448);
#32079=CONICAL_SURFACE('',#37171,19.8,1.20210042413685);
#32080=CONICAL_SURFACE('',#37173,13.075,0.74837804752352);
#32081=CONICAL_SURFACE('',#37186,1.85,0.785398163397437);
#32082=CONICAL_SURFACE('',#37197,1.75,0.785398163397437);
#32083=CONICAL_SURFACE('',#37207,1.75,0.785398163397437);
#32084=CONICAL_SURFACE('',#37216,20.9831675294297,1.3169225046995);
#32085=CONICAL_SURFACE('',#37221,22.1,1.18247760862243);
#32086=CONICAL_SURFACE('',#37224,19.75,1.45136740077656);
#32087=CONICAL_SURFACE('',#37226,23.1453899562452,0.98393788600994);
#32088=CONICAL_SURFACE('',#37229,24.,0.785398163397448);
#32089=CONICAL_SURFACE('',#37232,24.708659070475,0.567084583490677);
#32090=CONICAL_SURFACE('',#37235,25.2,0.348771003583908);
#32091=CONICAL_SURFACE('',#37238,25.5145642342283,0.174385501791952);
#32092=CONICAL_SURFACE('',#37246,24.82,0.785398163397448);
#32093=CONICAL_SURFACE('',#37254,26.2,1.24904577239825);
#32094=CONICAL_SURFACE('',#37258,19.55,1.44109378963898);
#32095=CONICAL_SURFACE('',#37260,21.65,1.17227388112848);
#32096=CONICAL_SURFACE('',#37262,23.3,0.750929062397939);
#32097=CONICAL_SURFACE('',#37264,24.4,0.41822432957923);
#32098=CONICAL_SURFACE('',#37266,24.56,0.0263675140393565);
#32099=CONICAL_SURFACE('',#37331,5.47677669529664,1.17809724509618);
#32100=CONICAL_SURFACE('',#37335,5.95,0.785398163397454);
#32101=CONICAL_SURFACE('',#37348,10.7,0.876058050598193);
#32102=CONICAL_SURFACE('',#37354,10.7,0.785398163397449);
#32103=CONICAL_SURFACE('',#37582,6.76,0.797743215241672);
#32104=CONICAL_SURFACE('',#37584,8.9203817394342,1.28983554566649);
#32105=CONICAL_SURFACE('',#37592,10.15,1.00887476453808);
#32106=CONICAL_SURFACE('',#37593,10.15,1.00887476453808);
#32107=CONICAL_SURFACE('',#37594,10.15,1.00887476453808);
#32108=CONICAL_SURFACE('',#37595,10.15,1.00887476453808);
#32109=CONICAL_SURFACE('',#37596,10.15,1.00887476453808);
#32110=CONICAL_SURFACE('',#37597,10.15,1.00887476453808);
#32111=CONICAL_SURFACE('',#37632,6.8,0.785398163397449);
#32112=CONICAL_SURFACE('',#37635,8.35,0.52183427981441);
#32113=ADVANCED_FACE('',(#3139),#31928,.T.);
#32114=ADVANCED_FACE('',(#3140),#31929,.T.);
#32115=ADVANCED_FACE('',(#3141),#2992,.T.);
#32116=ADVANCED_FACE('',(#3142),#31930,.T.);
#32117=ADVANCED_FACE('',(#3143,#1130),#1335,.T.);
#32118=ADVANCED_FACE('',(#3144),#31931,.F.);
#32119=ADVANCED_FACE('',(#3145),#2993,.F.);
#32120=ADVANCED_FACE('',(#3146,#1131),#1336,.T.);
#32121=ADVANCED_FACE('',(#3147),#31932,.T.);
#32122=ADVANCED_FACE('',(#3148),#31933,.T.);
#32123=ADVANCED_FACE('',(#3149,#1132),#1337,.T.);
#32124=ADVANCED_FACE('',(#3150),#31934,.T.);
#32125=ADVANCED_FACE('',(#3151),#31935,.T.);
#32126=ADVANCED_FACE('',(#3152),#31936,.T.);
#32127=ADVANCED_FACE('',(#3153),#31937,.T.);
#32128=ADVANCED_FACE('',(#3154),#31938,.T.);
#32129=ADVANCED_FACE('',(#3155),#31939,.T.);
#32130=ADVANCED_FACE('',(#3156),#31940,.T.);
#32131=ADVANCED_FACE('',(#3157),#31941,.T.);
#32132=ADVANCED_FACE('',(#3158),#31942,.T.);
#32133=ADVANCED_FACE('',(#3159),#31943,.T.);
#32134=ADVANCED_FACE('',(#3160,#1133,#1134,#1135,#1136,#1137,#1138,#1139,
#1140,#1141,#1142,#1143,#1144,#1145,#1146,#1147,#1148,#1149,#1150,#1151,
#1152,#1153,#1154,#1155,#1156,#1157,#1158,#1159,#1160,#1161,#1162,#1163,
#1164,#1165,#1166,#1167,#1168,#1169,#1170,#1171,#1172,#1173,#1174,#1175,
#1176,#1177,#1178,#1179,#1180,#1181,#1182,#1183,#1184,#1185,#1186,#1187,
#1188,#1189,#1190,#1191,#1192,#1193,#1194,#1195,#1196,#1197,#1198,#1199,
#1200,#1201,#1202,#1203),#2994,.T.);
#32135=ADVANCED_FACE('',(#3161),#31944,.T.);
#32136=ADVANCED_FACE('',(#3162),#31945,.T.);
#32137=ADVANCED_FACE('',(#3163),#31946,.T.);
#32138=ADVANCED_FACE('',(#3164),#31947,.T.);
#32139=ADVANCED_FACE('',(#3165),#31948,.T.);
#32140=ADVANCED_FACE('',(#3166),#31949,.T.);
#32141=ADVANCED_FACE('',(#3167),#31950,.T.);
#32142=ADVANCED_FACE('',(#3168),#31951,.T.);
#32143=ADVANCED_FACE('',(#3169),#31952,.T.);
#32144=ADVANCED_FACE('',(#3170),#31953,.T.);
#32145=ADVANCED_FACE('',(#3171),#2995,.T.);
#32146=ADVANCED_FACE('',(#3172),#2996,.T.);
#32147=ADVANCED_FACE('',(#3173),#2997,.T.);
#32148=ADVANCED_FACE('',(#3174),#2998,.T.);
#32149=ADVANCED_FACE('',(#3175),#2999,.T.);
#32150=ADVANCED_FACE('',(#3176),#3000,.T.);
#32151=ADVANCED_FACE('',(#3177,#1204,#1205,#1206,#1207,#1208,#1209),#1338,
 .T.);
#32152=ADVANCED_FACE('',(#3178),#1339,.T.);
#32153=ADVANCED_FACE('',(#3179),#1340,.T.);
#32154=ADVANCED_FACE('',(#3180),#1341,.T.);
#32155=ADVANCED_FACE('',(#3181),#1342,.T.);
#32156=ADVANCED_FACE('',(#3182),#1343,.T.);
#32157=ADVANCED_FACE('',(#3183),#1344,.T.);
#32158=ADVANCED_FACE('',(#3184),#1345,.T.);
#32159=ADVANCED_FACE('',(#3185),#1346,.T.);
#32160=ADVANCED_FACE('',(#3186),#1347,.T.);
#32161=ADVANCED_FACE('',(#3187),#1348,.T.);
#32162=ADVANCED_FACE('',(#3188),#1349,.T.);
#32163=ADVANCED_FACE('',(#3189),#1350,.T.);
#32164=ADVANCED_FACE('',(#3190),#1351,.T.);
#32165=ADVANCED_FACE('',(#3191),#1352,.T.);
#32166=ADVANCED_FACE('',(#3192),#1353,.T.);
#32167=ADVANCED_FACE('',(#3193),#1354,.T.);
#32168=ADVANCED_FACE('',(#3194),#1355,.T.);
#32169=ADVANCED_FACE('',(#3195),#1356,.T.);
#32170=ADVANCED_FACE('',(#3196),#1357,.T.);
#32171=ADVANCED_FACE('',(#3197),#1358,.T.);
#32172=ADVANCED_FACE('',(#3198),#1359,.T.);
#32173=ADVANCED_FACE('',(#3199),#1360,.T.);
#32174=ADVANCED_FACE('',(#3200),#1361,.T.);
#32175=ADVANCED_FACE('',(#3201),#1362,.T.);
#32176=ADVANCED_FACE('',(#3202),#1363,.T.);
#32177=ADVANCED_FACE('',(#3203),#1364,.T.);
#32178=ADVANCED_FACE('',(#3204),#1365,.F.);
#32179=ADVANCED_FACE('',(#3205),#1366,.T.);
#32180=ADVANCED_FACE('',(#3206),#1367,.T.);
#32181=ADVANCED_FACE('',(#3207),#1368,.T.);
#32182=ADVANCED_FACE('',(#3208),#1369,.T.);
#32183=ADVANCED_FACE('',(#3209),#1370,.T.);
#32184=ADVANCED_FACE('',(#3210),#1371,.T.);
#32185=ADVANCED_FACE('',(#3211),#1372,.T.);
#32186=ADVANCED_FACE('',(#3212),#1373,.T.);
#32187=ADVANCED_FACE('',(#3213),#1374,.T.);
#32188=ADVANCED_FACE('',(#3214),#1375,.T.);
#32189=ADVANCED_FACE('',(#3215),#1376,.T.);
#32190=ADVANCED_FACE('',(#3216),#1377,.T.);
#32191=ADVANCED_FACE('',(#3217),#1378,.T.);
#32192=ADVANCED_FACE('',(#3218),#1379,.T.);
#32193=ADVANCED_FACE('',(#3219),#1380,.T.);
#32194=ADVANCED_FACE('',(#3220),#1381,.T.);
#32195=ADVANCED_FACE('',(#3221),#1382,.T.);
#32196=ADVANCED_FACE('',(#3222),#1383,.T.);
#32197=ADVANCED_FACE('',(#3223),#1384,.T.);
#32198=ADVANCED_FACE('',(#3224),#1385,.T.);
#32199=ADVANCED_FACE('',(#3225),#1386,.T.);
#32200=ADVANCED_FACE('',(#3226),#1387,.T.);
#32201=ADVANCED_FACE('',(#3227),#1388,.T.);
#32202=ADVANCED_FACE('',(#3228),#1389,.T.);
#32203=ADVANCED_FACE('',(#3229),#1390,.T.);
#32204=ADVANCED_FACE('',(#3230),#1391,.T.);
#32205=ADVANCED_FACE('',(#3231),#1392,.T.);
#32206=ADVANCED_FACE('',(#3232),#1393,.F.);
#32207=ADVANCED_FACE('',(#3233),#1394,.T.);
#32208=ADVANCED_FACE('',(#3234),#1395,.T.);
#32209=ADVANCED_FACE('',(#3235),#1396,.T.);
#32210=ADVANCED_FACE('',(#3236),#1397,.T.);
#32211=ADVANCED_FACE('',(#3237),#1398,.T.);
#32212=ADVANCED_FACE('',(#3238),#1399,.T.);
#32213=ADVANCED_FACE('',(#3239),#1400,.T.);
#32214=ADVANCED_FACE('',(#3240),#1401,.T.);
#32215=ADVANCED_FACE('',(#3241),#1402,.T.);
#32216=ADVANCED_FACE('',(#3242),#1403,.T.);
#32217=ADVANCED_FACE('',(#3243),#1404,.T.);
#32218=ADVANCED_FACE('',(#3244),#1405,.T.);
#32219=ADVANCED_FACE('',(#3245),#1406,.T.);
#32220=ADVANCED_FACE('',(#3246),#1407,.T.);
#32221=ADVANCED_FACE('',(#3247),#1408,.F.);
#32222=ADVANCED_FACE('',(#3248),#1409,.T.);
#32223=ADVANCED_FACE('',(#3249),#1410,.T.);
#32224=ADVANCED_FACE('',(#3250),#1411,.T.);
#32225=ADVANCED_FACE('',(#3251),#1412,.T.);
#32226=ADVANCED_FACE('',(#3252),#1413,.T.);
#32227=ADVANCED_FACE('',(#3253),#1414,.T.);
#32228=ADVANCED_FACE('',(#3254),#1415,.T.);
#32229=ADVANCED_FACE('',(#3255),#1416,.T.);
#32230=ADVANCED_FACE('',(#3256),#1417,.T.);
#32231=ADVANCED_FACE('',(#3257),#1418,.T.);
#32232=ADVANCED_FACE('',(#3258),#1419,.T.);
#32233=ADVANCED_FACE('',(#3259),#1420,.T.);
#32234=ADVANCED_FACE('',(#3260),#1421,.T.);
#32235=ADVANCED_FACE('',(#3261),#1422,.T.);
#32236=ADVANCED_FACE('',(#3262),#1423,.T.);
#32237=ADVANCED_FACE('',(#3263),#1424,.T.);
#32238=ADVANCED_FACE('',(#3264),#1425,.T.);
#32239=ADVANCED_FACE('',(#3265),#1426,.T.);
#32240=ADVANCED_FACE('',(#3266),#1427,.T.);
#32241=ADVANCED_FACE('',(#3267),#1428,.T.);
#32242=ADVANCED_FACE('',(#3268),#1429,.T.);
#32243=ADVANCED_FACE('',(#3269),#1430,.T.);
#32244=ADVANCED_FACE('',(#3270),#1431,.T.);
#32245=ADVANCED_FACE('',(#3271),#1432,.T.);
#32246=ADVANCED_FACE('',(#3272),#1433,.T.);
#32247=ADVANCED_FACE('',(#3273),#1434,.T.);
#32248=ADVANCED_FACE('',(#3274),#1435,.T.);
#32249=ADVANCED_FACE('',(#3275),#1436,.T.);
#32250=ADVANCED_FACE('',(#3276),#1437,.F.);
#32251=ADVANCED_FACE('',(#3277),#1438,.T.);
#32252=ADVANCED_FACE('',(#3278),#1439,.T.);
#32253=ADVANCED_FACE('',(#3279),#1440,.T.);
#32254=ADVANCED_FACE('',(#3280),#1441,.T.);
#32255=ADVANCED_FACE('',(#3281),#1442,.T.);
#32256=ADVANCED_FACE('',(#3282),#1443,.T.);
#32257=ADVANCED_FACE('',(#3283),#1444,.T.);
#32258=ADVANCED_FACE('',(#3284),#1445,.T.);
#32259=ADVANCED_FACE('',(#3285),#1446,.T.);
#32260=ADVANCED_FACE('',(#3286),#1447,.T.);
#32261=ADVANCED_FACE('',(#3287),#1448,.T.);
#32262=ADVANCED_FACE('',(#3288),#1449,.T.);
#32263=ADVANCED_FACE('',(#3289),#1450,.T.);
#32264=ADVANCED_FACE('',(#3290),#1451,.T.);
#32265=ADVANCED_FACE('',(#3291),#1452,.T.);
#32266=ADVANCED_FACE('',(#3292),#1453,.T.);
#32267=ADVANCED_FACE('',(#3293),#1454,.T.);
#32268=ADVANCED_FACE('',(#3294),#1455,.T.);
#32269=ADVANCED_FACE('',(#3295),#1456,.T.);
#32270=ADVANCED_FACE('',(#3296),#1457,.T.);
#32271=ADVANCED_FACE('',(#3297),#1458,.T.);
#32272=ADVANCED_FACE('',(#3298),#1459,.T.);
#32273=ADVANCED_FACE('',(#3299),#1460,.T.);
#32274=ADVANCED_FACE('',(#3300),#1461,.T.);
#32275=ADVANCED_FACE('',(#3301),#1462,.T.);
#32276=ADVANCED_FACE('',(#3302),#1463,.T.);
#32277=ADVANCED_FACE('',(#3303),#1464,.T.);
#32278=ADVANCED_FACE('',(#3304),#1465,.F.);
#32279=ADVANCED_FACE('',(#3305),#1466,.T.);
#32280=ADVANCED_FACE('',(#3306),#1467,.T.);
#32281=ADVANCED_FACE('',(#3307),#1468,.T.);
#32282=ADVANCED_FACE('',(#3308),#1469,.T.);
#32283=ADVANCED_FACE('',(#3309),#1470,.T.);
#32284=ADVANCED_FACE('',(#3310),#1471,.T.);
#32285=ADVANCED_FACE('',(#3311),#1472,.T.);
#32286=ADVANCED_FACE('',(#3312),#1473,.T.);
#32287=ADVANCED_FACE('',(#3313),#1474,.T.);
#32288=ADVANCED_FACE('',(#3314),#1475,.T.);
#32289=ADVANCED_FACE('',(#3315),#1476,.T.);
#32290=ADVANCED_FACE('',(#3316),#1477,.T.);
#32291=ADVANCED_FACE('',(#3317),#1478,.T.);
#32292=ADVANCED_FACE('',(#3318),#1479,.T.);
#32293=ADVANCED_FACE('',(#3319),#1480,.F.);
#32294=ADVANCED_FACE('',(#3320),#1481,.T.);
#32295=ADVANCED_FACE('',(#3321),#1482,.T.);
#32296=ADVANCED_FACE('',(#3322),#1483,.T.);
#32297=ADVANCED_FACE('',(#3323),#1484,.T.);
#32298=ADVANCED_FACE('',(#3324),#1485,.T.);
#32299=ADVANCED_FACE('',(#3325),#1486,.T.);
#32300=ADVANCED_FACE('',(#3326),#1487,.T.);
#32301=ADVANCED_FACE('',(#3327),#1488,.T.);
#32302=ADVANCED_FACE('',(#3328),#1489,.T.);
#32303=ADVANCED_FACE('',(#3329),#1490,.T.);
#32304=ADVANCED_FACE('',(#3330),#1491,.T.);
#32305=ADVANCED_FACE('',(#3331),#1492,.T.);
#32306=ADVANCED_FACE('',(#3332),#1493,.T.);
#32307=ADVANCED_FACE('',(#3333),#1494,.T.);
#32308=ADVANCED_FACE('',(#3334),#1495,.T.);
#32309=ADVANCED_FACE('',(#3335),#1496,.T.);
#32310=ADVANCED_FACE('',(#3336),#1497,.T.);
#32311=ADVANCED_FACE('',(#3337),#1498,.T.);
#32312=ADVANCED_FACE('',(#3338),#1499,.T.);
#32313=ADVANCED_FACE('',(#3339),#1500,.T.);
#32314=ADVANCED_FACE('',(#3340),#1501,.T.);
#32315=ADVANCED_FACE('',(#3341),#1502,.T.);
#32316=ADVANCED_FACE('',(#3342),#1503,.T.);
#32317=ADVANCED_FACE('',(#3343),#1504,.T.);
#32318=ADVANCED_FACE('',(#3344),#1505,.T.);
#32319=ADVANCED_FACE('',(#3345),#1506,.T.);
#32320=ADVANCED_FACE('',(#3346),#1507,.T.);
#32321=ADVANCED_FACE('',(#3347),#1508,.T.);
#32322=ADVANCED_FACE('',(#3348),#1509,.F.);
#32323=ADVANCED_FACE('',(#3349),#1510,.T.);
#32324=ADVANCED_FACE('',(#3350),#1511,.T.);
#32325=ADVANCED_FACE('',(#3351),#1512,.T.);
#32326=ADVANCED_FACE('',(#3352),#1513,.T.);
#32327=ADVANCED_FACE('',(#3353),#1514,.T.);
#32328=ADVANCED_FACE('',(#3354),#1515,.T.);
#32329=ADVANCED_FACE('',(#3355),#1516,.T.);
#32330=ADVANCED_FACE('',(#3356),#1517,.T.);
#32331=ADVANCED_FACE('',(#3357),#1518,.T.);
#32332=ADVANCED_FACE('',(#3358),#1519,.T.);
#32333=ADVANCED_FACE('',(#3359),#1520,.T.);
#32334=ADVANCED_FACE('',(#3360),#1521,.T.);
#32335=ADVANCED_FACE('',(#3361),#1522,.T.);
#32336=ADVANCED_FACE('',(#3362),#1523,.T.);
#32337=ADVANCED_FACE('',(#3363),#1524,.T.);
#32338=ADVANCED_FACE('',(#3364),#1525,.T.);
#32339=ADVANCED_FACE('',(#3365),#1526,.T.);
#32340=ADVANCED_FACE('',(#3366),#1527,.T.);
#32341=ADVANCED_FACE('',(#3367),#1528,.T.);
#32342=ADVANCED_FACE('',(#3368),#1529,.T.);
#32343=ADVANCED_FACE('',(#3369),#1530,.T.);
#32344=ADVANCED_FACE('',(#3370),#1531,.T.);
#32345=ADVANCED_FACE('',(#3371),#1532,.T.);
#32346=ADVANCED_FACE('',(#3372),#1533,.T.);
#32347=ADVANCED_FACE('',(#3373),#1534,.T.);
#32348=ADVANCED_FACE('',(#3374),#1535,.T.);
#32349=ADVANCED_FACE('',(#3375),#1536,.T.);
#32350=ADVANCED_FACE('',(#3376),#1537,.F.);
#32351=ADVANCED_FACE('',(#3377),#1538,.T.);
#32352=ADVANCED_FACE('',(#3378),#1539,.T.);
#32353=ADVANCED_FACE('',(#3379),#1540,.T.);
#32354=ADVANCED_FACE('',(#3380),#1541,.T.);
#32355=ADVANCED_FACE('',(#3381),#1542,.T.);
#32356=ADVANCED_FACE('',(#3382),#1543,.T.);
#32357=ADVANCED_FACE('',(#3383),#1544,.T.);
#32358=ADVANCED_FACE('',(#3384),#1545,.T.);
#32359=ADVANCED_FACE('',(#3385),#1546,.T.);
#32360=ADVANCED_FACE('',(#3386),#1547,.T.);
#32361=ADVANCED_FACE('',(#3387),#1548,.T.);
#32362=ADVANCED_FACE('',(#3388),#1549,.T.);
#32363=ADVANCED_FACE('',(#3389),#1550,.T.);
#32364=ADVANCED_FACE('',(#3390),#1551,.T.);
#32365=ADVANCED_FACE('',(#3391),#1552,.F.);
#32366=ADVANCED_FACE('',(#3392),#1553,.T.);
#32367=ADVANCED_FACE('',(#3393),#1554,.T.);
#32368=ADVANCED_FACE('',(#3394),#1555,.T.);
#32369=ADVANCED_FACE('',(#3395),#1556,.T.);
#32370=ADVANCED_FACE('',(#3396),#1557,.T.);
#32371=ADVANCED_FACE('',(#3397),#1558,.T.);
#32372=ADVANCED_FACE('',(#3398),#1559,.T.);
#32373=ADVANCED_FACE('',(#3399),#1560,.T.);
#32374=ADVANCED_FACE('',(#3400),#1561,.T.);
#32375=ADVANCED_FACE('',(#3401),#1562,.T.);
#32376=ADVANCED_FACE('',(#3402),#1563,.T.);
#32377=ADVANCED_FACE('',(#3403),#1564,.T.);
#32378=ADVANCED_FACE('',(#3404),#1565,.T.);
#32379=ADVANCED_FACE('',(#3405),#1566,.T.);
#32380=ADVANCED_FACE('',(#3406),#1567,.T.);
#32381=ADVANCED_FACE('',(#3407),#1568,.T.);
#32382=ADVANCED_FACE('',(#3408),#1569,.T.);
#32383=ADVANCED_FACE('',(#3409),#1570,.T.);
#32384=ADVANCED_FACE('',(#3410),#1571,.T.);
#32385=ADVANCED_FACE('',(#3411),#1572,.T.);
#32386=ADVANCED_FACE('',(#3412),#1573,.T.);
#32387=ADVANCED_FACE('',(#3413),#1574,.T.);
#32388=ADVANCED_FACE('',(#3414),#1575,.T.);
#32389=ADVANCED_FACE('',(#3415),#1576,.T.);
#32390=ADVANCED_FACE('',(#3416),#1577,.T.);
#32391=ADVANCED_FACE('',(#3417),#1578,.T.);
#32392=ADVANCED_FACE('',(#3418),#1579,.T.);
#32393=ADVANCED_FACE('',(#3419),#1580,.T.);
#32394=ADVANCED_FACE('',(#3420),#1581,.F.);
#32395=ADVANCED_FACE('',(#3421),#1582,.T.);
#32396=ADVANCED_FACE('',(#3422),#1583,.T.);
#32397=ADVANCED_FACE('',(#3423),#1584,.T.);
#32398=ADVANCED_FACE('',(#3424),#1585,.T.);
#32399=ADVANCED_FACE('',(#3425),#1586,.T.);
#32400=ADVANCED_FACE('',(#3426),#1587,.T.);
#32401=ADVANCED_FACE('',(#3427),#1588,.T.);
#32402=ADVANCED_FACE('',(#3428),#1589,.T.);
#32403=ADVANCED_FACE('',(#3429),#1590,.T.);
#32404=ADVANCED_FACE('',(#3430),#1591,.T.);
#32405=ADVANCED_FACE('',(#3431),#1592,.T.);
#32406=ADVANCED_FACE('',(#3432),#1593,.T.);
#32407=ADVANCED_FACE('',(#3433),#1594,.T.);
#32408=ADVANCED_FACE('',(#3434),#1595,.T.);
#32409=ADVANCED_FACE('',(#3435),#1596,.T.);
#32410=ADVANCED_FACE('',(#3436),#1597,.T.);
#32411=ADVANCED_FACE('',(#3437),#1598,.T.);
#32412=ADVANCED_FACE('',(#3438),#1599,.T.);
#32413=ADVANCED_FACE('',(#3439),#1600,.T.);
#32414=ADVANCED_FACE('',(#3440),#1601,.T.);
#32415=ADVANCED_FACE('',(#3441),#1602,.T.);
#32416=ADVANCED_FACE('',(#3442),#1603,.T.);
#32417=ADVANCED_FACE('',(#3443),#1604,.T.);
#32418=ADVANCED_FACE('',(#3444),#1605,.T.);
#32419=ADVANCED_FACE('',(#3445),#1606,.T.);
#32420=ADVANCED_FACE('',(#3446),#1607,.T.);
#32421=ADVANCED_FACE('',(#3447),#1608,.T.);
#32422=ADVANCED_FACE('',(#3448),#1609,.F.);
#32423=ADVANCED_FACE('',(#3449),#1610,.T.);
#32424=ADVANCED_FACE('',(#3450),#1611,.T.);
#32425=ADVANCED_FACE('',(#3451),#1612,.T.);
#32426=ADVANCED_FACE('',(#3452),#1613,.T.);
#32427=ADVANCED_FACE('',(#3453),#1614,.T.);
#32428=ADVANCED_FACE('',(#3454),#1615,.T.);
#32429=ADVANCED_FACE('',(#3455),#1616,.T.);
#32430=ADVANCED_FACE('',(#3456),#1617,.T.);
#32431=ADVANCED_FACE('',(#3457),#1618,.T.);
#32432=ADVANCED_FACE('',(#3458),#1619,.T.);
#32433=ADVANCED_FACE('',(#3459),#1620,.T.);
#32434=ADVANCED_FACE('',(#3460),#1621,.T.);
#32435=ADVANCED_FACE('',(#3461),#1622,.T.);
#32436=ADVANCED_FACE('',(#3462),#1623,.T.);
#32437=ADVANCED_FACE('',(#3463),#1624,.F.);
#32438=ADVANCED_FACE('',(#3464),#1625,.T.);
#32439=ADVANCED_FACE('',(#3465),#1626,.T.);
#32440=ADVANCED_FACE('',(#3466),#1627,.T.);
#32441=ADVANCED_FACE('',(#3467),#1628,.T.);
#32442=ADVANCED_FACE('',(#3468),#1629,.T.);
#32443=ADVANCED_FACE('',(#3469),#1630,.T.);
#32444=ADVANCED_FACE('',(#3470),#1631,.T.);
#32445=ADVANCED_FACE('',(#3471),#1632,.T.);
#32446=ADVANCED_FACE('',(#3472),#1633,.T.);
#32447=ADVANCED_FACE('',(#3473),#1634,.T.);
#32448=ADVANCED_FACE('',(#3474),#1635,.T.);
#32449=ADVANCED_FACE('',(#3475),#1636,.T.);
#32450=ADVANCED_FACE('',(#3476),#1637,.T.);
#32451=ADVANCED_FACE('',(#3477),#1638,.T.);
#32452=ADVANCED_FACE('',(#3478),#1639,.T.);
#32453=ADVANCED_FACE('',(#3479),#1640,.T.);
#32454=ADVANCED_FACE('',(#3480),#1641,.T.);
#32455=ADVANCED_FACE('',(#3481),#1642,.T.);
#32456=ADVANCED_FACE('',(#3482),#1643,.T.);
#32457=ADVANCED_FACE('',(#3483),#1644,.T.);
#32458=ADVANCED_FACE('',(#3484),#1645,.T.);
#32459=ADVANCED_FACE('',(#3485),#1646,.T.);
#32460=ADVANCED_FACE('',(#3486),#1647,.T.);
#32461=ADVANCED_FACE('',(#3487),#1648,.T.);
#32462=ADVANCED_FACE('',(#3488),#1649,.T.);
#32463=ADVANCED_FACE('',(#3489),#1650,.T.);
#32464=ADVANCED_FACE('',(#3490),#1651,.T.);
#32465=ADVANCED_FACE('',(#3491),#1652,.T.);
#32466=ADVANCED_FACE('',(#3492),#1653,.F.);
#32467=ADVANCED_FACE('',(#3493),#1654,.T.);
#32468=ADVANCED_FACE('',(#3494),#1655,.T.);
#32469=ADVANCED_FACE('',(#3495),#1656,.T.);
#32470=ADVANCED_FACE('',(#3496),#1657,.T.);
#32471=ADVANCED_FACE('',(#3497),#1658,.T.);
#32472=ADVANCED_FACE('',(#3498),#1659,.T.);
#32473=ADVANCED_FACE('',(#3499),#1660,.T.);
#32474=ADVANCED_FACE('',(#3500),#1661,.T.);
#32475=ADVANCED_FACE('',(#3501),#1662,.T.);
#32476=ADVANCED_FACE('',(#3502),#1663,.T.);
#32477=ADVANCED_FACE('',(#3503),#1664,.T.);
#32478=ADVANCED_FACE('',(#3504),#1665,.T.);
#32479=ADVANCED_FACE('',(#3505),#1666,.T.);
#32480=ADVANCED_FACE('',(#3506),#1667,.T.);
#32481=ADVANCED_FACE('',(#3507),#1668,.T.);
#32482=ADVANCED_FACE('',(#3508),#1669,.T.);
#32483=ADVANCED_FACE('',(#3509),#1670,.T.);
#32484=ADVANCED_FACE('',(#3510),#1671,.T.);
#32485=ADVANCED_FACE('',(#3511),#1672,.T.);
#32486=ADVANCED_FACE('',(#3512),#1673,.T.);
#32487=ADVANCED_FACE('',(#3513),#1674,.T.);
#32488=ADVANCED_FACE('',(#3514),#1675,.T.);
#32489=ADVANCED_FACE('',(#3515),#1676,.T.);
#32490=ADVANCED_FACE('',(#3516),#1677,.T.);
#32491=ADVANCED_FACE('',(#3517),#1678,.T.);
#32492=ADVANCED_FACE('',(#3518),#1679,.T.);
#32493=ADVANCED_FACE('',(#3519),#1680,.T.);
#32494=ADVANCED_FACE('',(#3520),#1681,.F.);
#32495=ADVANCED_FACE('',(#3521),#1682,.T.);
#32496=ADVANCED_FACE('',(#3522),#1683,.T.);
#32497=ADVANCED_FACE('',(#3523),#1684,.T.);
#32498=ADVANCED_FACE('',(#3524),#1685,.T.);
#32499=ADVANCED_FACE('',(#3525),#1686,.T.);
#32500=ADVANCED_FACE('',(#3526),#1687,.T.);
#32501=ADVANCED_FACE('',(#3527),#1688,.T.);
#32502=ADVANCED_FACE('',(#3528),#1689,.T.);
#32503=ADVANCED_FACE('',(#3529),#1690,.T.);
#32504=ADVANCED_FACE('',(#3530),#1691,.T.);
#32505=ADVANCED_FACE('',(#3531),#1692,.T.);
#32506=ADVANCED_FACE('',(#3532),#1693,.T.);
#32507=ADVANCED_FACE('',(#3533),#1694,.T.);
#32508=ADVANCED_FACE('',(#3534),#1695,.T.);
#32509=ADVANCED_FACE('',(#3535),#1696,.F.);
#32510=ADVANCED_FACE('',(#3536),#1697,.T.);
#32511=ADVANCED_FACE('',(#3537),#1698,.T.);
#32512=ADVANCED_FACE('',(#3538),#1699,.T.);
#32513=ADVANCED_FACE('',(#3539),#1700,.T.);
#32514=ADVANCED_FACE('',(#3540),#1701,.T.);
#32515=ADVANCED_FACE('',(#3541),#1702,.T.);
#32516=ADVANCED_FACE('',(#3542),#1703,.T.);
#32517=ADVANCED_FACE('',(#3543),#1704,.T.);
#32518=ADVANCED_FACE('',(#3544),#1705,.T.);
#32519=ADVANCED_FACE('',(#3545),#1706,.T.);
#32520=ADVANCED_FACE('',(#3546),#1707,.T.);
#32521=ADVANCED_FACE('',(#3547),#1708,.T.);
#32522=ADVANCED_FACE('',(#3548),#1709,.T.);
#32523=ADVANCED_FACE('',(#3549),#1710,.T.);
#32524=ADVANCED_FACE('',(#3550),#1711,.T.);
#32525=ADVANCED_FACE('',(#3551),#1712,.T.);
#32526=ADVANCED_FACE('',(#3552),#1713,.T.);
#32527=ADVANCED_FACE('',(#3553),#1714,.T.);
#32528=ADVANCED_FACE('',(#3554),#1715,.T.);
#32529=ADVANCED_FACE('',(#3555),#1716,.T.);
#32530=ADVANCED_FACE('',(#3556),#1717,.T.);
#32531=ADVANCED_FACE('',(#3557),#1718,.T.);
#32532=ADVANCED_FACE('',(#3558),#1719,.T.);
#32533=ADVANCED_FACE('',(#3559),#1720,.T.);
#32534=ADVANCED_FACE('',(#3560),#1721,.T.);
#32535=ADVANCED_FACE('',(#3561),#1722,.T.);
#32536=ADVANCED_FACE('',(#3562),#1723,.T.);
#32537=ADVANCED_FACE('',(#3563),#1724,.T.);
#32538=ADVANCED_FACE('',(#3564),#1725,.F.);
#32539=ADVANCED_FACE('',(#3565),#1726,.T.);
#32540=ADVANCED_FACE('',(#3566),#1727,.T.);
#32541=ADVANCED_FACE('',(#3567),#1728,.T.);
#32542=ADVANCED_FACE('',(#3568),#1729,.T.);
#32543=ADVANCED_FACE('',(#3569),#1730,.T.);
#32544=ADVANCED_FACE('',(#3570),#1731,.T.);
#32545=ADVANCED_FACE('',(#3571),#1732,.T.);
#32546=ADVANCED_FACE('',(#3572),#1733,.T.);
#32547=ADVANCED_FACE('',(#3573),#1734,.T.);
#32548=ADVANCED_FACE('',(#3574),#1735,.T.);
#32549=ADVANCED_FACE('',(#3575),#1736,.T.);
#32550=ADVANCED_FACE('',(#3576),#1737,.T.);
#32551=ADVANCED_FACE('',(#3577),#1738,.T.);
#32552=ADVANCED_FACE('',(#3578),#1739,.T.);
#32553=ADVANCED_FACE('',(#3579),#1740,.T.);
#32554=ADVANCED_FACE('',(#3580),#1741,.T.);
#32555=ADVANCED_FACE('',(#3581),#1742,.T.);
#32556=ADVANCED_FACE('',(#3582),#1743,.T.);
#32557=ADVANCED_FACE('',(#3583),#1744,.T.);
#32558=ADVANCED_FACE('',(#3584),#1745,.T.);
#32559=ADVANCED_FACE('',(#3585),#1746,.T.);
#32560=ADVANCED_FACE('',(#3586),#1747,.T.);
#32561=ADVANCED_FACE('',(#3587),#1748,.T.);
#32562=ADVANCED_FACE('',(#3588),#1749,.T.);
#32563=ADVANCED_FACE('',(#3589),#1750,.T.);
#32564=ADVANCED_FACE('',(#3590),#1751,.T.);
#32565=ADVANCED_FACE('',(#3591),#1752,.T.);
#32566=ADVANCED_FACE('',(#3592),#1753,.F.);
#32567=ADVANCED_FACE('',(#3593),#1754,.T.);
#32568=ADVANCED_FACE('',(#3594),#1755,.T.);
#32569=ADVANCED_FACE('',(#3595),#1756,.T.);
#32570=ADVANCED_FACE('',(#3596),#1757,.T.);
#32571=ADVANCED_FACE('',(#3597),#1758,.T.);
#32572=ADVANCED_FACE('',(#3598),#1759,.T.);
#32573=ADVANCED_FACE('',(#3599),#1760,.T.);
#32574=ADVANCED_FACE('',(#3600),#1761,.T.);
#32575=ADVANCED_FACE('',(#3601),#1762,.T.);
#32576=ADVANCED_FACE('',(#3602),#1763,.T.);
#32577=ADVANCED_FACE('',(#3603),#1764,.T.);
#32578=ADVANCED_FACE('',(#3604),#1765,.T.);
#32579=ADVANCED_FACE('',(#3605),#1766,.T.);
#32580=ADVANCED_FACE('',(#3606),#1767,.T.);
#32581=ADVANCED_FACE('',(#3607),#1768,.F.);
#32582=ADVANCED_FACE('',(#3608),#1769,.T.);
#32583=ADVANCED_FACE('',(#3609),#1770,.T.);
#32584=ADVANCED_FACE('',(#3610),#1771,.T.);
#32585=ADVANCED_FACE('',(#3611),#1772,.T.);
#32586=ADVANCED_FACE('',(#3612),#1773,.T.);
#32587=ADVANCED_FACE('',(#3613),#1774,.T.);
#32588=ADVANCED_FACE('',(#3614),#1775,.T.);
#32589=ADVANCED_FACE('',(#3615),#1776,.T.);
#32590=ADVANCED_FACE('',(#3616),#1777,.T.);
#32591=ADVANCED_FACE('',(#3617),#1778,.T.);
#32592=ADVANCED_FACE('',(#3618),#1779,.T.);
#32593=ADVANCED_FACE('',(#3619),#1780,.T.);
#32594=ADVANCED_FACE('',(#3620),#1781,.T.);
#32595=ADVANCED_FACE('',(#3621),#1782,.T.);
#32596=ADVANCED_FACE('',(#3622),#1783,.T.);
#32597=ADVANCED_FACE('',(#3623),#1784,.T.);
#32598=ADVANCED_FACE('',(#3624),#1785,.T.);
#32599=ADVANCED_FACE('',(#3625),#1786,.T.);
#32600=ADVANCED_FACE('',(#3626),#1787,.T.);
#32601=ADVANCED_FACE('',(#3627),#1788,.T.);
#32602=ADVANCED_FACE('',(#3628),#1789,.T.);
#32603=ADVANCED_FACE('',(#3629),#1790,.T.);
#32604=ADVANCED_FACE('',(#3630),#1791,.T.);
#32605=ADVANCED_FACE('',(#3631),#1792,.T.);
#32606=ADVANCED_FACE('',(#3632),#1793,.T.);
#32607=ADVANCED_FACE('',(#3633),#1794,.T.);
#32608=ADVANCED_FACE('',(#3634),#1795,.T.);
#32609=ADVANCED_FACE('',(#3635),#1796,.T.);
#32610=ADVANCED_FACE('',(#3636),#1797,.F.);
#32611=ADVANCED_FACE('',(#3637),#1798,.T.);
#32612=ADVANCED_FACE('',(#3638),#1799,.T.);
#32613=ADVANCED_FACE('',(#3639),#1800,.T.);
#32614=ADVANCED_FACE('',(#3640),#1801,.T.);
#32615=ADVANCED_FACE('',(#3641),#1802,.T.);
#32616=ADVANCED_FACE('',(#3642),#1803,.T.);
#32617=ADVANCED_FACE('',(#3643),#1804,.T.);
#32618=ADVANCED_FACE('',(#3644),#1805,.T.);
#32619=ADVANCED_FACE('',(#3645),#1806,.T.);
#32620=ADVANCED_FACE('',(#3646),#1807,.T.);
#32621=ADVANCED_FACE('',(#3647),#1808,.T.);
#32622=ADVANCED_FACE('',(#3648),#1809,.T.);
#32623=ADVANCED_FACE('',(#3649),#1810,.T.);
#32624=ADVANCED_FACE('',(#3650),#1811,.T.);
#32625=ADVANCED_FACE('',(#3651),#1812,.T.);
#32626=ADVANCED_FACE('',(#3652),#1813,.T.);
#32627=ADVANCED_FACE('',(#3653),#1814,.T.);
#32628=ADVANCED_FACE('',(#3654),#1815,.T.);
#32629=ADVANCED_FACE('',(#3655),#1816,.T.);
#32630=ADVANCED_FACE('',(#3656),#1817,.T.);
#32631=ADVANCED_FACE('',(#3657),#1818,.T.);
#32632=ADVANCED_FACE('',(#3658),#1819,.T.);
#32633=ADVANCED_FACE('',(#3659),#1820,.T.);
#32634=ADVANCED_FACE('',(#3660),#1821,.T.);
#32635=ADVANCED_FACE('',(#3661),#1822,.T.);
#32636=ADVANCED_FACE('',(#3662),#1823,.T.);
#32637=ADVANCED_FACE('',(#3663),#1824,.T.);
#32638=ADVANCED_FACE('',(#3664),#1825,.F.);
#32639=ADVANCED_FACE('',(#3665),#1826,.T.);
#32640=ADVANCED_FACE('',(#3666),#1827,.T.);
#32641=ADVANCED_FACE('',(#3667),#1828,.T.);
#32642=ADVANCED_FACE('',(#3668),#1829,.T.);
#32643=ADVANCED_FACE('',(#3669),#1830,.T.);
#32644=ADVANCED_FACE('',(#3670),#1831,.T.);
#32645=ADVANCED_FACE('',(#3671),#1832,.T.);
#32646=ADVANCED_FACE('',(#3672),#1833,.T.);
#32647=ADVANCED_FACE('',(#3673),#1834,.T.);
#32648=ADVANCED_FACE('',(#3674),#1835,.T.);
#32649=ADVANCED_FACE('',(#3675),#1836,.T.);
#32650=ADVANCED_FACE('',(#3676),#1837,.T.);
#32651=ADVANCED_FACE('',(#3677),#1838,.T.);
#32652=ADVANCED_FACE('',(#3678),#1839,.T.);
#32653=ADVANCED_FACE('',(#3679),#1840,.F.);
#32654=ADVANCED_FACE('',(#3680),#1841,.T.);
#32655=ADVANCED_FACE('',(#3681),#1842,.T.);
#32656=ADVANCED_FACE('',(#3682),#1843,.T.);
#32657=ADVANCED_FACE('',(#3683),#1844,.T.);
#32658=ADVANCED_FACE('',(#3684),#1845,.T.);
#32659=ADVANCED_FACE('',(#3685),#1846,.T.);
#32660=ADVANCED_FACE('',(#3686),#1847,.T.);
#32661=ADVANCED_FACE('',(#3687),#1848,.T.);
#32662=ADVANCED_FACE('',(#3688),#1849,.T.);
#32663=ADVANCED_FACE('',(#3689),#1850,.T.);
#32664=ADVANCED_FACE('',(#3690),#1851,.T.);
#32665=ADVANCED_FACE('',(#3691),#1852,.T.);
#32666=ADVANCED_FACE('',(#3692),#1853,.T.);
#32667=ADVANCED_FACE('',(#3693),#1854,.T.);
#32668=ADVANCED_FACE('',(#3694),#1855,.T.);
#32669=ADVANCED_FACE('',(#3695),#1856,.T.);
#32670=ADVANCED_FACE('',(#3696),#1857,.T.);
#32671=ADVANCED_FACE('',(#3697),#1858,.T.);
#32672=ADVANCED_FACE('',(#3698),#1859,.T.);
#32673=ADVANCED_FACE('',(#3699),#1860,.T.);
#32674=ADVANCED_FACE('',(#3700),#1861,.T.);
#32675=ADVANCED_FACE('',(#3701),#1862,.T.);
#32676=ADVANCED_FACE('',(#3702),#1863,.T.);
#32677=ADVANCED_FACE('',(#3703),#1864,.T.);
#32678=ADVANCED_FACE('',(#3704),#1865,.T.);
#32679=ADVANCED_FACE('',(#3705),#1866,.T.);
#32680=ADVANCED_FACE('',(#3706),#1867,.T.);
#32681=ADVANCED_FACE('',(#3707),#1868,.T.);
#32682=ADVANCED_FACE('',(#3708),#1869,.F.);
#32683=ADVANCED_FACE('',(#3709),#1870,.T.);
#32684=ADVANCED_FACE('',(#3710),#1871,.T.);
#32685=ADVANCED_FACE('',(#3711),#1872,.T.);
#32686=ADVANCED_FACE('',(#3712),#1873,.T.);
#32687=ADVANCED_FACE('',(#3713),#1874,.T.);
#32688=ADVANCED_FACE('',(#3714),#1875,.T.);
#32689=ADVANCED_FACE('',(#3715),#1876,.T.);
#32690=ADVANCED_FACE('',(#3716),#1877,.T.);
#32691=ADVANCED_FACE('',(#3717),#1878,.T.);
#32692=ADVANCED_FACE('',(#3718),#1879,.T.);
#32693=ADVANCED_FACE('',(#3719),#1880,.T.);
#32694=ADVANCED_FACE('',(#3720),#1881,.T.);
#32695=ADVANCED_FACE('',(#3721),#1882,.T.);
#32696=ADVANCED_FACE('',(#3722),#1883,.T.);
#32697=ADVANCED_FACE('',(#3723),#1884,.T.);
#32698=ADVANCED_FACE('',(#3724),#1885,.T.);
#32699=ADVANCED_FACE('',(#3725),#1886,.T.);
#32700=ADVANCED_FACE('',(#3726),#1887,.T.);
#32701=ADVANCED_FACE('',(#3727),#1888,.T.);
#32702=ADVANCED_FACE('',(#3728),#1889,.T.);
#32703=ADVANCED_FACE('',(#3729),#1890,.T.);
#32704=ADVANCED_FACE('',(#3730),#1891,.T.);
#32705=ADVANCED_FACE('',(#3731),#1892,.T.);
#32706=ADVANCED_FACE('',(#3732),#1893,.T.);
#32707=ADVANCED_FACE('',(#3733),#1894,.T.);
#32708=ADVANCED_FACE('',(#3734),#1895,.T.);
#32709=ADVANCED_FACE('',(#3735),#1896,.T.);
#32710=ADVANCED_FACE('',(#3736),#1897,.F.);
#32711=ADVANCED_FACE('',(#3737),#1898,.T.);
#32712=ADVANCED_FACE('',(#3738),#1899,.T.);
#32713=ADVANCED_FACE('',(#3739),#1900,.T.);
#32714=ADVANCED_FACE('',(#3740),#1901,.T.);
#32715=ADVANCED_FACE('',(#3741),#1902,.T.);
#32716=ADVANCED_FACE('',(#3742),#1903,.T.);
#32717=ADVANCED_FACE('',(#3743),#1904,.T.);
#32718=ADVANCED_FACE('',(#3744),#1905,.T.);
#32719=ADVANCED_FACE('',(#3745),#1906,.T.);
#32720=ADVANCED_FACE('',(#3746),#1907,.T.);
#32721=ADVANCED_FACE('',(#3747),#1908,.T.);
#32722=ADVANCED_FACE('',(#3748),#1909,.T.);
#32723=ADVANCED_FACE('',(#3749),#1910,.T.);
#32724=ADVANCED_FACE('',(#3750),#1911,.T.);
#32725=ADVANCED_FACE('',(#3751),#1912,.F.);
#32726=ADVANCED_FACE('',(#3752),#1913,.T.);
#32727=ADVANCED_FACE('',(#3753),#1914,.T.);
#32728=ADVANCED_FACE('',(#3754),#1915,.T.);
#32729=ADVANCED_FACE('',(#3755),#1916,.T.);
#32730=ADVANCED_FACE('',(#3756),#1917,.T.);
#32731=ADVANCED_FACE('',(#3757),#1918,.T.);
#32732=ADVANCED_FACE('',(#3758),#1919,.T.);
#32733=ADVANCED_FACE('',(#3759),#1920,.T.);
#32734=ADVANCED_FACE('',(#3760),#1921,.T.);
#32735=ADVANCED_FACE('',(#3761),#1922,.T.);
#32736=ADVANCED_FACE('',(#3762),#1923,.T.);
#32737=ADVANCED_FACE('',(#3763),#1924,.T.);
#32738=ADVANCED_FACE('',(#3764),#1925,.T.);
#32739=ADVANCED_FACE('',(#3765),#1926,.T.);
#32740=ADVANCED_FACE('',(#3766),#1927,.T.);
#32741=ADVANCED_FACE('',(#3767),#1928,.T.);
#32742=ADVANCED_FACE('',(#3768),#1929,.T.);
#32743=ADVANCED_FACE('',(#3769),#1930,.T.);
#32744=ADVANCED_FACE('',(#3770),#1931,.T.);
#32745=ADVANCED_FACE('',(#3771),#1932,.T.);
#32746=ADVANCED_FACE('',(#3772),#1933,.T.);
#32747=ADVANCED_FACE('',(#3773),#1934,.T.);
#32748=ADVANCED_FACE('',(#3774),#1935,.T.);
#32749=ADVANCED_FACE('',(#3775),#1936,.T.);
#32750=ADVANCED_FACE('',(#3776),#1937,.T.);
#32751=ADVANCED_FACE('',(#3777),#1938,.T.);
#32752=ADVANCED_FACE('',(#3778),#1939,.T.);
#32753=ADVANCED_FACE('',(#3779),#1940,.T.);
#32754=ADVANCED_FACE('',(#3780),#1941,.F.);
#32755=ADVANCED_FACE('',(#3781),#1942,.T.);
#32756=ADVANCED_FACE('',(#3782),#1943,.T.);
#32757=ADVANCED_FACE('',(#3783),#1944,.T.);
#32758=ADVANCED_FACE('',(#3784),#1945,.T.);
#32759=ADVANCED_FACE('',(#3785),#1946,.T.);
#32760=ADVANCED_FACE('',(#3786),#1947,.T.);
#32761=ADVANCED_FACE('',(#3787),#1948,.T.);
#32762=ADVANCED_FACE('',(#3788),#1949,.T.);
#32763=ADVANCED_FACE('',(#3789),#1950,.T.);
#32764=ADVANCED_FACE('',(#3790),#1951,.T.);
#32765=ADVANCED_FACE('',(#3791),#1952,.T.);
#32766=ADVANCED_FACE('',(#3792),#1953,.T.);
#32767=ADVANCED_FACE('',(#3793),#1954,.T.);
#32768=ADVANCED_FACE('',(#3794),#1955,.T.);
#32769=ADVANCED_FACE('',(#3795),#1956,.T.);
#32770=ADVANCED_FACE('',(#3796),#1957,.T.);
#32771=ADVANCED_FACE('',(#3797),#1958,.T.);
#32772=ADVANCED_FACE('',(#3798),#1959,.T.);
#32773=ADVANCED_FACE('',(#3799),#1960,.T.);
#32774=ADVANCED_FACE('',(#3800),#1961,.T.);
#32775=ADVANCED_FACE('',(#3801),#1962,.T.);
#32776=ADVANCED_FACE('',(#3802),#1963,.T.);
#32777=ADVANCED_FACE('',(#3803),#1964,.T.);
#32778=ADVANCED_FACE('',(#3804),#1965,.T.);
#32779=ADVANCED_FACE('',(#3805),#1966,.T.);
#32780=ADVANCED_FACE('',(#3806),#1967,.T.);
#32781=ADVANCED_FACE('',(#3807),#1968,.T.);
#32782=ADVANCED_FACE('',(#3808),#1969,.F.);
#32783=ADVANCED_FACE('',(#3809),#1970,.T.);
#32784=ADVANCED_FACE('',(#3810),#1971,.T.);
#32785=ADVANCED_FACE('',(#3811),#1972,.T.);
#32786=ADVANCED_FACE('',(#3812),#1973,.T.);
#32787=ADVANCED_FACE('',(#3813),#1974,.T.);
#32788=ADVANCED_FACE('',(#3814),#1975,.T.);
#32789=ADVANCED_FACE('',(#3815),#1976,.T.);
#32790=ADVANCED_FACE('',(#3816),#1977,.T.);
#32791=ADVANCED_FACE('',(#3817),#1978,.T.);
#32792=ADVANCED_FACE('',(#3818),#1979,.T.);
#32793=ADVANCED_FACE('',(#3819),#1980,.T.);
#32794=ADVANCED_FACE('',(#3820),#1981,.T.);
#32795=ADVANCED_FACE('',(#3821),#1982,.T.);
#32796=ADVANCED_FACE('',(#3822),#1983,.T.);
#32797=ADVANCED_FACE('',(#3823),#1984,.F.);
#32798=ADVANCED_FACE('',(#3824),#1985,.T.);
#32799=ADVANCED_FACE('',(#3825),#1986,.T.);
#32800=ADVANCED_FACE('',(#3826),#1987,.T.);
#32801=ADVANCED_FACE('',(#3827),#1988,.T.);
#32802=ADVANCED_FACE('',(#3828),#1989,.T.);
#32803=ADVANCED_FACE('',(#3829),#1990,.T.);
#32804=ADVANCED_FACE('',(#3830),#1991,.T.);
#32805=ADVANCED_FACE('',(#3831),#1992,.T.);
#32806=ADVANCED_FACE('',(#3832),#1993,.T.);
#32807=ADVANCED_FACE('',(#3833),#1994,.T.);
#32808=ADVANCED_FACE('',(#3834),#1995,.T.);
#32809=ADVANCED_FACE('',(#3835),#1996,.T.);
#32810=ADVANCED_FACE('',(#3836),#1997,.T.);
#32811=ADVANCED_FACE('',(#3837),#1998,.T.);
#32812=ADVANCED_FACE('',(#3838),#1999,.T.);
#32813=ADVANCED_FACE('',(#3839),#2000,.T.);
#32814=ADVANCED_FACE('',(#3840),#2001,.T.);
#32815=ADVANCED_FACE('',(#3841),#2002,.T.);
#32816=ADVANCED_FACE('',(#3842),#2003,.T.);
#32817=ADVANCED_FACE('',(#3843),#2004,.T.);
#32818=ADVANCED_FACE('',(#3844),#2005,.T.);
#32819=ADVANCED_FACE('',(#3845),#2006,.T.);
#32820=ADVANCED_FACE('',(#3846),#2007,.T.);
#32821=ADVANCED_FACE('',(#3847),#2008,.T.);
#32822=ADVANCED_FACE('',(#3848),#2009,.T.);
#32823=ADVANCED_FACE('',(#3849),#2010,.T.);
#32824=ADVANCED_FACE('',(#3850),#2011,.T.);
#32825=ADVANCED_FACE('',(#3851),#2012,.T.);
#32826=ADVANCED_FACE('',(#3852),#2013,.F.);
#32827=ADVANCED_FACE('',(#3853),#2014,.T.);
#32828=ADVANCED_FACE('',(#3854),#2015,.T.);
#32829=ADVANCED_FACE('',(#3855),#2016,.T.);
#32830=ADVANCED_FACE('',(#3856),#2017,.T.);
#32831=ADVANCED_FACE('',(#3857),#2018,.T.);
#32832=ADVANCED_FACE('',(#3858),#2019,.T.);
#32833=ADVANCED_FACE('',(#3859),#2020,.T.);
#32834=ADVANCED_FACE('',(#3860),#2021,.T.);
#32835=ADVANCED_FACE('',(#3861),#2022,.T.);
#32836=ADVANCED_FACE('',(#3862),#2023,.T.);
#32837=ADVANCED_FACE('',(#3863),#2024,.T.);
#32838=ADVANCED_FACE('',(#3864),#2025,.T.);
#32839=ADVANCED_FACE('',(#3865),#2026,.T.);
#32840=ADVANCED_FACE('',(#3866),#2027,.T.);
#32841=ADVANCED_FACE('',(#3867),#2028,.T.);
#32842=ADVANCED_FACE('',(#3868),#2029,.T.);
#32843=ADVANCED_FACE('',(#3869),#2030,.T.);
#32844=ADVANCED_FACE('',(#3870),#2031,.T.);
#32845=ADVANCED_FACE('',(#3871),#2032,.T.);
#32846=ADVANCED_FACE('',(#3872),#2033,.T.);
#32847=ADVANCED_FACE('',(#3873),#2034,.T.);
#32848=ADVANCED_FACE('',(#3874),#2035,.T.);
#32849=ADVANCED_FACE('',(#3875),#2036,.T.);
#32850=ADVANCED_FACE('',(#3876),#2037,.T.);
#32851=ADVANCED_FACE('',(#3877),#2038,.T.);
#32852=ADVANCED_FACE('',(#3878),#2039,.T.);
#32853=ADVANCED_FACE('',(#3879),#2040,.T.);
#32854=ADVANCED_FACE('',(#3880),#2041,.F.);
#32855=ADVANCED_FACE('',(#3881),#2042,.T.);
#32856=ADVANCED_FACE('',(#3882),#2043,.T.);
#32857=ADVANCED_FACE('',(#3883),#2044,.T.);
#32858=ADVANCED_FACE('',(#3884),#2045,.T.);
#32859=ADVANCED_FACE('',(#3885),#2046,.T.);
#32860=ADVANCED_FACE('',(#3886),#2047,.T.);
#32861=ADVANCED_FACE('',(#3887),#2048,.T.);
#32862=ADVANCED_FACE('',(#3888),#2049,.T.);
#32863=ADVANCED_FACE('',(#3889),#2050,.T.);
#32864=ADVANCED_FACE('',(#3890),#2051,.T.);
#32865=ADVANCED_FACE('',(#3891),#2052,.T.);
#32866=ADVANCED_FACE('',(#3892),#2053,.T.);
#32867=ADVANCED_FACE('',(#3893),#2054,.T.);
#32868=ADVANCED_FACE('',(#3894),#2055,.T.);
#32869=ADVANCED_FACE('',(#3895),#2056,.F.);
#32870=ADVANCED_FACE('',(#3896),#2057,.T.);
#32871=ADVANCED_FACE('',(#3897),#2058,.T.);
#32872=ADVANCED_FACE('',(#3898),#2059,.T.);
#32873=ADVANCED_FACE('',(#3899),#2060,.T.);
#32874=ADVANCED_FACE('',(#3900),#2061,.T.);
#32875=ADVANCED_FACE('',(#3901),#2062,.T.);
#32876=ADVANCED_FACE('',(#3902),#2063,.T.);
#32877=ADVANCED_FACE('',(#3903),#2064,.T.);
#32878=ADVANCED_FACE('',(#3904),#2065,.T.);
#32879=ADVANCED_FACE('',(#3905),#2066,.T.);
#32880=ADVANCED_FACE('',(#3906),#2067,.T.);
#32881=ADVANCED_FACE('',(#3907),#2068,.T.);
#32882=ADVANCED_FACE('',(#3908),#2069,.T.);
#32883=ADVANCED_FACE('',(#3909),#2070,.T.);
#32884=ADVANCED_FACE('',(#3910),#2071,.T.);
#32885=ADVANCED_FACE('',(#3911),#2072,.T.);
#32886=ADVANCED_FACE('',(#3912),#2073,.T.);
#32887=ADVANCED_FACE('',(#3913),#2074,.T.);
#32888=ADVANCED_FACE('',(#3914),#2075,.T.);
#32889=ADVANCED_FACE('',(#3915),#2076,.T.);
#32890=ADVANCED_FACE('',(#3916),#2077,.T.);
#32891=ADVANCED_FACE('',(#3917),#2078,.T.);
#32892=ADVANCED_FACE('',(#3918),#2079,.T.);
#32893=ADVANCED_FACE('',(#3919),#2080,.T.);
#32894=ADVANCED_FACE('',(#3920),#2081,.T.);
#32895=ADVANCED_FACE('',(#3921),#2082,.T.);
#32896=ADVANCED_FACE('',(#3922),#2083,.T.);
#32897=ADVANCED_FACE('',(#3923),#2084,.T.);
#32898=ADVANCED_FACE('',(#3924),#2085,.F.);
#32899=ADVANCED_FACE('',(#3925),#2086,.T.);
#32900=ADVANCED_FACE('',(#3926),#2087,.T.);
#32901=ADVANCED_FACE('',(#3927),#2088,.T.);
#32902=ADVANCED_FACE('',(#3928),#2089,.T.);
#32903=ADVANCED_FACE('',(#3929),#2090,.T.);
#32904=ADVANCED_FACE('',(#3930),#2091,.T.);
#32905=ADVANCED_FACE('',(#3931),#2092,.T.);
#32906=ADVANCED_FACE('',(#3932),#2093,.T.);
#32907=ADVANCED_FACE('',(#3933),#2094,.T.);
#32908=ADVANCED_FACE('',(#3934),#2095,.T.);
#32909=ADVANCED_FACE('',(#3935),#2096,.T.);
#32910=ADVANCED_FACE('',(#3936),#2097,.T.);
#32911=ADVANCED_FACE('',(#3937),#2098,.T.);
#32912=ADVANCED_FACE('',(#3938),#2099,.T.);
#32913=ADVANCED_FACE('',(#3939),#2100,.T.);
#32914=ADVANCED_FACE('',(#3940),#2101,.T.);
#32915=ADVANCED_FACE('',(#3941),#2102,.T.);
#32916=ADVANCED_FACE('',(#3942),#2103,.T.);
#32917=ADVANCED_FACE('',(#3943),#2104,.T.);
#32918=ADVANCED_FACE('',(#3944),#2105,.T.);
#32919=ADVANCED_FACE('',(#3945),#2106,.T.);
#32920=ADVANCED_FACE('',(#3946),#2107,.T.);
#32921=ADVANCED_FACE('',(#3947),#2108,.T.);
#32922=ADVANCED_FACE('',(#3948),#2109,.T.);
#32923=ADVANCED_FACE('',(#3949),#2110,.T.);
#32924=ADVANCED_FACE('',(#3950),#2111,.T.);
#32925=ADVANCED_FACE('',(#3951),#2112,.T.);
#32926=ADVANCED_FACE('',(#3952),#2113,.F.);
#32927=ADVANCED_FACE('',(#3953),#2114,.T.);
#32928=ADVANCED_FACE('',(#3954),#2115,.T.);
#32929=ADVANCED_FACE('',(#3955),#2116,.T.);
#32930=ADVANCED_FACE('',(#3956),#2117,.T.);
#32931=ADVANCED_FACE('',(#3957),#2118,.T.);
#32932=ADVANCED_FACE('',(#3958),#2119,.T.);
#32933=ADVANCED_FACE('',(#3959),#2120,.T.);
#32934=ADVANCED_FACE('',(#3960),#2121,.T.);
#32935=ADVANCED_FACE('',(#3961),#2122,.T.);
#32936=ADVANCED_FACE('',(#3962),#2123,.T.);
#32937=ADVANCED_FACE('',(#3963),#2124,.T.);
#32938=ADVANCED_FACE('',(#3964),#2125,.T.);
#32939=ADVANCED_FACE('',(#3965),#2126,.T.);
#32940=ADVANCED_FACE('',(#3966),#2127,.T.);
#32941=ADVANCED_FACE('',(#3967),#2128,.F.);
#32942=ADVANCED_FACE('',(#3968),#2129,.T.);
#32943=ADVANCED_FACE('',(#3969),#2130,.T.);
#32944=ADVANCED_FACE('',(#3970),#2131,.T.);
#32945=ADVANCED_FACE('',(#3971),#2132,.T.);
#32946=ADVANCED_FACE('',(#3972),#2133,.T.);
#32947=ADVANCED_FACE('',(#3973),#2134,.T.);
#32948=ADVANCED_FACE('',(#3974),#2135,.T.);
#32949=ADVANCED_FACE('',(#3975),#2136,.T.);
#32950=ADVANCED_FACE('',(#3976),#2137,.T.);
#32951=ADVANCED_FACE('',(#3977),#2138,.T.);
#32952=ADVANCED_FACE('',(#3978),#2139,.T.);
#32953=ADVANCED_FACE('',(#3979),#2140,.T.);
#32954=ADVANCED_FACE('',(#3980),#2141,.T.);
#32955=ADVANCED_FACE('',(#3981),#2142,.T.);
#32956=ADVANCED_FACE('',(#3982),#2143,.T.);
#32957=ADVANCED_FACE('',(#3983),#2144,.T.);
#32958=ADVANCED_FACE('',(#3984),#2145,.T.);
#32959=ADVANCED_FACE('',(#3985),#2146,.T.);
#32960=ADVANCED_FACE('',(#3986),#2147,.T.);
#32961=ADVANCED_FACE('',(#3987),#2148,.T.);
#32962=ADVANCED_FACE('',(#3988),#2149,.T.);
#32963=ADVANCED_FACE('',(#3989),#2150,.T.);
#32964=ADVANCED_FACE('',(#3990),#2151,.T.);
#32965=ADVANCED_FACE('',(#3991),#2152,.T.);
#32966=ADVANCED_FACE('',(#3992),#2153,.T.);
#32967=ADVANCED_FACE('',(#3993),#2154,.T.);
#32968=ADVANCED_FACE('',(#3994),#2155,.T.);
#32969=ADVANCED_FACE('',(#3995),#2156,.T.);
#32970=ADVANCED_FACE('',(#3996),#2157,.F.);
#32971=ADVANCED_FACE('',(#3997),#2158,.T.);
#32972=ADVANCED_FACE('',(#3998),#2159,.T.);
#32973=ADVANCED_FACE('',(#3999),#2160,.T.);
#32974=ADVANCED_FACE('',(#4000),#2161,.T.);
#32975=ADVANCED_FACE('',(#4001),#2162,.T.);
#32976=ADVANCED_FACE('',(#4002),#2163,.T.);
#32977=ADVANCED_FACE('',(#4003),#2164,.T.);
#32978=ADVANCED_FACE('',(#4004),#2165,.T.);
#32979=ADVANCED_FACE('',(#4005),#2166,.T.);
#32980=ADVANCED_FACE('',(#4006),#2167,.T.);
#32981=ADVANCED_FACE('',(#4007),#2168,.T.);
#32982=ADVANCED_FACE('',(#4008),#2169,.T.);
#32983=ADVANCED_FACE('',(#4009),#2170,.T.);
#32984=ADVANCED_FACE('',(#4010),#2171,.T.);
#32985=ADVANCED_FACE('',(#4011),#2172,.T.);
#32986=ADVANCED_FACE('',(#4012),#2173,.T.);
#32987=ADVANCED_FACE('',(#4013),#2174,.T.);
#32988=ADVANCED_FACE('',(#4014),#2175,.T.);
#32989=ADVANCED_FACE('',(#4015),#2176,.T.);
#32990=ADVANCED_FACE('',(#4016),#2177,.T.);
#32991=ADVANCED_FACE('',(#4017),#2178,.T.);
#32992=ADVANCED_FACE('',(#4018),#2179,.T.);
#32993=ADVANCED_FACE('',(#4019),#2180,.T.);
#32994=ADVANCED_FACE('',(#4020),#2181,.T.);
#32995=ADVANCED_FACE('',(#4021),#2182,.T.);
#32996=ADVANCED_FACE('',(#4022),#2183,.T.);
#32997=ADVANCED_FACE('',(#4023),#2184,.T.);
#32998=ADVANCED_FACE('',(#4024),#2185,.F.);
#32999=ADVANCED_FACE('',(#4025),#2186,.T.);
#33000=ADVANCED_FACE('',(#4026),#2187,.T.);
#33001=ADVANCED_FACE('',(#4027),#2188,.T.);
#33002=ADVANCED_FACE('',(#4028),#2189,.T.);
#33003=ADVANCED_FACE('',(#4029),#2190,.T.);
#33004=ADVANCED_FACE('',(#4030),#2191,.T.);
#33005=ADVANCED_FACE('',(#4031),#2192,.T.);
#33006=ADVANCED_FACE('',(#4032),#2193,.T.);
#33007=ADVANCED_FACE('',(#4033),#2194,.T.);
#33008=ADVANCED_FACE('',(#4034),#2195,.T.);
#33009=ADVANCED_FACE('',(#4035),#2196,.T.);
#33010=ADVANCED_FACE('',(#4036),#2197,.T.);
#33011=ADVANCED_FACE('',(#4037),#2198,.T.);
#33012=ADVANCED_FACE('',(#4038),#2199,.T.);
#33013=ADVANCED_FACE('',(#4039),#2200,.F.);
#33014=ADVANCED_FACE('',(#4040),#2201,.T.);
#33015=ADVANCED_FACE('',(#4041),#2202,.T.);
#33016=ADVANCED_FACE('',(#4042),#2203,.T.);
#33017=ADVANCED_FACE('',(#4043),#2204,.T.);
#33018=ADVANCED_FACE('',(#4044),#2205,.T.);
#33019=ADVANCED_FACE('',(#4045),#2206,.T.);
#33020=ADVANCED_FACE('',(#4046),#2207,.T.);
#33021=ADVANCED_FACE('',(#4047),#2208,.T.);
#33022=ADVANCED_FACE('',(#4048),#2209,.T.);
#33023=ADVANCED_FACE('',(#4049),#2210,.T.);
#33024=ADVANCED_FACE('',(#4050),#2211,.T.);
#33025=ADVANCED_FACE('',(#4051),#2212,.T.);
#33026=ADVANCED_FACE('',(#4052),#2213,.T.);
#33027=ADVANCED_FACE('',(#4053),#2214,.T.);
#33028=ADVANCED_FACE('',(#4054),#2215,.T.);
#33029=ADVANCED_FACE('',(#4055),#2216,.T.);
#33030=ADVANCED_FACE('',(#4056),#2217,.T.);
#33031=ADVANCED_FACE('',(#4057),#2218,.T.);
#33032=ADVANCED_FACE('',(#4058),#2219,.T.);
#33033=ADVANCED_FACE('',(#4059),#2220,.T.);
#33034=ADVANCED_FACE('',(#4060),#2221,.T.);
#33035=ADVANCED_FACE('',(#4061),#2222,.T.);
#33036=ADVANCED_FACE('',(#4062),#2223,.T.);
#33037=ADVANCED_FACE('',(#4063),#2224,.T.);
#33038=ADVANCED_FACE('',(#4064),#2225,.T.);
#33039=ADVANCED_FACE('',(#4065),#2226,.T.);
#33040=ADVANCED_FACE('',(#4066),#2227,.T.);
#33041=ADVANCED_FACE('',(#4067),#2228,.T.);
#33042=ADVANCED_FACE('',(#4068),#2229,.F.);
#33043=ADVANCED_FACE('',(#4069),#2230,.T.);
#33044=ADVANCED_FACE('',(#4070),#2231,.T.);
#33045=ADVANCED_FACE('',(#4071),#2232,.T.);
#33046=ADVANCED_FACE('',(#4072),#2233,.T.);
#33047=ADVANCED_FACE('',(#4073),#2234,.T.);
#33048=ADVANCED_FACE('',(#4074),#2235,.T.);
#33049=ADVANCED_FACE('',(#4075),#2236,.T.);
#33050=ADVANCED_FACE('',(#4076),#2237,.T.);
#33051=ADVANCED_FACE('',(#4077),#2238,.T.);
#33052=ADVANCED_FACE('',(#4078),#2239,.T.);
#33053=ADVANCED_FACE('',(#4079),#2240,.T.);
#33054=ADVANCED_FACE('',(#4080),#2241,.T.);
#33055=ADVANCED_FACE('',(#4081),#2242,.T.);
#33056=ADVANCED_FACE('',(#4082),#2243,.T.);
#33057=ADVANCED_FACE('',(#4083),#2244,.T.);
#33058=ADVANCED_FACE('',(#4084),#2245,.T.);
#33059=ADVANCED_FACE('',(#4085),#2246,.T.);
#33060=ADVANCED_FACE('',(#4086),#2247,.T.);
#33061=ADVANCED_FACE('',(#4087),#2248,.T.);
#33062=ADVANCED_FACE('',(#4088),#2249,.T.);
#33063=ADVANCED_FACE('',(#4089),#2250,.T.);
#33064=ADVANCED_FACE('',(#4090),#2251,.T.);
#33065=ADVANCED_FACE('',(#4091),#2252,.T.);
#33066=ADVANCED_FACE('',(#4092),#2253,.T.);
#33067=ADVANCED_FACE('',(#4093),#2254,.T.);
#33068=ADVANCED_FACE('',(#4094),#2255,.T.);
#33069=ADVANCED_FACE('',(#4095),#2256,.T.);
#33070=ADVANCED_FACE('',(#4096),#2257,.F.);
#33071=ADVANCED_FACE('',(#4097),#2258,.T.);
#33072=ADVANCED_FACE('',(#4098),#2259,.T.);
#33073=ADVANCED_FACE('',(#4099),#2260,.T.);
#33074=ADVANCED_FACE('',(#4100),#2261,.T.);
#33075=ADVANCED_FACE('',(#4101),#2262,.T.);
#33076=ADVANCED_FACE('',(#4102),#2263,.T.);
#33077=ADVANCED_FACE('',(#4103),#2264,.T.);
#33078=ADVANCED_FACE('',(#4104),#2265,.T.);
#33079=ADVANCED_FACE('',(#4105),#2266,.T.);
#33080=ADVANCED_FACE('',(#4106),#2267,.T.);
#33081=ADVANCED_FACE('',(#4107),#2268,.T.);
#33082=ADVANCED_FACE('',(#4108),#2269,.T.);
#33083=ADVANCED_FACE('',(#4109),#2270,.T.);
#33084=ADVANCED_FACE('',(#4110),#2271,.T.);
#33085=ADVANCED_FACE('',(#4111),#2272,.F.);
#33086=ADVANCED_FACE('',(#4112),#2273,.T.);
#33087=ADVANCED_FACE('',(#4113),#2274,.T.);
#33088=ADVANCED_FACE('',(#4114),#2275,.T.);
#33089=ADVANCED_FACE('',(#4115),#2276,.T.);
#33090=ADVANCED_FACE('',(#4116),#2277,.T.);
#33091=ADVANCED_FACE('',(#4117),#2278,.T.);
#33092=ADVANCED_FACE('',(#4118),#2279,.T.);
#33093=ADVANCED_FACE('',(#4119),#2280,.T.);
#33094=ADVANCED_FACE('',(#4120),#2281,.T.);
#33095=ADVANCED_FACE('',(#4121),#2282,.T.);
#33096=ADVANCED_FACE('',(#4122),#2283,.T.);
#33097=ADVANCED_FACE('',(#4123),#2284,.T.);
#33098=ADVANCED_FACE('',(#4124),#2285,.T.);
#33099=ADVANCED_FACE('',(#4125),#2286,.T.);
#33100=ADVANCED_FACE('',(#4126),#2287,.T.);
#33101=ADVANCED_FACE('',(#4127),#2288,.T.);
#33102=ADVANCED_FACE('',(#4128),#2289,.T.);
#33103=ADVANCED_FACE('',(#4129),#2290,.T.);
#33104=ADVANCED_FACE('',(#4130),#2291,.T.);
#33105=ADVANCED_FACE('',(#4131),#2292,.T.);
#33106=ADVANCED_FACE('',(#4132),#2293,.T.);
#33107=ADVANCED_FACE('',(#4133),#2294,.T.);
#33108=ADVANCED_FACE('',(#4134),#2295,.T.);
#33109=ADVANCED_FACE('',(#4135),#2296,.T.);
#33110=ADVANCED_FACE('',(#4136),#2297,.T.);
#33111=ADVANCED_FACE('',(#4137),#2298,.T.);
#33112=ADVANCED_FACE('',(#4138),#2299,.T.);
#33113=ADVANCED_FACE('',(#4139),#2300,.T.);
#33114=ADVANCED_FACE('',(#4140),#2301,.F.);
#33115=ADVANCED_FACE('',(#4141),#2302,.T.);
#33116=ADVANCED_FACE('',(#4142),#2303,.T.);
#33117=ADVANCED_FACE('',(#4143),#2304,.T.);
#33118=ADVANCED_FACE('',(#4144),#2305,.T.);
#33119=ADVANCED_FACE('',(#4145),#2306,.T.);
#33120=ADVANCED_FACE('',(#4146),#2307,.T.);
#33121=ADVANCED_FACE('',(#4147),#2308,.T.);
#33122=ADVANCED_FACE('',(#4148),#2309,.T.);
#33123=ADVANCED_FACE('',(#4149),#2310,.T.);
#33124=ADVANCED_FACE('',(#4150),#2311,.T.);
#33125=ADVANCED_FACE('',(#4151),#2312,.T.);
#33126=ADVANCED_FACE('',(#4152),#2313,.T.);
#33127=ADVANCED_FACE('',(#4153),#2314,.T.);
#33128=ADVANCED_FACE('',(#4154),#2315,.T.);
#33129=ADVANCED_FACE('',(#4155),#2316,.T.);
#33130=ADVANCED_FACE('',(#4156),#2317,.T.);
#33131=ADVANCED_FACE('',(#4157),#2318,.T.);
#33132=ADVANCED_FACE('',(#4158),#2319,.T.);
#33133=ADVANCED_FACE('',(#4159),#2320,.T.);
#33134=ADVANCED_FACE('',(#4160),#2321,.T.);
#33135=ADVANCED_FACE('',(#4161),#2322,.T.);
#33136=ADVANCED_FACE('',(#4162),#2323,.T.);
#33137=ADVANCED_FACE('',(#4163),#2324,.T.);
#33138=ADVANCED_FACE('',(#4164),#2325,.T.);
#33139=ADVANCED_FACE('',(#4165),#2326,.T.);
#33140=ADVANCED_FACE('',(#4166),#2327,.T.);
#33141=ADVANCED_FACE('',(#4167),#2328,.T.);
#33142=ADVANCED_FACE('',(#4168),#2329,.F.);
#33143=ADVANCED_FACE('',(#4169),#2330,.T.);
#33144=ADVANCED_FACE('',(#4170),#2331,.T.);
#33145=ADVANCED_FACE('',(#4171),#2332,.T.);
#33146=ADVANCED_FACE('',(#4172),#2333,.T.);
#33147=ADVANCED_FACE('',(#4173),#2334,.T.);
#33148=ADVANCED_FACE('',(#4174),#2335,.T.);
#33149=ADVANCED_FACE('',(#4175),#2336,.T.);
#33150=ADVANCED_FACE('',(#4176),#2337,.T.);
#33151=ADVANCED_FACE('',(#4177),#2338,.T.);
#33152=ADVANCED_FACE('',(#4178),#2339,.T.);
#33153=ADVANCED_FACE('',(#4179),#2340,.T.);
#33154=ADVANCED_FACE('',(#4180),#2341,.T.);
#33155=ADVANCED_FACE('',(#4181),#2342,.T.);
#33156=ADVANCED_FACE('',(#4182),#2343,.T.);
#33157=ADVANCED_FACE('',(#4183),#2344,.F.);
#33158=ADVANCED_FACE('',(#4184),#2345,.T.);
#33159=ADVANCED_FACE('',(#4185),#2346,.T.);
#33160=ADVANCED_FACE('',(#4186),#31954,.F.);
#33161=ADVANCED_FACE('',(#4187),#31955,.F.);
#33162=ADVANCED_FACE('',(#4188),#3001,.F.);
#33163=ADVANCED_FACE('',(#4189),#2347,.T.);
#33164=ADVANCED_FACE('',(#4190),#2348,.T.);
#33165=ADVANCED_FACE('',(#4191),#2349,.T.);
#33166=ADVANCED_FACE('',(#4192),#2350,.T.);
#33167=ADVANCED_FACE('',(#4193),#2351,.T.);
#33168=ADVANCED_FACE('',(#4194),#2352,.T.);
#33169=ADVANCED_FACE('',(#4195),#2353,.T.);
#33170=ADVANCED_FACE('',(#4196),#2354,.T.);
#33171=ADVANCED_FACE('',(#4197),#2355,.T.);
#33172=ADVANCED_FACE('',(#4198),#2356,.T.);
#33173=ADVANCED_FACE('',(#4199),#2357,.T.);
#33174=ADVANCED_FACE('',(#4200),#2358,.T.);
#33175=ADVANCED_FACE('',(#4201),#2359,.F.);
#33176=ADVANCED_FACE('',(#4202),#2360,.T.);
#33177=ADVANCED_FACE('',(#4203),#2361,.T.);
#33178=ADVANCED_FACE('',(#4204),#2362,.T.);
#33179=ADVANCED_FACE('',(#4205),#2363,.T.);
#33180=ADVANCED_FACE('',(#4206),#2364,.T.);
#33181=ADVANCED_FACE('',(#4207),#2365,.T.);
#33182=ADVANCED_FACE('',(#4208),#2366,.T.);
#33183=ADVANCED_FACE('',(#4209),#2367,.T.);
#33184=ADVANCED_FACE('',(#4210),#2368,.T.);
#33185=ADVANCED_FACE('',(#4211),#2369,.T.);
#33186=ADVANCED_FACE('',(#4212),#2370,.T.);
#33187=ADVANCED_FACE('',(#4213),#2371,.T.);
#33188=ADVANCED_FACE('',(#4214),#2372,.T.);
#33189=ADVANCED_FACE('',(#4215),#2373,.T.);
#33190=ADVANCED_FACE('',(#4216),#2374,.F.);
#33191=ADVANCED_FACE('',(#4217),#2375,.T.);
#33192=ADVANCED_FACE('',(#4218),#2376,.T.);
#33193=ADVANCED_FACE('',(#4219),#31956,.T.);
#33194=ADVANCED_FACE('',(#4220),#3002,.T.);
#33195=ADVANCED_FACE('',(#4221),#31957,.T.);
#33196=ADVANCED_FACE('',(#4222),#31958,.F.);
#33197=ADVANCED_FACE('',(#4223,#1210),#2377,.T.);
#33198=ADVANCED_FACE('',(#4224),#31959,.T.);
#33199=ADVANCED_FACE('',(#4225),#31960,.T.);
#33200=ADVANCED_FACE('',(#4226),#31961,.T.);
#33201=ADVANCED_FACE('',(#4227),#2378,.T.);
#33202=ADVANCED_FACE('',(#4228),#2379,.T.);
#33203=ADVANCED_FACE('',(#4229),#2380,.T.);
#33204=ADVANCED_FACE('',(#4230),#2381,.T.);
#33205=ADVANCED_FACE('',(#4231),#2382,.T.);
#33206=ADVANCED_FACE('',(#4232),#2383,.T.);
#33207=ADVANCED_FACE('',(#4233),#2384,.T.);
#33208=ADVANCED_FACE('',(#4234),#2385,.T.);
#33209=ADVANCED_FACE('',(#4235),#2386,.F.);
#33210=ADVANCED_FACE('',(#4236),#2387,.T.);
#33211=ADVANCED_FACE('',(#4237),#2388,.T.);
#33212=ADVANCED_FACE('',(#4238),#2389,.T.);
#33213=ADVANCED_FACE('',(#4239),#2390,.F.);
#33214=ADVANCED_FACE('',(#4240),#2391,.T.);
#33215=ADVANCED_FACE('',(#4241),#2392,.T.);
#33216=ADVANCED_FACE('',(#4242),#2393,.T.);
#33217=ADVANCED_FACE('',(#4243),#2394,.T.);
#33218=ADVANCED_FACE('',(#4244),#2395,.T.);
#33219=ADVANCED_FACE('',(#4245),#2396,.F.);
#33220=ADVANCED_FACE('',(#4246),#2397,.T.);
#33221=ADVANCED_FACE('',(#4247),#2398,.T.);
#33222=ADVANCED_FACE('',(#4248),#2399,.T.);
#33223=ADVANCED_FACE('',(#4249),#2400,.F.);
#33224=ADVANCED_FACE('',(#4250),#2401,.T.);
#33225=ADVANCED_FACE('',(#4251),#2402,.T.);
#33226=ADVANCED_FACE('',(#4252),#2403,.T.);
#33227=ADVANCED_FACE('',(#4253),#2404,.T.);
#33228=ADVANCED_FACE('',(#4254),#2405,.T.);
#33229=ADVANCED_FACE('',(#4255),#2406,.F.);
#33230=ADVANCED_FACE('',(#4256),#2407,.T.);
#33231=ADVANCED_FACE('',(#4257),#2408,.T.);
#33232=ADVANCED_FACE('',(#4258),#2409,.T.);
#33233=ADVANCED_FACE('',(#4259),#2410,.F.);
#33234=ADVANCED_FACE('',(#4260),#2411,.T.);
#33235=ADVANCED_FACE('',(#4261),#2412,.T.);
#33236=ADVANCED_FACE('',(#4262),#2413,.T.);
#33237=ADVANCED_FACE('',(#4263),#2414,.T.);
#33238=ADVANCED_FACE('',(#4264),#2415,.T.);
#33239=ADVANCED_FACE('',(#4265),#2416,.F.);
#33240=ADVANCED_FACE('',(#4266),#2417,.T.);
#33241=ADVANCED_FACE('',(#4267),#2418,.T.);
#33242=ADVANCED_FACE('',(#4268),#2419,.T.);
#33243=ADVANCED_FACE('',(#4269),#2420,.F.);
#33244=ADVANCED_FACE('',(#4270),#2421,.T.);
#33245=ADVANCED_FACE('',(#4271),#2422,.T.);
#33246=ADVANCED_FACE('',(#4272),#2423,.T.);
#33247=ADVANCED_FACE('',(#4273),#2424,.T.);
#33248=ADVANCED_FACE('',(#4274),#2425,.T.);
#33249=ADVANCED_FACE('',(#4275),#2426,.F.);
#33250=ADVANCED_FACE('',(#4276),#2427,.T.);
#33251=ADVANCED_FACE('',(#4277),#2428,.T.);
#33252=ADVANCED_FACE('',(#4278),#2429,.T.);
#33253=ADVANCED_FACE('',(#4279),#2430,.F.);
#33254=ADVANCED_FACE('',(#4280),#2431,.T.);
#33255=ADVANCED_FACE('',(#4281),#2432,.T.);
#33256=ADVANCED_FACE('',(#4282),#2433,.T.);
#33257=ADVANCED_FACE('',(#4283),#2434,.T.);
#33258=ADVANCED_FACE('',(#4284),#2435,.T.);
#33259=ADVANCED_FACE('',(#4285),#2436,.F.);
#33260=ADVANCED_FACE('',(#4286),#2437,.T.);
#33261=ADVANCED_FACE('',(#4287),#2438,.T.);
#33262=ADVANCED_FACE('',(#4288),#2439,.T.);
#33263=ADVANCED_FACE('',(#4289),#2440,.F.);
#33264=ADVANCED_FACE('',(#4290),#2441,.T.);
#33265=ADVANCED_FACE('',(#4291),#2442,.T.);
#33266=ADVANCED_FACE('',(#4292),#2443,.T.);
#33267=ADVANCED_FACE('',(#4293),#2444,.T.);
#33268=ADVANCED_FACE('',(#4294),#2445,.T.);
#33269=ADVANCED_FACE('',(#4295),#2446,.F.);
#33270=ADVANCED_FACE('',(#4296),#2447,.T.);
#33271=ADVANCED_FACE('',(#4297),#2448,.T.);
#33272=ADVANCED_FACE('',(#4298),#2449,.T.);
#33273=ADVANCED_FACE('',(#4299),#2450,.F.);
#33274=ADVANCED_FACE('',(#4300),#2451,.T.);
#33275=ADVANCED_FACE('',(#4301),#2452,.T.);
#33276=ADVANCED_FACE('',(#4302),#2453,.T.);
#33277=ADVANCED_FACE('',(#4303),#2454,.T.);
#33278=ADVANCED_FACE('',(#4304),#2455,.T.);
#33279=ADVANCED_FACE('',(#4305),#2456,.F.);
#33280=ADVANCED_FACE('',(#4306),#2457,.T.);
#33281=ADVANCED_FACE('',(#4307),#2458,.T.);
#33282=ADVANCED_FACE('',(#4308),#2459,.T.);
#33283=ADVANCED_FACE('',(#4309),#2460,.F.);
#33284=ADVANCED_FACE('',(#4310),#2461,.T.);
#33285=ADVANCED_FACE('',(#4311),#2462,.T.);
#33286=ADVANCED_FACE('',(#4312),#2463,.T.);
#33287=ADVANCED_FACE('',(#4313),#2464,.T.);
#33288=ADVANCED_FACE('',(#4314),#2465,.T.);
#33289=ADVANCED_FACE('',(#4315),#2466,.F.);
#33290=ADVANCED_FACE('',(#4316),#2467,.T.);
#33291=ADVANCED_FACE('',(#4317),#2468,.T.);
#33292=ADVANCED_FACE('',(#4318),#2469,.T.);
#33293=ADVANCED_FACE('',(#4319),#2470,.F.);
#33294=ADVANCED_FACE('',(#4320),#2471,.T.);
#33295=ADVANCED_FACE('',(#4321),#2472,.T.);
#33296=ADVANCED_FACE('',(#4322),#2473,.T.);
#33297=ADVANCED_FACE('',(#4323),#2474,.T.);
#33298=ADVANCED_FACE('',(#4324),#2475,.T.);
#33299=ADVANCED_FACE('',(#4325),#2476,.F.);
#33300=ADVANCED_FACE('',(#4326),#2477,.T.);
#33301=ADVANCED_FACE('',(#4327),#2478,.T.);
#33302=ADVANCED_FACE('',(#4328),#2479,.T.);
#33303=ADVANCED_FACE('',(#4329),#2480,.F.);
#33304=ADVANCED_FACE('',(#4330),#2481,.T.);
#33305=ADVANCED_FACE('',(#4331),#2482,.T.);
#33306=ADVANCED_FACE('',(#4332),#2483,.T.);
#33307=ADVANCED_FACE('',(#4333),#2484,.T.);
#33308=ADVANCED_FACE('',(#4334),#2485,.T.);
#33309=ADVANCED_FACE('',(#4335),#2486,.F.);
#33310=ADVANCED_FACE('',(#4336),#2487,.T.);
#33311=ADVANCED_FACE('',(#4337),#2488,.T.);
#33312=ADVANCED_FACE('',(#4338),#2489,.T.);
#33313=ADVANCED_FACE('',(#4339),#2490,.F.);
#33314=ADVANCED_FACE('',(#4340),#2491,.T.);
#33315=ADVANCED_FACE('',(#4341),#2492,.T.);
#33316=ADVANCED_FACE('',(#4342),#2493,.T.);
#33317=ADVANCED_FACE('',(#4343),#2494,.T.);
#33318=ADVANCED_FACE('',(#4344),#2495,.T.);
#33319=ADVANCED_FACE('',(#4345),#2496,.F.);
#33320=ADVANCED_FACE('',(#4346),#2497,.T.);
#33321=ADVANCED_FACE('',(#4347),#2498,.T.);
#33322=ADVANCED_FACE('',(#4348),#2499,.T.);
#33323=ADVANCED_FACE('',(#4349),#2500,.F.);
#33324=ADVANCED_FACE('',(#4350),#2501,.T.);
#33325=ADVANCED_FACE('',(#4351),#2502,.T.);
#33326=ADVANCED_FACE('',(#4352),#2503,.T.);
#33327=ADVANCED_FACE('',(#4353),#2504,.T.);
#33328=ADVANCED_FACE('',(#4354),#2505,.T.);
#33329=ADVANCED_FACE('',(#4355),#2506,.F.);
#33330=ADVANCED_FACE('',(#4356),#2507,.T.);
#33331=ADVANCED_FACE('',(#4357),#2508,.T.);
#33332=ADVANCED_FACE('',(#4358),#2509,.T.);
#33333=ADVANCED_FACE('',(#4359),#2510,.F.);
#33334=ADVANCED_FACE('',(#4360),#2511,.T.);
#33335=ADVANCED_FACE('',(#4361),#2512,.T.);
#33336=ADVANCED_FACE('',(#4362),#2513,.T.);
#33337=ADVANCED_FACE('',(#4363),#2514,.T.);
#33338=ADVANCED_FACE('',(#4364),#2515,.T.);
#33339=ADVANCED_FACE('',(#4365),#2516,.F.);
#33340=ADVANCED_FACE('',(#4366),#2517,.T.);
#33341=ADVANCED_FACE('',(#4367),#2518,.T.);
#33342=ADVANCED_FACE('',(#4368),#2519,.T.);
#33343=ADVANCED_FACE('',(#4369),#2520,.F.);
#33344=ADVANCED_FACE('',(#4370),#2521,.T.);
#33345=ADVANCED_FACE('',(#4371),#3003,.F.);
#33346=ADVANCED_FACE('',(#4372),#3004,.F.);
#33347=ADVANCED_FACE('',(#4373),#3005,.F.);
#33348=ADVANCED_FACE('',(#4374),#3006,.F.);
#33349=ADVANCED_FACE('',(#4375),#3007,.F.);
#33350=ADVANCED_FACE('',(#4376),#31962,.F.);
#33351=ADVANCED_FACE('',(#4377),#3008,.F.);
#33352=ADVANCED_FACE('',(#4378),#3009,.T.);
#33353=ADVANCED_FACE('',(#4379),#3010,.T.);
#33354=ADVANCED_FACE('',(#4380),#3011,.T.);
#33355=ADVANCED_FACE('',(#4381),#3012,.T.);
#33356=ADVANCED_FACE('',(#4382,#1211),#2522,.T.);
#33357=ADVANCED_FACE('',(#4383),#3013,.F.);
#33358=ADVANCED_FACE('',(#4384,#1212),#2523,.T.);
#33359=ADVANCED_FACE('',(#4385),#3014,.F.);
#33360=ADVANCED_FACE('',(#4386,#1213),#2524,.T.);
#33361=ADVANCED_FACE('',(#4387),#3015,.F.);
#33362=ADVANCED_FACE('',(#4388,#1214),#2525,.T.);
#33363=ADVANCED_FACE('',(#4389),#3016,.F.);
#33364=ADVANCED_FACE('',(#4390),#31963,.F.);
#33365=ADVANCED_FACE('',(#4391),#31964,.T.);
#33366=ADVANCED_FACE('',(#4392,#1215,#1216,#1217,#1218,#1219,#1220),#2526,
 .T.);
#33367=ADVANCED_FACE('',(#4393),#31965,.F.);
#33368=ADVANCED_FACE('',(#4394),#31966,.F.);
#33369=ADVANCED_FACE('',(#4395),#3017,.T.);
#33370=ADVANCED_FACE('',(#4396),#3018,.T.);
#33371=ADVANCED_FACE('',(#4397),#3019,.T.);
#33372=ADVANCED_FACE('',(#4398),#3020,.T.);
#33373=ADVANCED_FACE('',(#4399),#3021,.T.);
#33374=ADVANCED_FACE('',(#4400),#3022,.T.);
#33375=ADVANCED_FACE('',(#4401),#3023,.T.);
#33376=ADVANCED_FACE('',(#4402),#3024,.T.);
#33377=ADVANCED_FACE('',(#4403),#3025,.T.);
#33378=ADVANCED_FACE('',(#4404),#31967,.F.);
#33379=ADVANCED_FACE('',(#4405),#31968,.F.);
#33380=ADVANCED_FACE('',(#4406,#1221),#2527,.T.);
#33381=ADVANCED_FACE('',(#4407),#2528,.T.);
#33382=ADVANCED_FACE('',(#4408),#2529,.F.);
#33383=ADVANCED_FACE('',(#4409),#2530,.T.);
#33384=ADVANCED_FACE('',(#4410),#2531,.T.);
#33385=ADVANCED_FACE('',(#4411),#2532,.T.);
#33386=ADVANCED_FACE('',(#4412),#2533,.T.);
#33387=ADVANCED_FACE('',(#4413),#2534,.T.);
#33388=ADVANCED_FACE('',(#4414),#2535,.T.);
#33389=ADVANCED_FACE('',(#4415),#2536,.T.);
#33390=ADVANCED_FACE('',(#4416),#2537,.T.);
#33391=ADVANCED_FACE('',(#4417),#2538,.T.);
#33392=ADVANCED_FACE('',(#4418),#2539,.T.);
#33393=ADVANCED_FACE('',(#4419),#2540,.T.);
#33394=ADVANCED_FACE('',(#4420),#2541,.T.);
#33395=ADVANCED_FACE('',(#4421),#2542,.T.);
#33396=ADVANCED_FACE('',(#4422),#2543,.T.);
#33397=ADVANCED_FACE('',(#4423),#2544,.T.);
#33398=ADVANCED_FACE('',(#4424),#2545,.T.);
#33399=ADVANCED_FACE('',(#4425),#2546,.T.);
#33400=ADVANCED_FACE('',(#4426),#2547,.T.);
#33401=ADVANCED_FACE('',(#4427),#2548,.T.);
#33402=ADVANCED_FACE('',(#4428),#2549,.T.);
#33403=ADVANCED_FACE('',(#4429),#2550,.T.);
#33404=ADVANCED_FACE('',(#4430),#2551,.T.);
#33405=ADVANCED_FACE('',(#4431),#2552,.T.);
#33406=ADVANCED_FACE('',(#4432),#2553,.T.);
#33407=ADVANCED_FACE('',(#4433),#2554,.T.);
#33408=ADVANCED_FACE('',(#4434),#2555,.T.);
#33409=ADVANCED_FACE('',(#4435),#2556,.T.);
#33410=ADVANCED_FACE('',(#4436),#2557,.T.);
#33411=ADVANCED_FACE('',(#4437),#2558,.T.);
#33412=ADVANCED_FACE('',(#4438),#2559,.T.);
#33413=ADVANCED_FACE('',(#4439),#2560,.T.);
#33414=ADVANCED_FACE('',(#4440),#2561,.T.);
#33415=ADVANCED_FACE('',(#4441),#2562,.T.);
#33416=ADVANCED_FACE('',(#4442),#31969,.F.);
#33417=ADVANCED_FACE('',(#4443,#1222,#1223,#1224,#1225,#1226),#2563,.T.);
#33418=ADVANCED_FACE('',(#4444),#3026,.F.);
#33419=ADVANCED_FACE('',(#4445),#31970,.F.);
#33420=ADVANCED_FACE('',(#4446),#3027,.F.);
#33421=ADVANCED_FACE('',(#4447),#31971,.F.);
#33422=ADVANCED_FACE('',(#4448),#3028,.F.);
#33423=ADVANCED_FACE('',(#4449),#31972,.F.);
#33424=ADVANCED_FACE('',(#4450),#3029,.F.);
#33425=ADVANCED_FACE('',(#4451),#31973,.F.);
#33426=ADVANCED_FACE('',(#4452,#1227,#1228,#1229,#1230,#1231),#2564,.F.);
#33427=ADVANCED_FACE('',(#4453),#31974,.F.);
#33428=ADVANCED_FACE('',(#4454),#31975,.F.);
#33429=ADVANCED_FACE('',(#4455),#31976,.F.);
#33430=ADVANCED_FACE('',(#4456),#2565,.T.);
#33431=ADVANCED_FACE('',(#4457),#2566,.T.);
#33432=ADVANCED_FACE('',(#4458),#2567,.T.);
#33433=ADVANCED_FACE('',(#4459),#2568,.T.);
#33434=ADVANCED_FACE('',(#4460),#2569,.T.);
#33435=ADVANCED_FACE('',(#4461),#2570,.T.);
#33436=ADVANCED_FACE('',(#4462),#31977,.T.);
#33437=ADVANCED_FACE('',(#4463),#31978,.T.);
#33438=ADVANCED_FACE('',(#4464),#3030,.T.);
#33439=ADVANCED_FACE('',(#4465),#31979,.T.);
#33440=ADVANCED_FACE('',(#4466),#2571,.T.);
#33441=ADVANCED_FACE('',(#4467),#275,.F.);
#33442=ADVANCED_FACE('',(#4468),#276,.F.);
#33443=ADVANCED_FACE('',(#4469),#277,.F.);
#33444=ADVANCED_FACE('',(#4470),#278,.F.);
#33445=ADVANCED_FACE('',(#4471),#279,.F.);
#33446=ADVANCED_FACE('',(#4472),#280,.F.);
#33447=ADVANCED_FACE('',(#4473),#281,.F.);
#33448=ADVANCED_FACE('',(#4474),#282,.F.);
#33449=ADVANCED_FACE('',(#4475),#283,.F.);
#33450=ADVANCED_FACE('',(#4476),#284,.F.);
#33451=ADVANCED_FACE('',(#4477),#285,.F.);
#33452=ADVANCED_FACE('',(#4478),#3031,.T.);
#33453=ADVANCED_FACE('',(#4479),#3032,.T.);
#33454=ADVANCED_FACE('',(#4480),#3033,.T.);
#33455=ADVANCED_FACE('',(#4481),#3034,.T.);
#33456=ADVANCED_FACE('',(#4482),#3035,.T.);
#33457=ADVANCED_FACE('',(#4483),#2572,.F.);
#33458=ADVANCED_FACE('',(#4484),#2573,.T.);
#33459=ADVANCED_FACE('',(#4485),#286,.F.);
#33460=ADVANCED_FACE('',(#4486),#2574,.F.);
#33461=ADVANCED_FACE('',(#4487),#2575,.F.);
#33462=ADVANCED_FACE('',(#4488),#2576,.F.);
#33463=ADVANCED_FACE('',(#4489),#2577,.F.);
#33464=ADVANCED_FACE('',(#4490),#2578,.F.);
#33465=ADVANCED_FACE('',(#4491),#2579,.F.);
#33466=ADVANCED_FACE('',(#4492),#2580,.F.);
#33467=ADVANCED_FACE('',(#4493),#2581,.F.);
#33468=ADVANCED_FACE('',(#4494),#2582,.F.);
#33469=ADVANCED_FACE('',(#4495),#2583,.F.);
#33470=ADVANCED_FACE('',(#4496),#2584,.F.);
#33471=ADVANCED_FACE('',(#4497),#3036,.T.);
#33472=ADVANCED_FACE('',(#4498),#3037,.T.);
#33473=ADVANCED_FACE('',(#4499),#3038,.T.);
#33474=ADVANCED_FACE('',(#4500),#3039,.T.);
#33475=ADVANCED_FACE('',(#4501),#3040,.T.);
#33476=ADVANCED_FACE('',(#4502),#3041,.T.);
#33477=ADVANCED_FACE('',(#4503),#3042,.T.);
#33478=ADVANCED_FACE('',(#4504),#3043,.T.);
#33479=ADVANCED_FACE('',(#4505),#3044,.T.);
#33480=ADVANCED_FACE('',(#4506),#3045,.T.);
#33481=ADVANCED_FACE('',(#4507),#3046,.T.);
#33482=ADVANCED_FACE('',(#4508),#3047,.T.);
#33483=ADVANCED_FACE('',(#4509),#3048,.T.);
#33484=ADVANCED_FACE('',(#4510),#3049,.T.);
#33485=ADVANCED_FACE('',(#4511),#3050,.F.);
#33486=ADVANCED_FACE('',(#4512),#31980,.T.);
#33487=ADVANCED_FACE('',(#4513),#3051,.T.);
#33488=ADVANCED_FACE('',(#4514,#1232),#2585,.T.);
#33489=ADVANCED_FACE('',(#4515),#31981,.T.);
#33490=ADVANCED_FACE('',(#4516),#3052,.T.);
#33491=ADVANCED_FACE('',(#4517),#31982,.T.);
#33492=ADVANCED_FACE('',(#4518),#31983,.T.);
#33493=ADVANCED_FACE('',(#4519),#2586,.F.);
#33494=ADVANCED_FACE('',(#4520),#2587,.F.);
#33495=ADVANCED_FACE('',(#4521),#3053,.T.);
#33496=ADVANCED_FACE('',(#4522),#2588,.F.);
#33497=ADVANCED_FACE('',(#4523,#1233),#2589,.T.);
#33498=ADVANCED_FACE('',(#4524),#3054,.T.);
#33499=ADVANCED_FACE('',(#4525),#31984,.T.);
#33500=ADVANCED_FACE('',(#4526),#31985,.T.);
#33501=ADVANCED_FACE('',(#4527),#2590,.F.);
#33502=ADVANCED_FACE('',(#4528),#3055,.T.);
#33503=ADVANCED_FACE('',(#4529),#31986,.F.);
#33504=ADVANCED_FACE('',(#4530,#1234),#2591,.T.);
#33505=ADVANCED_FACE('',(#4531),#3056,.F.);
#33506=ADVANCED_FACE('',(#4532),#31987,.F.);
#33507=ADVANCED_FACE('',(#4533,#1235),#2592,.T.);
#33508=ADVANCED_FACE('',(#4534),#3057,.F.);
#33509=ADVANCED_FACE('',(#4535),#95,.F.);
#33510=ADVANCED_FACE('',(#4536,#1236),#2593,.T.);
#33511=ADVANCED_FACE('',(#4537),#31988,.T.);
#33512=ADVANCED_FACE('',(#4538),#3058,.T.);
#33513=ADVANCED_FACE('',(#4539),#31989,.T.);
#33514=ADVANCED_FACE('',(#4540),#31990,.F.);
#33515=ADVANCED_FACE('',(#4541),#31991,.F.);
#33516=ADVANCED_FACE('',(#4542),#3059,.F.);
#33517=ADVANCED_FACE('',(#4543),#31992,.F.);
#33518=ADVANCED_FACE('',(#4544,#1237),#2594,.T.);
#33519=ADVANCED_FACE('',(#4545),#31993,.T.);
#33520=ADVANCED_FACE('',(#4546),#3060,.T.);
#33521=ADVANCED_FACE('',(#4547),#31994,.T.);
#33522=ADVANCED_FACE('',(#4548,#1238),#2595,.T.);
#33523=ADVANCED_FACE('',(#4549),#31995,.F.);
#33524=ADVANCED_FACE('',(#4550),#31996,.F.);
#33525=ADVANCED_FACE('',(#4551),#31997,.F.);
#33526=ADVANCED_FACE('',(#4552,#1239),#2596,.T.);
#33527=ADVANCED_FACE('',(#4553),#31998,.T.);
#33528=ADVANCED_FACE('',(#4554,#1240),#2597,.T.);
#33529=ADVANCED_FACE('',(#4555),#3061,.T.);
#33530=ADVANCED_FACE('',(#4556),#31999,.T.);
#33531=ADVANCED_FACE('',(#4557),#3062,.T.);
#33532=ADVANCED_FACE('',(#4558,#1241),#2598,.T.);
#33533=ADVANCED_FACE('',(#4559),#96,.T.);
#33534=ADVANCED_FACE('',(#4560),#32000,.T.);
#33535=ADVANCED_FACE('',(#4561),#97,.T.);
#33536=ADVANCED_FACE('',(#4562),#2599,.T.);
#33537=ADVANCED_FACE('',(#4563),#2600,.T.);
#33538=ADVANCED_FACE('',(#4564),#98,.T.);
#33539=ADVANCED_FACE('',(#4565),#32001,.T.);
#33540=ADVANCED_FACE('',(#4566),#99,.T.);
#33541=ADVANCED_FACE('',(#4567),#2601,.T.);
#33542=ADVANCED_FACE('',(#4568),#2602,.T.);
#33543=ADVANCED_FACE('',(#4569),#100,.T.);
#33544=ADVANCED_FACE('',(#4570),#32002,.T.);
#33545=ADVANCED_FACE('',(#4571),#101,.T.);
#33546=ADVANCED_FACE('',(#4572),#2603,.T.);
#33547=ADVANCED_FACE('',(#4573),#2604,.T.);
#33548=ADVANCED_FACE('',(#4574),#102,.T.);
#33549=ADVANCED_FACE('',(#4575),#32003,.T.);
#33550=ADVANCED_FACE('',(#4576),#103,.T.);
#33551=ADVANCED_FACE('',(#4577),#2605,.T.);
#33552=ADVANCED_FACE('',(#4578),#2606,.T.);
#33553=ADVANCED_FACE('',(#4579),#104,.T.);
#33554=ADVANCED_FACE('',(#4580),#32004,.T.);
#33555=ADVANCED_FACE('',(#4581),#105,.T.);
#33556=ADVANCED_FACE('',(#4582),#2607,.T.);
#33557=ADVANCED_FACE('',(#4583),#2608,.T.);
#33558=ADVANCED_FACE('',(#4584),#106,.T.);
#33559=ADVANCED_FACE('',(#4585),#32005,.T.);
#33560=ADVANCED_FACE('',(#4586),#107,.T.);
#33561=ADVANCED_FACE('',(#4587),#2609,.T.);
#33562=ADVANCED_FACE('',(#4588),#2610,.T.);
#33563=ADVANCED_FACE('',(#4589),#108,.T.);
#33564=ADVANCED_FACE('',(#4590),#32006,.T.);
#33565=ADVANCED_FACE('',(#4591),#109,.T.);
#33566=ADVANCED_FACE('',(#4592),#2611,.T.);
#33567=ADVANCED_FACE('',(#4593),#2612,.T.);
#33568=ADVANCED_FACE('',(#4594),#110,.T.);
#33569=ADVANCED_FACE('',(#4595),#32007,.T.);
#33570=ADVANCED_FACE('',(#4596),#111,.T.);
#33571=ADVANCED_FACE('',(#4597),#2613,.T.);
#33572=ADVANCED_FACE('',(#4598),#2614,.T.);
#33573=ADVANCED_FACE('',(#4599),#112,.T.);
#33574=ADVANCED_FACE('',(#4600),#32008,.T.);
#33575=ADVANCED_FACE('',(#4601),#113,.T.);
#33576=ADVANCED_FACE('',(#4602),#2615,.T.);
#33577=ADVANCED_FACE('',(#4603),#2616,.T.);
#33578=ADVANCED_FACE('',(#4604),#114,.T.);
#33579=ADVANCED_FACE('',(#4605),#32009,.T.);
#33580=ADVANCED_FACE('',(#4606),#115,.T.);
#33581=ADVANCED_FACE('',(#4607),#2617,.T.);
#33582=ADVANCED_FACE('',(#4608),#2618,.T.);
#33583=ADVANCED_FACE('',(#4609),#116,.T.);
#33584=ADVANCED_FACE('',(#4610),#32010,.T.);
#33585=ADVANCED_FACE('',(#4611),#117,.T.);
#33586=ADVANCED_FACE('',(#4612),#2619,.T.);
#33587=ADVANCED_FACE('',(#4613),#2620,.T.);
#33588=ADVANCED_FACE('',(#4614),#118,.T.);
#33589=ADVANCED_FACE('',(#4615),#32011,.T.);
#33590=ADVANCED_FACE('',(#4616),#119,.T.);
#33591=ADVANCED_FACE('',(#4617),#2621,.T.);
#33592=ADVANCED_FACE('',(#4618),#2622,.T.);
#33593=ADVANCED_FACE('',(#4619),#120,.T.);
#33594=ADVANCED_FACE('',(#4620),#32012,.T.);
#33595=ADVANCED_FACE('',(#4621),#121,.T.);
#33596=ADVANCED_FACE('',(#4622),#2623,.T.);
#33597=ADVANCED_FACE('',(#4623),#2624,.T.);
#33598=ADVANCED_FACE('',(#4624),#122,.T.);
#33599=ADVANCED_FACE('',(#4625),#32013,.T.);
#33600=ADVANCED_FACE('',(#4626),#123,.T.);
#33601=ADVANCED_FACE('',(#4627),#2625,.T.);
#33602=ADVANCED_FACE('',(#4628),#2626,.T.);
#33603=ADVANCED_FACE('',(#4629),#124,.T.);
#33604=ADVANCED_FACE('',(#4630),#32014,.T.);
#33605=ADVANCED_FACE('',(#4631),#125,.T.);
#33606=ADVANCED_FACE('',(#4632),#2627,.T.);
#33607=ADVANCED_FACE('',(#4633),#2628,.T.);
#33608=ADVANCED_FACE('',(#4634),#126,.T.);
#33609=ADVANCED_FACE('',(#4635),#32015,.T.);
#33610=ADVANCED_FACE('',(#4636),#127,.T.);
#33611=ADVANCED_FACE('',(#4637),#2629,.T.);
#33612=ADVANCED_FACE('',(#4638),#2630,.T.);
#33613=ADVANCED_FACE('',(#4639),#128,.T.);
#33614=ADVANCED_FACE('',(#4640),#32016,.T.);
#33615=ADVANCED_FACE('',(#4641),#129,.T.);
#33616=ADVANCED_FACE('',(#4642),#2631,.T.);
#33617=ADVANCED_FACE('',(#4643),#2632,.T.);
#33618=ADVANCED_FACE('',(#4644),#130,.T.);
#33619=ADVANCED_FACE('',(#4645),#32017,.T.);
#33620=ADVANCED_FACE('',(#4646),#131,.T.);
#33621=ADVANCED_FACE('',(#4647),#2633,.T.);
#33622=ADVANCED_FACE('',(#4648),#2634,.T.);
#33623=ADVANCED_FACE('',(#4649),#132,.T.);
#33624=ADVANCED_FACE('',(#4650),#32018,.T.);
#33625=ADVANCED_FACE('',(#4651),#133,.T.);
#33626=ADVANCED_FACE('',(#4652),#2635,.T.);
#33627=ADVANCED_FACE('',(#4653),#2636,.T.);
#33628=ADVANCED_FACE('',(#4654),#134,.T.);
#33629=ADVANCED_FACE('',(#4655),#32019,.T.);
#33630=ADVANCED_FACE('',(#4656),#135,.T.);
#33631=ADVANCED_FACE('',(#4657),#2637,.T.);
#33632=ADVANCED_FACE('',(#4658),#2638,.T.);
#33633=ADVANCED_FACE('',(#4659),#136,.T.);
#33634=ADVANCED_FACE('',(#4660),#32020,.T.);
#33635=ADVANCED_FACE('',(#4661),#137,.T.);
#33636=ADVANCED_FACE('',(#4662),#2639,.T.);
#33637=ADVANCED_FACE('',(#4663),#2640,.T.);
#33638=ADVANCED_FACE('',(#4664),#138,.T.);
#33639=ADVANCED_FACE('',(#4665),#32021,.T.);
#33640=ADVANCED_FACE('',(#4666),#139,.T.);
#33641=ADVANCED_FACE('',(#4667),#2641,.T.);
#33642=ADVANCED_FACE('',(#4668),#2642,.T.);
#33643=ADVANCED_FACE('',(#4669),#32022,.T.);
#33644=ADVANCED_FACE('',(#4670,#1242,#1243,#1244,#1245,#1246,#1247,#1248,
#1249,#1250,#1251,#1252,#1253,#1254,#1255,#1256,#1257,#1258,#1259,#1260,
#1261,#1262),#32023,.T.);
#33645=ADVANCED_FACE('',(#4671),#32024,.T.);
#33646=ADVANCED_FACE('',(#4672,#1263),#2643,.T.);
#33647=ADVANCED_FACE('',(#4673),#32025,.F.);
#33648=ADVANCED_FACE('',(#4674),#3063,.F.);
#33649=ADVANCED_FACE('',(#4675),#32026,.F.);
#33650=ADVANCED_FACE('',(#4676,#1264),#2644,.T.);
#33651=ADVANCED_FACE('',(#4677),#32027,.T.);
#33652=ADVANCED_FACE('',(#4678),#3064,.T.);
#33653=ADVANCED_FACE('',(#4679),#32028,.T.);
#33654=ADVANCED_FACE('',(#4680,#1265),#2645,.T.);
#33655=ADVANCED_FACE('',(#4681),#32029,.F.);
#33656=ADVANCED_FACE('',(#4682),#32030,.F.);
#33657=ADVANCED_FACE('',(#4683),#32031,.F.);
#33658=ADVANCED_FACE('',(#4684,#1266),#2646,.T.);
#33659=ADVANCED_FACE('',(#4685),#32032,.T.);
#33660=ADVANCED_FACE('',(#4686,#1267),#2647,.T.);
#33661=ADVANCED_FACE('',(#4687),#3065,.T.);
#33662=ADVANCED_FACE('',(#4688),#32033,.T.);
#33663=ADVANCED_FACE('',(#4689),#3066,.T.);
#33664=ADVANCED_FACE('',(#4690,#1268),#2648,.T.);
#33665=ADVANCED_FACE('',(#4691),#140,.T.);
#33666=ADVANCED_FACE('',(#4692),#32034,.T.);
#33667=ADVANCED_FACE('',(#4693),#141,.T.);
#33668=ADVANCED_FACE('',(#4694),#2649,.T.);
#33669=ADVANCED_FACE('',(#4695),#2650,.T.);
#33670=ADVANCED_FACE('',(#4696),#142,.T.);
#33671=ADVANCED_FACE('',(#4697),#32035,.T.);
#33672=ADVANCED_FACE('',(#4698),#143,.T.);
#33673=ADVANCED_FACE('',(#4699),#2651,.T.);
#33674=ADVANCED_FACE('',(#4700),#2652,.T.);
#33675=ADVANCED_FACE('',(#4701),#144,.T.);
#33676=ADVANCED_FACE('',(#4702),#32036,.T.);
#33677=ADVANCED_FACE('',(#4703),#145,.T.);
#33678=ADVANCED_FACE('',(#4704),#2653,.T.);
#33679=ADVANCED_FACE('',(#4705),#2654,.T.);
#33680=ADVANCED_FACE('',(#4706),#146,.T.);
#33681=ADVANCED_FACE('',(#4707),#32037,.T.);
#33682=ADVANCED_FACE('',(#4708),#147,.T.);
#33683=ADVANCED_FACE('',(#4709),#2655,.T.);
#33684=ADVANCED_FACE('',(#4710),#2656,.T.);
#33685=ADVANCED_FACE('',(#4711),#148,.T.);
#33686=ADVANCED_FACE('',(#4712),#32038,.T.);
#33687=ADVANCED_FACE('',(#4713),#149,.T.);
#33688=ADVANCED_FACE('',(#4714),#2657,.T.);
#33689=ADVANCED_FACE('',(#4715),#2658,.T.);
#33690=ADVANCED_FACE('',(#4716),#150,.T.);
#33691=ADVANCED_FACE('',(#4717),#32039,.T.);
#33692=ADVANCED_FACE('',(#4718),#151,.T.);
#33693=ADVANCED_FACE('',(#4719),#2659,.T.);
#33694=ADVANCED_FACE('',(#4720),#2660,.T.);
#33695=ADVANCED_FACE('',(#4721),#152,.T.);
#33696=ADVANCED_FACE('',(#4722),#32040,.T.);
#33697=ADVANCED_FACE('',(#4723),#153,.T.);
#33698=ADVANCED_FACE('',(#4724),#2661,.T.);
#33699=ADVANCED_FACE('',(#4725),#2662,.T.);
#33700=ADVANCED_FACE('',(#4726),#154,.T.);
#33701=ADVANCED_FACE('',(#4727),#32041,.T.);
#33702=ADVANCED_FACE('',(#4728),#155,.T.);
#33703=ADVANCED_FACE('',(#4729),#2663,.T.);
#33704=ADVANCED_FACE('',(#4730),#2664,.T.);
#33705=ADVANCED_FACE('',(#4731),#156,.T.);
#33706=ADVANCED_FACE('',(#4732),#32042,.T.);
#33707=ADVANCED_FACE('',(#4733),#157,.T.);
#33708=ADVANCED_FACE('',(#4734),#2665,.T.);
#33709=ADVANCED_FACE('',(#4735),#2666,.T.);
#33710=ADVANCED_FACE('',(#4736),#158,.T.);
#33711=ADVANCED_FACE('',(#4737),#32043,.T.);
#33712=ADVANCED_FACE('',(#4738),#159,.T.);
#33713=ADVANCED_FACE('',(#4739),#2667,.T.);
#33714=ADVANCED_FACE('',(#4740),#2668,.T.);
#33715=ADVANCED_FACE('',(#4741),#160,.T.);
#33716=ADVANCED_FACE('',(#4742),#32044,.T.);
#33717=ADVANCED_FACE('',(#4743),#161,.T.);
#33718=ADVANCED_FACE('',(#4744),#2669,.T.);
#33719=ADVANCED_FACE('',(#4745),#2670,.T.);
#33720=ADVANCED_FACE('',(#4746),#162,.T.);
#33721=ADVANCED_FACE('',(#4747),#32045,.T.);
#33722=ADVANCED_FACE('',(#4748),#163,.T.);
#33723=ADVANCED_FACE('',(#4749),#2671,.T.);
#33724=ADVANCED_FACE('',(#4750),#2672,.T.);
#33725=ADVANCED_FACE('',(#4751),#164,.T.);
#33726=ADVANCED_FACE('',(#4752),#32046,.T.);
#33727=ADVANCED_FACE('',(#4753),#165,.T.);
#33728=ADVANCED_FACE('',(#4754),#2673,.T.);
#33729=ADVANCED_FACE('',(#4755),#2674,.T.);
#33730=ADVANCED_FACE('',(#4756),#166,.T.);
#33731=ADVANCED_FACE('',(#4757),#32047,.T.);
#33732=ADVANCED_FACE('',(#4758),#167,.T.);
#33733=ADVANCED_FACE('',(#4759),#2675,.T.);
#33734=ADVANCED_FACE('',(#4760),#2676,.T.);
#33735=ADVANCED_FACE('',(#4761),#168,.T.);
#33736=ADVANCED_FACE('',(#4762),#32048,.T.);
#33737=ADVANCED_FACE('',(#4763),#169,.T.);
#33738=ADVANCED_FACE('',(#4764),#2677,.T.);
#33739=ADVANCED_FACE('',(#4765),#2678,.T.);
#33740=ADVANCED_FACE('',(#4766),#170,.T.);
#33741=ADVANCED_FACE('',(#4767),#32049,.T.);
#33742=ADVANCED_FACE('',(#4768),#171,.T.);
#33743=ADVANCED_FACE('',(#4769),#2679,.T.);
#33744=ADVANCED_FACE('',(#4770),#2680,.T.);
#33745=ADVANCED_FACE('',(#4771),#172,.T.);
#33746=ADVANCED_FACE('',(#4772),#32050,.T.);
#33747=ADVANCED_FACE('',(#4773),#173,.T.);
#33748=ADVANCED_FACE('',(#4774),#2681,.T.);
#33749=ADVANCED_FACE('',(#4775),#2682,.T.);
#33750=ADVANCED_FACE('',(#4776),#174,.T.);
#33751=ADVANCED_FACE('',(#4777),#32051,.T.);
#33752=ADVANCED_FACE('',(#4778),#175,.T.);
#33753=ADVANCED_FACE('',(#4779),#2683,.T.);
#33754=ADVANCED_FACE('',(#4780),#2684,.T.);
#33755=ADVANCED_FACE('',(#4781),#176,.T.);
#33756=ADVANCED_FACE('',(#4782),#32052,.T.);
#33757=ADVANCED_FACE('',(#4783),#177,.T.);
#33758=ADVANCED_FACE('',(#4784),#2685,.T.);
#33759=ADVANCED_FACE('',(#4785),#2686,.T.);
#33760=ADVANCED_FACE('',(#4786),#178,.T.);
#33761=ADVANCED_FACE('',(#4787),#32053,.T.);
#33762=ADVANCED_FACE('',(#4788),#179,.T.);
#33763=ADVANCED_FACE('',(#4789),#2687,.T.);
#33764=ADVANCED_FACE('',(#4790),#2688,.T.);
#33765=ADVANCED_FACE('',(#4791),#32054,.T.);
#33766=ADVANCED_FACE('',(#4792,#1269,#1270,#1271,#1272,#1273,#1274,#1275,
#1276,#1277,#1278,#1279,#1280,#1281,#1282,#1283,#1284,#1285,#1286,#1287),
#32055,.T.);
#33767=ADVANCED_FACE('',(#4793),#32056,.T.);
#33768=ADVANCED_FACE('',(#4794,#1288),#2689,.T.);
#33769=ADVANCED_FACE('',(#4795),#32057,.F.);
#33770=ADVANCED_FACE('',(#4796),#3067,.F.);
#33771=ADVANCED_FACE('',(#4797),#32058,.F.);
#33772=ADVANCED_FACE('',(#4798,#1289),#2690,.T.);
#33773=ADVANCED_FACE('',(#4799),#2691,.T.);
#33774=ADVANCED_FACE('',(#4800),#2692,.T.);
#33775=ADVANCED_FACE('',(#4801),#2693,.T.);
#33776=ADVANCED_FACE('',(#4802),#2694,.T.);
#33777=ADVANCED_FACE('',(#4803),#2695,.T.);
#33778=ADVANCED_FACE('',(#4804,#1290),#2696,.T.);
#33779=ADVANCED_FACE('',(#4805),#3068,.F.);
#33780=ADVANCED_FACE('',(#4806,#1291),#2697,.T.);
#33781=ADVANCED_FACE('',(#4807),#32059,.T.);
#33782=ADVANCED_FACE('',(#4808),#3069,.T.);
#33783=ADVANCED_FACE('',(#4809),#32060,.T.);
#33784=ADVANCED_FACE('',(#4810),#2698,.T.);
#33785=ADVANCED_FACE('',(#4811),#2699,.T.);
#33786=ADVANCED_FACE('',(#4812),#32061,.T.);
#33787=ADVANCED_FACE('',(#4813),#2700,.F.);
#33788=ADVANCED_FACE('',(#4814),#2701,.T.);
#33789=ADVANCED_FACE('',(#4815),#2702,.T.);
#33790=ADVANCED_FACE('',(#4816),#2703,.T.);
#33791=ADVANCED_FACE('',(#4817),#2704,.F.);
#33792=ADVANCED_FACE('',(#4818),#2705,.F.);
#33793=ADVANCED_FACE('',(#4819),#2706,.T.);
#33794=ADVANCED_FACE('',(#4820),#2707,.T.);
#33795=ADVANCED_FACE('',(#4821),#32062,.F.);
#33796=ADVANCED_FACE('',(#4822),#2708,.T.);
#33797=ADVANCED_FACE('',(#4823),#2709,.T.);
#33798=ADVANCED_FACE('',(#4824),#2710,.T.);
#33799=ADVANCED_FACE('',(#4825),#2711,.T.);
#33800=ADVANCED_FACE('',(#4826),#2712,.T.);
#33801=ADVANCED_FACE('',(#4827),#32063,.F.);
#33802=ADVANCED_FACE('',(#4828),#2713,.T.);
#33803=ADVANCED_FACE('',(#4829),#32064,.T.);
#33804=ADVANCED_FACE('',(#4830),#2714,.T.);
#33805=ADVANCED_FACE('',(#4831),#2715,.T.);
#33806=ADVANCED_FACE('',(#4832),#2716,.T.);
#33807=ADVANCED_FACE('',(#4833),#32065,.T.);
#33808=ADVANCED_FACE('',(#4834),#2717,.T.);
#33809=ADVANCED_FACE('',(#4835),#2718,.T.);
#33810=ADVANCED_FACE('',(#4836),#32066,.T.);
#33811=ADVANCED_FACE('',(#4837),#2719,.F.);
#33812=ADVANCED_FACE('',(#4838),#2720,.T.);
#33813=ADVANCED_FACE('',(#4839),#2721,.T.);
#33814=ADVANCED_FACE('',(#4840),#2722,.T.);
#33815=ADVANCED_FACE('',(#4841),#2723,.T.);
#33816=ADVANCED_FACE('',(#4842),#2724,.T.);
#33817=ADVANCED_FACE('',(#4843),#2725,.T.);
#33818=ADVANCED_FACE('',(#4844),#2726,.T.);
#33819=ADVANCED_FACE('',(#4845),#2727,.T.);
#33820=ADVANCED_FACE('',(#4846),#2728,.T.);
#33821=ADVANCED_FACE('',(#4847),#2729,.T.);
#33822=ADVANCED_FACE('',(#4848),#2730,.F.);
#33823=ADVANCED_FACE('',(#4849),#2731,.F.);
#33824=ADVANCED_FACE('',(#4850),#2732,.T.);
#33825=ADVANCED_FACE('',(#4851),#2733,.T.);
#33826=ADVANCED_FACE('',(#4852),#32067,.F.);
#33827=ADVANCED_FACE('',(#4853),#2734,.T.);
#33828=ADVANCED_FACE('',(#4854),#2735,.T.);
#33829=ADVANCED_FACE('',(#4855),#2736,.T.);
#33830=ADVANCED_FACE('',(#4856),#32068,.T.);
#33831=ADVANCED_FACE('',(#4857),#2737,.F.);
#33832=ADVANCED_FACE('',(#4858),#2738,.F.);
#33833=ADVANCED_FACE('',(#4859),#2739,.T.);
#33834=ADVANCED_FACE('',(#4860),#2740,.T.);
#33835=ADVANCED_FACE('',(#4861),#2741,.T.);
#33836=ADVANCED_FACE('',(#4862),#2742,.F.);
#33837=ADVANCED_FACE('',(#4863),#2743,.T.);
#33838=ADVANCED_FACE('',(#4864),#2744,.F.);
#33839=ADVANCED_FACE('',(#4865),#2745,.T.);
#33840=ADVANCED_FACE('',(#4866),#32069,.F.);
#33841=ADVANCED_FACE('',(#4867),#2746,.T.);
#33842=ADVANCED_FACE('',(#4868),#2747,.T.);
#33843=ADVANCED_FACE('',(#4869),#2748,.T.);
#33844=ADVANCED_FACE('',(#4870),#2749,.T.);
#33845=ADVANCED_FACE('',(#4871),#2750,.T.);
#33846=ADVANCED_FACE('',(#4872),#2751,.T.);
#33847=ADVANCED_FACE('',(#4873),#2752,.T.);
#33848=ADVANCED_FACE('',(#4874),#2753,.T.);
#33849=ADVANCED_FACE('',(#4875),#2754,.T.);
#33850=ADVANCED_FACE('',(#4876),#2755,.T.);
#33851=ADVANCED_FACE('',(#4877),#32070,.F.);
#33852=ADVANCED_FACE('',(#4878),#32071,.F.);
#33853=ADVANCED_FACE('',(#4879),#2756,.T.);
#33854=ADVANCED_FACE('',(#4880),#32072,.F.);
#33855=ADVANCED_FACE('',(#4881),#32073,.F.);
#33856=ADVANCED_FACE('',(#4882),#2757,.T.);
#33857=ADVANCED_FACE('',(#4883),#3070,.F.);
#33858=ADVANCED_FACE('',(#4884),#32074,.F.);
#33859=ADVANCED_FACE('',(#4885),#2758,.T.);
#33860=ADVANCED_FACE('',(#4886),#2759,.T.);
#33861=ADVANCED_FACE('',(#4887),#2760,.T.);
#33862=ADVANCED_FACE('',(#4888),#32075,.T.);
#33863=ADVANCED_FACE('',(#4889),#2761,.T.);
#33864=ADVANCED_FACE('',(#4890),#2762,.T.);
#33865=ADVANCED_FACE('',(#4891),#2763,.T.);
#33866=ADVANCED_FACE('',(#4892),#2764,.T.);
#33867=ADVANCED_FACE('',(#4893),#2765,.T.);
#33868=ADVANCED_FACE('',(#4894),#2766,.T.);
#33869=ADVANCED_FACE('',(#4895),#2767,.T.);
#33870=ADVANCED_FACE('',(#4896),#32076,.F.);
#33871=ADVANCED_FACE('',(#4897),#2768,.T.);
#33872=ADVANCED_FACE('',(#4898),#32077,.F.);
#33873=ADVANCED_FACE('',(#4899),#2769,.T.);
#33874=ADVANCED_FACE('',(#4900),#2770,.T.);
#33875=ADVANCED_FACE('',(#4901),#32078,.F.);
#33876=ADVANCED_FACE('',(#4902),#2771,.F.);
#33877=ADVANCED_FACE('',(#4903),#2772,.F.);
#33878=ADVANCED_FACE('',(#4904),#2773,.T.);
#33879=ADVANCED_FACE('',(#4905),#2774,.T.);
#33880=ADVANCED_FACE('',(#4906),#2775,.T.);
#33881=ADVANCED_FACE('',(#4907),#2776,.T.);
#33882=ADVANCED_FACE('',(#4908),#2777,.T.);
#33883=ADVANCED_FACE('',(#4909),#2778,.T.);
#33884=ADVANCED_FACE('',(#4910),#32079,.T.);
#33885=ADVANCED_FACE('',(#4911),#32080,.F.);
#33886=ADVANCED_FACE('',(#4912),#2779,.F.);
#33887=ADVANCED_FACE('',(#4913),#2780,.F.);
#33888=ADVANCED_FACE('',(#4914),#2781,.F.);
#33889=ADVANCED_FACE('',(#4915),#2782,.T.);
#33890=ADVANCED_FACE('',(#4916),#2783,.T.);
#33891=ADVANCED_FACE('',(#4917),#2784,.F.);
#33892=ADVANCED_FACE('',(#4918),#2785,.F.);
#33893=ADVANCED_FACE('',(#4919),#2786,.F.);
#33894=ADVANCED_FACE('',(#4920),#2787,.T.);
#33895=ADVANCED_FACE('',(#4921,#1292),#2788,.F.);
#33896=ADVANCED_FACE('',(#4922),#32081,.T.);
#33897=ADVANCED_FACE('',(#4923),#3071,.T.);
#33898=ADVANCED_FACE('',(#4924),#2789,.T.);
#33899=ADVANCED_FACE('',(#4925),#32082,.T.);
#33900=ADVANCED_FACE('',(#4926),#2790,.T.);
#33901=ADVANCED_FACE('',(#4927),#2791,.F.);
#33902=ADVANCED_FACE('',(#4928),#2792,.T.);
#33903=ADVANCED_FACE('',(#4929),#2793,.F.);
#33904=ADVANCED_FACE('',(#4930),#2794,.T.);
#33905=ADVANCED_FACE('',(#4931),#2795,.T.);
#33906=ADVANCED_FACE('',(#4932),#2796,.T.);
#33907=ADVANCED_FACE('',(#4933),#2797,.F.);
#33908=ADVANCED_FACE('',(#4934),#32083,.T.);
#33909=ADVANCED_FACE('',(#4935),#2798,.F.);
#33910=ADVANCED_FACE('',(#4936),#2799,.F.);
#33911=ADVANCED_FACE('',(#4937,#1293),#180,.T.);
#33912=ADVANCED_FACE('',(#4938),#2800,.T.);
#33913=ADVANCED_FACE('',(#4939),#32084,.T.);
#33914=ADVANCED_FACE('',(#4940),#32085,.T.);
#33915=ADVANCED_FACE('',(#4941),#32086,.T.);
#33916=ADVANCED_FACE('',(#4942),#32087,.T.);
#33917=ADVANCED_FACE('',(#4943),#32088,.T.);
#33918=ADVANCED_FACE('',(#4944),#32089,.T.);
#33919=ADVANCED_FACE('',(#4945),#32090,.T.);
#33920=ADVANCED_FACE('',(#4946),#32091,.T.);
#33921=ADVANCED_FACE('',(#4947),#3072,.T.);
#33922=ADVANCED_FACE('',(#4948,#1294),#2801,.T.);
#33923=ADVANCED_FACE('',(#4949),#32092,.T.);
#33924=ADVANCED_FACE('',(#4950),#3073,.T.);
#33925=ADVANCED_FACE('',(#4951,#1295),#2802,.T.);
#33926=ADVANCED_FACE('',(#4952),#3074,.T.);
#33927=ADVANCED_FACE('',(#4953),#32093,.T.);
#33928=ADVANCED_FACE('',(#4954),#2803,.T.);
#33929=ADVANCED_FACE('',(#4955),#2804,.T.);
#33930=ADVANCED_FACE('',(#4956),#32094,.F.);
#33931=ADVANCED_FACE('',(#4957),#32095,.F.);
#33932=ADVANCED_FACE('',(#4958),#32096,.F.);
#33933=ADVANCED_FACE('',(#4959),#32097,.F.);
#33934=ADVANCED_FACE('',(#4960),#32098,.F.);
#33935=ADVANCED_FACE('',(#4961),#3075,.F.);
#33936=ADVANCED_FACE('',(#4962),#3076,.T.);
#33937=ADVANCED_FACE('',(#4963),#3077,.T.);
#33938=ADVANCED_FACE('',(#4964),#3078,.T.);
#33939=ADVANCED_FACE('',(#4965),#3079,.T.);
#33940=ADVANCED_FACE('',(#4966),#3080,.T.);
#33941=ADVANCED_FACE('',(#4967),#3081,.T.);
#33942=ADVANCED_FACE('',(#4968),#3082,.T.);
#33943=ADVANCED_FACE('',(#4969),#3083,.T.);
#33944=ADVANCED_FACE('',(#4970),#3084,.T.);
#33945=ADVANCED_FACE('',(#4971),#3085,.T.);
#33946=ADVANCED_FACE('',(#4972),#3086,.T.);
#33947=ADVANCED_FACE('',(#4973),#3087,.T.);
#33948=ADVANCED_FACE('',(#4974),#3088,.T.);
#33949=ADVANCED_FACE('',(#4975),#3089,.T.);
#33950=ADVANCED_FACE('',(#4976),#3090,.T.);
#33951=ADVANCED_FACE('',(#4977),#3091,.T.);
#33952=ADVANCED_FACE('',(#4978),#3092,.T.);
#33953=ADVANCED_FACE('',(#4979),#3093,.T.);
#33954=ADVANCED_FACE('',(#4980),#3094,.T.);
#33955=ADVANCED_FACE('',(#4981),#3095,.T.);
#33956=ADVANCED_FACE('',(#4982),#3096,.T.);
#33957=ADVANCED_FACE('',(#4983),#3097,.T.);
#33958=ADVANCED_FACE('',(#4984),#3098,.T.);
#33959=ADVANCED_FACE('',(#4985),#3099,.T.);
#33960=ADVANCED_FACE('',(#4986),#3100,.T.);
#33961=ADVANCED_FACE('',(#4987),#3101,.T.);
#33962=ADVANCED_FACE('',(#4988),#3102,.T.);
#33963=ADVANCED_FACE('',(#4989),#3103,.T.);
#33964=ADVANCED_FACE('',(#4990),#3104,.T.);
#33965=ADVANCED_FACE('',(#4991),#3105,.T.);
#33966=ADVANCED_FACE('',(#4992),#3106,.T.);
#33967=ADVANCED_FACE('',(#4993),#3107,.T.);
#33968=ADVANCED_FACE('',(#4994),#3108,.T.);
#33969=ADVANCED_FACE('',(#4995),#3109,.T.);
#33970=ADVANCED_FACE('',(#4996),#3110,.T.);
#33971=ADVANCED_FACE('',(#4997),#3111,.T.);
#33972=ADVANCED_FACE('',(#4998),#3112,.T.);
#33973=ADVANCED_FACE('',(#4999),#3113,.T.);
#33974=ADVANCED_FACE('',(#5000),#3114,.T.);
#33975=ADVANCED_FACE('',(#5001),#3115,.T.);
#33976=ADVANCED_FACE('',(#5002),#3116,.T.);
#33977=ADVANCED_FACE('',(#5003),#3117,.T.);
#33978=ADVANCED_FACE('',(#5004),#3118,.T.);
#33979=ADVANCED_FACE('',(#5005),#3119,.T.);
#33980=ADVANCED_FACE('',(#5006),#3120,.T.);
#33981=ADVANCED_FACE('',(#5007),#3121,.T.);
#33982=ADVANCED_FACE('',(#5008),#3122,.T.);
#33983=ADVANCED_FACE('',(#5009),#3123,.T.);
#33984=ADVANCED_FACE('',(#5010),#3124,.T.);
#33985=ADVANCED_FACE('',(#5011),#3125,.T.);
#33986=ADVANCED_FACE('',(#5012),#3126,.T.);
#33987=ADVANCED_FACE('',(#5013),#3127,.T.);
#33988=ADVANCED_FACE('',(#5014),#3128,.T.);
#33989=ADVANCED_FACE('',(#5015),#3129,.T.);
#33990=ADVANCED_FACE('',(#5016),#3130,.T.);
#33991=ADVANCED_FACE('',(#5017),#3131,.T.);
#33992=ADVANCED_FACE('',(#5018),#3132,.T.);
#33993=ADVANCED_FACE('',(#5019),#3133,.T.);
#33994=ADVANCED_FACE('',(#5020),#32099,.T.);
#33995=ADVANCED_FACE('',(#5021),#32100,.T.);
#33996=ADVANCED_FACE('',(#5022),#2805,.T.);
#33997=ADVANCED_FACE('',(#5023),#2806,.T.);
#33998=ADVANCED_FACE('',(#5024,#1296),#2807,.T.);
#33999=ADVANCED_FACE('',(#5025),#2808,.T.);
#34000=ADVANCED_FACE('',(#5026),#3134,.T.);
#34001=ADVANCED_FACE('',(#5027),#32101,.T.);
#34002=ADVANCED_FACE('',(#5028),#2809,.T.);
#34003=ADVANCED_FACE('',(#5029),#2810,.F.);
#34004=ADVANCED_FACE('',(#5030),#2811,.T.);
#34005=ADVANCED_FACE('',(#5031),#2812,.T.);
#34006=ADVANCED_FACE('',(#5032),#32102,.T.);
#34007=ADVANCED_FACE('',(#5033),#2813,.F.);
#34008=ADVANCED_FACE('',(#5034),#287,.F.);
#34009=ADVANCED_FACE('',(#5035),#2814,.T.);
#34010=ADVANCED_FACE('',(#5036),#3135,.T.);
#34011=ADVANCED_FACE('',(#5037),#288,.F.);
#34012=ADVANCED_FACE('',(#5038),#3136,.T.);
#34013=ADVANCED_FACE('',(#5039),#2815,.F.);
#34014=ADVANCED_FACE('',(#5040),#2816,.T.);
#34015=ADVANCED_FACE('',(#5041),#2817,.F.);
#34016=ADVANCED_FACE('',(#5042),#2818,.F.);
#34017=ADVANCED_FACE('',(#5043),#2819,.F.);
#34018=ADVANCED_FACE('',(#5044),#2820,.T.);
#34019=ADVANCED_FACE('',(#5045),#2821,.F.);
#34020=ADVANCED_FACE('',(#5046),#2822,.F.);
#34021=ADVANCED_FACE('',(#5047),#2823,.F.);
#34022=ADVANCED_FACE('',(#5048),#2824,.T.);
#34023=ADVANCED_FACE('',(#5049),#2825,.F.);
#34024=ADVANCED_FACE('',(#5050),#2826,.F.);
#34025=ADVANCED_FACE('',(#5051),#2827,.F.);
#34026=ADVANCED_FACE('',(#5052),#2828,.T.);
#34027=ADVANCED_FACE('',(#5053),#2829,.F.);
#34028=ADVANCED_FACE('',(#5054),#2830,.F.);
#34029=ADVANCED_FACE('',(#5055),#2831,.F.);
#34030=ADVANCED_FACE('',(#5056),#2832,.T.);
#34031=ADVANCED_FACE('',(#5057),#2833,.F.);
#34032=ADVANCED_FACE('',(#5058),#2834,.F.);
#34033=ADVANCED_FACE('',(#5059),#2835,.F.);
#34034=ADVANCED_FACE('',(#5060),#2836,.T.);
#34035=ADVANCED_FACE('',(#5061),#2837,.F.);
#34036=ADVANCED_FACE('',(#5062),#2838,.F.);
#34037=ADVANCED_FACE('',(#5063),#2839,.F.);
#34038=ADVANCED_FACE('',(#5064),#2840,.T.);
#34039=ADVANCED_FACE('',(#5065),#2841,.F.);
#34040=ADVANCED_FACE('',(#5066),#2842,.F.);
#34041=ADVANCED_FACE('',(#5067),#2843,.F.);
#34042=ADVANCED_FACE('',(#5068),#2844,.T.);
#34043=ADVANCED_FACE('',(#5069),#2845,.F.);
#34044=ADVANCED_FACE('',(#5070),#2846,.F.);
#34045=ADVANCED_FACE('',(#5071),#2847,.F.);
#34046=ADVANCED_FACE('',(#5072),#2848,.T.);
#34047=ADVANCED_FACE('',(#5073),#2849,.F.);
#34048=ADVANCED_FACE('',(#5074),#2850,.F.);
#34049=ADVANCED_FACE('',(#5075),#2851,.F.);
#34050=ADVANCED_FACE('',(#5076),#2852,.T.);
#34051=ADVANCED_FACE('',(#5077),#2853,.F.);
#34052=ADVANCED_FACE('',(#5078),#2854,.F.);
#34053=ADVANCED_FACE('',(#5079),#2855,.F.);
#34054=ADVANCED_FACE('',(#5080),#2856,.T.);
#34055=ADVANCED_FACE('',(#5081),#2857,.F.);
#34056=ADVANCED_FACE('',(#5082),#2858,.F.);
#34057=ADVANCED_FACE('',(#5083),#2859,.F.);
#34058=ADVANCED_FACE('',(#5084),#2860,.T.);
#34059=ADVANCED_FACE('',(#5085),#2861,.F.);
#34060=ADVANCED_FACE('',(#5086),#2862,.F.);
#34061=ADVANCED_FACE('',(#5087),#2863,.F.);
#34062=ADVANCED_FACE('',(#5088),#2864,.T.);
#34063=ADVANCED_FACE('',(#5089),#2865,.F.);
#34064=ADVANCED_FACE('',(#5090),#2866,.F.);
#34065=ADVANCED_FACE('',(#5091),#2867,.F.);
#34066=ADVANCED_FACE('',(#5092),#2868,.T.);
#34067=ADVANCED_FACE('',(#5093),#2869,.F.);
#34068=ADVANCED_FACE('',(#5094),#2870,.F.);
#34069=ADVANCED_FACE('',(#5095),#2871,.F.);
#34070=ADVANCED_FACE('',(#5096),#2872,.T.);
#34071=ADVANCED_FACE('',(#5097),#2873,.F.);
#34072=ADVANCED_FACE('',(#5098),#2874,.F.);
#34073=ADVANCED_FACE('',(#5099),#2875,.F.);
#34074=ADVANCED_FACE('',(#5100),#2876,.T.);
#34075=ADVANCED_FACE('',(#5101),#2877,.F.);
#34076=ADVANCED_FACE('',(#5102),#2878,.F.);
#34077=ADVANCED_FACE('',(#5103),#2879,.F.);
#34078=ADVANCED_FACE('',(#5104),#2880,.T.);
#34079=ADVANCED_FACE('',(#5105),#2881,.F.);
#34080=ADVANCED_FACE('',(#5106),#2882,.F.);
#34081=ADVANCED_FACE('',(#5107),#2883,.F.);
#34082=ADVANCED_FACE('',(#5108),#2884,.T.);
#34083=ADVANCED_FACE('',(#5109),#2885,.F.);
#34084=ADVANCED_FACE('',(#5110),#2886,.F.);
#34085=ADVANCED_FACE('',(#5111),#2887,.F.);
#34086=ADVANCED_FACE('',(#5112),#2888,.T.);
#34087=ADVANCED_FACE('',(#5113),#2889,.F.);
#34088=ADVANCED_FACE('',(#5114),#2890,.F.);
#34089=ADVANCED_FACE('',(#5115),#2891,.F.);
#34090=ADVANCED_FACE('',(#5116),#2892,.T.);
#34091=ADVANCED_FACE('',(#5117),#2893,.F.);
#34092=ADVANCED_FACE('',(#5118),#2894,.F.);
#34093=ADVANCED_FACE('',(#5119),#2895,.F.);
#34094=ADVANCED_FACE('',(#5120),#2896,.T.);
#34095=ADVANCED_FACE('',(#5121),#2897,.F.);
#34096=ADVANCED_FACE('',(#5122),#2898,.F.);
#34097=ADVANCED_FACE('',(#5123),#2899,.F.);
#34098=ADVANCED_FACE('',(#5124),#2900,.T.);
#34099=ADVANCED_FACE('',(#5125),#2901,.F.);
#34100=ADVANCED_FACE('',(#5126),#2902,.F.);
#34101=ADVANCED_FACE('',(#5127),#2903,.F.);
#34102=ADVANCED_FACE('',(#5128),#2904,.T.);
#34103=ADVANCED_FACE('',(#5129),#2905,.F.);
#34104=ADVANCED_FACE('',(#5130),#2906,.F.);
#34105=ADVANCED_FACE('',(#5131),#2907,.F.);
#34106=ADVANCED_FACE('',(#5132),#2908,.T.);
#34107=ADVANCED_FACE('',(#5133),#2909,.F.);
#34108=ADVANCED_FACE('',(#5134),#2910,.F.);
#34109=ADVANCED_FACE('',(#5135),#2911,.F.);
#34110=ADVANCED_FACE('',(#5136),#2912,.T.);
#34111=ADVANCED_FACE('',(#5137),#2913,.F.);
#34112=ADVANCED_FACE('',(#5138),#2914,.F.);
#34113=ADVANCED_FACE('',(#5139),#2915,.F.);
#34114=ADVANCED_FACE('',(#5140),#2916,.T.);
#34115=ADVANCED_FACE('',(#5141),#2917,.F.);
#34116=ADVANCED_FACE('',(#5142),#2918,.F.);
#34117=ADVANCED_FACE('',(#5143),#2919,.F.);
#34118=ADVANCED_FACE('',(#5144),#2920,.T.);
#34119=ADVANCED_FACE('',(#5145),#2921,.F.);
#34120=ADVANCED_FACE('',(#5146),#2922,.F.);
#34121=ADVANCED_FACE('',(#5147),#2923,.F.);
#34122=ADVANCED_FACE('',(#5148),#2924,.T.);
#34123=ADVANCED_FACE('',(#5149),#2925,.F.);
#34124=ADVANCED_FACE('',(#5150),#2926,.F.);
#34125=ADVANCED_FACE('',(#5151),#2927,.F.);
#34126=ADVANCED_FACE('',(#5152),#2928,.T.);
#34127=ADVANCED_FACE('',(#5153),#2929,.F.);
#34128=ADVANCED_FACE('',(#5154),#2930,.F.);
#34129=ADVANCED_FACE('',(#5155),#2931,.F.);
#34130=ADVANCED_FACE('',(#5156),#2932,.T.);
#34131=ADVANCED_FACE('',(#5157),#2933,.F.);
#34132=ADVANCED_FACE('',(#5158),#2934,.F.);
#34133=ADVANCED_FACE('',(#5159),#2935,.F.);
#34134=ADVANCED_FACE('',(#5160),#2936,.T.);
#34135=ADVANCED_FACE('',(#5161),#2937,.F.);
#34136=ADVANCED_FACE('',(#5162),#2938,.F.);
#34137=ADVANCED_FACE('',(#5163),#2939,.F.);
#34138=ADVANCED_FACE('',(#5164),#2940,.T.);
#34139=ADVANCED_FACE('',(#5165),#2941,.F.);
#34140=ADVANCED_FACE('',(#5166),#2942,.F.);
#34141=ADVANCED_FACE('',(#5167),#2943,.F.);
#34142=ADVANCED_FACE('',(#5168),#2944,.T.);
#34143=ADVANCED_FACE('',(#5169),#2945,.F.);
#34144=ADVANCED_FACE('',(#5170),#2946,.F.);
#34145=ADVANCED_FACE('',(#5171),#2947,.F.);
#34146=ADVANCED_FACE('',(#5172),#2948,.T.);
#34147=ADVANCED_FACE('',(#5173),#2949,.F.);
#34148=ADVANCED_FACE('',(#5174),#2950,.F.);
#34149=ADVANCED_FACE('',(#5175),#2951,.F.);
#34150=ADVANCED_FACE('',(#5176),#2952,.T.);
#34151=ADVANCED_FACE('',(#5177),#2953,.F.);
#34152=ADVANCED_FACE('',(#5178),#2954,.F.);
#34153=ADVANCED_FACE('',(#5179),#2955,.F.);
#34154=ADVANCED_FACE('',(#5180),#2956,.T.);
#34155=ADVANCED_FACE('',(#5181),#2957,.F.);
#34156=ADVANCED_FACE('',(#5182),#2958,.F.);
#34157=ADVANCED_FACE('',(#5183,#1297,#1298,#1299,#1300,#1301,#1302,#1303,
#1304,#1305,#1306,#1307,#1308,#1309,#1310,#1311,#1312,#1313,#1314,#1315,
#1316,#1317,#1318,#1319,#1320,#1321,#1322,#1323,#1324,#1325,#1326,#1327,
#1328,#1329,#1330,#1331),#3137,.T.);
#34158=ADVANCED_FACE('',(#5184),#32103,.T.);
#34159=ADVANCED_FACE('',(#5185),#32104,.T.);
#34160=ADVANCED_FACE('',(#5186),#289,.T.);
#34161=ADVANCED_FACE('',(#5187),#290,.T.);
#34162=ADVANCED_FACE('',(#5188),#32105,.T.);
#34163=ADVANCED_FACE('',(#5189),#32106,.T.);
#34164=ADVANCED_FACE('',(#5190),#32107,.T.);
#34165=ADVANCED_FACE('',(#5191),#32108,.T.);
#34166=ADVANCED_FACE('',(#5192),#32109,.T.);
#34167=ADVANCED_FACE('',(#5193),#32110,.T.);
#34168=ADVANCED_FACE('',(#5194),#291,.T.);
#34169=ADVANCED_FACE('',(#5195,#1332),#2959,.T.);
#34170=ADVANCED_FACE('',(#5196),#2960,.T.);
#34171=ADVANCED_FACE('',(#5197),#2961,.T.);
#34172=ADVANCED_FACE('',(#5198),#2962,.T.);
#34173=ADVANCED_FACE('',(#5199),#2963,.T.);
#34174=ADVANCED_FACE('',(#5200),#2964,.T.);
#34175=ADVANCED_FACE('',(#5201),#2965,.T.);
#34176=ADVANCED_FACE('',(#5202),#2966,.T.);
#34177=ADVANCED_FACE('',(#5203),#2967,.T.);
#34178=ADVANCED_FACE('',(#5204),#2968,.T.);
#34179=ADVANCED_FACE('',(#5205),#2969,.T.);
#34180=ADVANCED_FACE('',(#5206),#2970,.T.);
#34181=ADVANCED_FACE('',(#5207),#2971,.T.);
#34182=ADVANCED_FACE('',(#5208),#2972,.T.);
#34183=ADVANCED_FACE('',(#5209),#2973,.T.);
#34184=ADVANCED_FACE('',(#5210),#2974,.T.);
#34185=ADVANCED_FACE('',(#5211),#292,.T.);
#34186=ADVANCED_FACE('',(#5212),#2975,.T.);
#34187=ADVANCED_FACE('',(#5213),#293,.T.);
#34188=ADVANCED_FACE('',(#5214),#2976,.T.);
#34189=ADVANCED_FACE('',(#5215),#2977,.T.);
#34190=ADVANCED_FACE('',(#5216),#294,.T.);
#34191=ADVANCED_FACE('',(#5217),#2978,.T.);
#34192=ADVANCED_FACE('',(#5218),#2979,.T.);
#34193=ADVANCED_FACE('',(#5219),#2980,.T.);
#34194=ADVANCED_FACE('',(#5220),#2981,.T.);
#34195=ADVANCED_FACE('',(#5221),#2982,.T.);
#34196=ADVANCED_FACE('',(#5222),#2983,.T.);
#34197=ADVANCED_FACE('',(#5223),#2984,.T.);
#34198=ADVANCED_FACE('',(#5224,#1333),#2985,.F.);
#34199=ADVANCED_FACE('',(#5225),#2986,.T.);
#34200=ADVANCED_FACE('',(#5226),#2987,.T.);
#34201=ADVANCED_FACE('',(#5227),#2988,.T.);
#34202=ADVANCED_FACE('',(#5228),#2989,.T.);
#34203=ADVANCED_FACE('',(#5229),#2990,.T.);
#34204=ADVANCED_FACE('',(#5230),#32111,.F.);
#34205=ADVANCED_FACE('',(#5231),#32112,.T.);
#34206=ADVANCED_FACE('',(#5232,#1334),#2991,.T.);
#34207=ADVANCED_FACE('',(#5233),#3138,.F.);
#34208=CLOSED_SHELL('',(#32113,#32114,#32115,#32116,#32117,#32118,#32119,
#32120,#32121,#32122,#32123,#32124,#32125,#32126,#32127,#32128,#32129,#32130,
#32131,#32132,#32133,#32134,#32135,#32136,#32137,#32138,#32139,#32140,#32141,
#32142,#32143,#32144,#32145,#32146,#32147,#32148,#32149,#32150,#32151,#32152,
#32153,#32154,#32155,#32156,#32157,#32158,#32159,#32160,#32161,#32162,#32163,
#32164,#32165,#32166,#32167,#32168,#32169,#32170,#32171,#32172,#32173,#32174,
#32175,#32176,#32177,#32178,#32179,#32180,#32181,#32182,#32183,#32184,#32185,
#32186,#32187,#32188,#32189,#32190,#32191,#32192,#32193,#32194,#32195,#32196,
#32197,#32198,#32199,#32200,#32201,#32202,#32203,#32204,#32205,#32206,#32207,
#32208,#32209,#32210,#32211,#32212,#32213,#32214,#32215,#32216,#32217,#32218,
#32219,#32220,#32221,#32222,#32223,#32224,#32225,#32226,#32227,#32228,#32229,
#32230,#32231,#32232,#32233,#32234,#32235,#32236,#32237,#32238,#32239,#32240,
#32241,#32242,#32243,#32244,#32245,#32246,#32247,#32248,#32249,#32250,#32251,
#32252,#32253,#32254,#32255,#32256,#32257,#32258,#32259,#32260,#32261,#32262,
#32263,#32264,#32265,#32266,#32267,#32268,#32269,#32270,#32271,#32272,#32273,
#32274,#32275,#32276,#32277,#32278,#32279,#32280,#32281,#32282,#32283,#32284,
#32285,#32286,#32287,#32288,#32289,#32290,#32291,#32292,#32293,#32294,#32295,
#32296,#32297,#32298,#32299,#32300,#32301,#32302,#32303,#32304,#32305,#32306,
#32307,#32308,#32309,#32310,#32311,#32312,#32313,#32314,#32315,#32316,#32317,
#32318,#32319,#32320,#32321,#32322,#32323,#32324,#32325,#32326,#32327,#32328,
#32329,#32330,#32331,#32332,#32333,#32334,#32335,#32336,#32337,#32338,#32339,
#32340,#32341,#32342,#32343,#32344,#32345,#32346,#32347,#32348,#32349,#32350,
#32351,#32352,#32353,#32354,#32355,#32356,#32357,#32358,#32359,#32360,#32361,
#32362,#32363,#32364,#32365,#32366,#32367,#32368,#32369,#32370,#32371,#32372,
#32373,#32374,#32375,#32376,#32377,#32378,#32379,#32380,#32381,#32382,#32383,
#32384,#32385,#32386,#32387,#32388,#32389,#32390,#32391,#32392,#32393,#32394,
#32395,#32396,#32397,#32398,#32399,#32400,#32401,#32402,#32403,#32404,#32405,
#32406,#32407,#32408,#32409,#32410,#32411,#32412,#32413,#32414,#32415,#32416,
#32417,#32418,#32419,#32420,#32421,#32422,#32423,#32424,#32425,#32426,#32427,
#32428,#32429,#32430,#32431,#32432,#32433,#32434,#32435,#32436,#32437,#32438,
#32439,#32440,#32441,#32442,#32443,#32444,#32445,#32446,#32447,#32448,#32449,
#32450,#32451,#32452,#32453,#32454,#32455,#32456,#32457,#32458,#32459,#32460,
#32461,#32462,#32463,#32464,#32465,#32466,#32467,#32468,#32469,#32470,#32471,
#32472,#32473,#32474,#32475,#32476,#32477,#32478,#32479,#32480,#32481,#32482,
#32483,#32484,#32485,#32486,#32487,#32488,#32489,#32490,#32491,#32492,#32493,
#32494,#32495,#32496,#32497,#32498,#32499,#32500,#32501,#32502,#32503,#32504,
#32505,#32506,#32507,#32508,#32509,#32510,#32511,#32512,#32513,#32514,#32515,
#32516,#32517,#32518,#32519,#32520,#32521,#32522,#32523,#32524,#32525,#32526,
#32527,#32528,#32529,#32530,#32531,#32532,#32533,#32534,#32535,#32536,#32537,
#32538,#32539,#32540,#32541,#32542,#32543,#32544,#32545,#32546,#32547,#32548,
#32549,#32550,#32551,#32552,#32553,#32554,#32555,#32556,#32557,#32558,#32559,
#32560,#32561,#32562,#32563,#32564,#32565,#32566,#32567,#32568,#32569,#32570,
#32571,#32572,#32573,#32574,#32575,#32576,#32577,#32578,#32579,#32580,#32581,
#32582,#32583,#32584,#32585,#32586,#32587,#32588,#32589,#32590,#32591,#32592,
#32593,#32594,#32595,#32596,#32597,#32598,#32599,#32600,#32601,#32602,#32603,
#32604,#32605,#32606,#32607,#32608,#32609,#32610,#32611,#32612,#32613,#32614,
#32615,#32616,#32617,#32618,#32619,#32620,#32621,#32622,#32623,#32624,#32625,
#32626,#32627,#32628,#32629,#32630,#32631,#32632,#32633,#32634,#32635,#32636,
#32637,#32638,#32639,#32640,#32641,#32642,#32643,#32644,#32645,#32646,#32647,
#32648,#32649,#32650,#32651,#32652,#32653,#32654,#32655,#32656,#32657,#32658,
#32659,#32660,#32661,#32662,#32663,#32664,#32665,#32666,#32667,#32668,#32669,
#32670,#32671,#32672,#32673,#32674,#32675,#32676,#32677,#32678,#32679,#32680,
#32681,#32682,#32683,#32684,#32685,#32686,#32687,#32688,#32689,#32690,#32691,
#32692,#32693,#32694,#32695,#32696,#32697,#32698,#32699,#32700,#32701,#32702,
#32703,#32704,#32705,#32706,#32707,#32708,#32709,#32710,#32711,#32712,#32713,
#32714,#32715,#32716,#32717,#32718,#32719,#32720,#32721,#32722,#32723,#32724,
#32725,#32726,#32727,#32728,#32729,#32730,#32731,#32732,#32733,#32734,#32735,
#32736,#32737,#32738,#32739,#32740,#32741,#32742,#32743,#32744,#32745,#32746,
#32747,#32748,#32749,#32750,#32751,#32752,#32753,#32754,#32755,#32756,#32757,
#32758,#32759,#32760,#32761,#32762,#32763,#32764,#32765,#32766,#32767,#32768,
#32769,#32770,#32771,#32772,#32773,#32774,#32775,#32776,#32777,#32778,#32779,
#32780,#32781,#32782,#32783,#32784,#32785,#32786,#32787,#32788,#32789,#32790,
#32791,#32792,#32793,#32794,#32795,#32796,#32797,#32798,#32799,#32800,#32801,
#32802,#32803,#32804,#32805,#32806,#32807,#32808,#32809,#32810,#32811,#32812,
#32813,#32814,#32815,#32816,#32817,#32818,#32819,#32820,#32821,#32822,#32823,
#32824,#32825,#32826,#32827,#32828,#32829,#32830,#32831,#32832,#32833,#32834,
#32835,#32836,#32837,#32838,#32839,#32840,#32841,#32842,#32843,#32844,#32845,
#32846,#32847,#32848,#32849,#32850,#32851,#32852,#32853,#32854,#32855,#32856,
#32857,#32858,#32859,#32860,#32861,#32862,#32863,#32864,#32865,#32866,#32867,
#32868,#32869,#32870,#32871,#32872,#32873,#32874,#32875,#32876,#32877,#32878,
#32879,#32880,#32881,#32882,#32883,#32884,#32885,#32886,#32887,#32888,#32889,
#32890,#32891,#32892,#32893,#32894,#32895,#32896,#32897,#32898,#32899,#32900,
#32901,#32902,#32903,#32904,#32905,#32906,#32907,#32908,#32909,#32910,#32911,
#32912,#32913,#32914,#32915,#32916,#32917,#32918,#32919,#32920,#32921,#32922,
#32923,#32924,#32925,#32926,#32927,#32928,#32929,#32930,#32931,#32932,#32933,
#32934,#32935,#32936,#32937,#32938,#32939,#32940,#32941,#32942,#32943,#32944,
#32945,#32946,#32947,#32948,#32949,#32950,#32951,#32952,#32953,#32954,#32955,
#32956,#32957,#32958,#32959,#32960,#32961,#32962,#32963,#32964,#32965,#32966,
#32967,#32968,#32969,#32970,#32971,#32972,#32973,#32974,#32975,#32976,#32977,
#32978,#32979,#32980,#32981,#32982,#32983,#32984,#32985,#32986,#32987,#32988,
#32989,#32990,#32991,#32992,#32993,#32994,#32995,#32996,#32997,#32998,#32999,
#33000,#33001,#33002,#33003,#33004,#33005,#33006,#33007,#33008,#33009,#33010,
#33011,#33012,#33013,#33014,#33015,#33016,#33017,#33018,#33019,#33020,#33021,
#33022,#33023,#33024,#33025,#33026,#33027,#33028,#33029,#33030,#33031,#33032,
#33033,#33034,#33035,#33036,#33037,#33038,#33039,#33040,#33041,#33042,#33043,
#33044,#33045,#33046,#33047,#33048,#33049,#33050,#33051,#33052,#33053,#33054,
#33055,#33056,#33057,#33058,#33059,#33060,#33061,#33062,#33063,#33064,#33065,
#33066,#33067,#33068,#33069,#33070,#33071,#33072,#33073,#33074,#33075,#33076,
#33077,#33078,#33079,#33080,#33081,#33082,#33083,#33084,#33085,#33086,#33087,
#33088,#33089,#33090,#33091,#33092,#33093,#33094,#33095,#33096,#33097,#33098,
#33099,#33100,#33101,#33102,#33103,#33104,#33105,#33106,#33107,#33108,#33109,
#33110,#33111,#33112,#33113,#33114,#33115,#33116,#33117,#33118,#33119,#33120,
#33121,#33122,#33123,#33124,#33125,#33126,#33127,#33128,#33129,#33130,#33131,
#33132,#33133,#33134,#33135,#33136,#33137,#33138,#33139,#33140,#33141,#33142,
#33143,#33144,#33145,#33146,#33147,#33148,#33149,#33150,#33151,#33152,#33153,
#33154,#33155,#33156,#33157,#33158,#33159,#33160,#33161,#33162,#33163,#33164,
#33165,#33166,#33167,#33168,#33169,#33170,#33171,#33172,#33173,#33174,#33175,
#33176,#33177,#33178,#33179,#33180,#33181,#33182,#33183,#33184,#33185,#33186,
#33187,#33188,#33189,#33190,#33191,#33192,#33193,#33194,#33195,#33196,#33197,
#33198,#33199,#33200,#33201,#33202,#33203,#33204,#33205,#33206,#33207,#33208,
#33209,#33210,#33211,#33212,#33213,#33214,#33215,#33216,#33217,#33218,#33219,
#33220,#33221,#33222,#33223,#33224,#33225,#33226,#33227,#33228,#33229,#33230,
#33231,#33232,#33233,#33234,#33235,#33236,#33237,#33238,#33239,#33240,#33241,
#33242,#33243,#33244,#33245,#33246,#33247,#33248,#33249,#33250,#33251,#33252,
#33253,#33254,#33255,#33256,#33257,#33258,#33259,#33260,#33261,#33262,#33263,
#33264,#33265,#33266,#33267,#33268,#33269,#33270,#33271,#33272,#33273,#33274,
#33275,#33276,#33277,#33278,#33279,#33280,#33281,#33282,#33283,#33284,#33285,
#33286,#33287,#33288,#33289,#33290,#33291,#33292,#33293,#33294,#33295,#33296,
#33297,#33298,#33299,#33300,#33301,#33302,#33303,#33304,#33305,#33306,#33307,
#33308,#33309,#33310,#33311,#33312,#33313,#33314,#33315,#33316,#33317,#33318,
#33319,#33320,#33321,#33322,#33323,#33324,#33325,#33326,#33327,#33328,#33329,
#33330,#33331,#33332,#33333,#33334,#33335,#33336,#33337,#33338,#33339,#33340,
#33341,#33342,#33343,#33344,#33345,#33346,#33347,#33348,#33349,#33350,#33351,
#33352,#33353,#33354,#33355,#33356,#33357,#33358,#33359,#33360,#33361,#33362,
#33363,#33364,#33365,#33366,#33367,#33368));
#34209=CLOSED_SHELL('',(#33369,#33370,#33371,#33372,#33373,#33374,#33375,
#33376,#33377,#33378,#33379,#33380,#33381,#33382,#33383,#33384,#33385,#33386,
#33387,#33388,#33389,#33390,#33391,#33392,#33393,#33394,#33395,#33396,#33397,
#33398,#33399,#33400,#33401,#33402,#33403,#33404,#33405,#33406,#33407,#33408,
#33409,#33410,#33411,#33412,#33413,#33414,#33415,#33416,#33417,#33418,#33419,
#33420,#33421,#33422,#33423,#33424,#33425,#33426,#33427,#33428,#33429,#33430,
#33431,#33432,#33433,#33434,#33435,#33436,#33437,#33438,#33439,#33440,#33441,
#33442,#33443,#33444,#33445,#33446,#33447,#33448,#33449,#33450,#33451,#33452,
#33453,#33454,#33455,#33456,#33457,#33458,#33459,#33460,#33461,#33462,#33463,
#33464,#33465,#33466,#33467,#33468,#33469,#33470,#33471,#33472,#33473,#33474,
#33475,#33476,#33477,#33478,#33479,#33480,#33481,#33482,#33483,#33484,#33485,
#33486,#33487,#33488,#33489,#33490,#33491,#33492,#33493,#33494,#33495,#33496,
#33497,#33498,#33499,#33500,#33501,#33502));
#34210=CLOSED_SHELL('',(#33503,#33504,#33505,#33506,#33507,#33508,#33509,
#33510,#33511,#33512,#33513,#33514,#33515,#33516,#33517,#33518));
#34211=CLOSED_SHELL('',(#33519,#33520,#33521,#33522,#33523,#33524,#33525,
#33526));
#34212=CLOSED_SHELL('',(#33527,#33528,#33529,#33530,#33531,#33532,#33533,
#33534,#33535,#33536,#33537,#33538,#33539,#33540,#33541,#33542,#33543,#33544,
#33545,#33546,#33547,#33548,#33549,#33550,#33551,#33552,#33553,#33554,#33555,
#33556,#33557,#33558,#33559,#33560,#33561,#33562,#33563,#33564,#33565,#33566,
#33567,#33568,#33569,#33570,#33571,#33572,#33573,#33574,#33575,#33576,#33577,
#33578,#33579,#33580,#33581,#33582,#33583,#33584,#33585,#33586,#33587,#33588,
#33589,#33590,#33591,#33592,#33593,#33594,#33595,#33596,#33597,#33598,#33599,
#33600,#33601,#33602,#33603,#33604,#33605,#33606,#33607,#33608,#33609,#33610,
#33611,#33612,#33613,#33614,#33615,#33616,#33617,#33618,#33619,#33620,#33621,
#33622,#33623,#33624,#33625,#33626,#33627,#33628,#33629,#33630,#33631,#33632,
#33633,#33634,#33635,#33636,#33637,#33638,#33639,#33640,#33641,#33642,#33643,
#33644,#33645,#33646,#33647,#33648,#33649,#33650));
#34213=CLOSED_SHELL('',(#33651,#33652,#33653,#33654,#33655,#33656,#33657,
#33658));
#34214=CLOSED_SHELL('',(#33659,#33660,#33661,#33662,#33663,#33664,#33665,
#33666,#33667,#33668,#33669,#33670,#33671,#33672,#33673,#33674,#33675,#33676,
#33677,#33678,#33679,#33680,#33681,#33682,#33683,#33684,#33685,#33686,#33687,
#33688,#33689,#33690,#33691,#33692,#33693,#33694,#33695,#33696,#33697,#33698,
#33699,#33700,#33701,#33702,#33703,#33704,#33705,#33706,#33707,#33708,#33709,
#33710,#33711,#33712,#33713,#33714,#33715,#33716,#33717,#33718,#33719,#33720,
#33721,#33722,#33723,#33724,#33725,#33726,#33727,#33728,#33729,#33730,#33731,
#33732,#33733,#33734,#33735,#33736,#33737,#33738,#33739,#33740,#33741,#33742,
#33743,#33744,#33745,#33746,#33747,#33748,#33749,#33750,#33751,#33752,#33753,
#33754,#33755,#33756,#33757,#33758,#33759,#33760,#33761,#33762,#33763,#33764,
#33765,#33766,#33767,#33768,#33769,#33770,#33771,#33772));
#34215=CLOSED_SHELL('',(#33773,#33774,#33775,#33776,#33777,#33778,#33779,
#33780,#33781,#33782,#33783));
#34216=CLOSED_SHELL('',(#33784,#33785,#33786,#33787,#33788,#33789,#33790,
#33791,#33792,#33793,#33794,#33795,#33796,#33797,#33798,#33799,#33800,#33801,
#33802,#33803,#33804,#33805,#33806,#33807,#33808,#33809,#33810,#33811,#33812,
#33813,#33814,#33815,#33816,#33817,#33818,#33819,#33820,#33821,#33822,#33823,
#33824,#33825,#33826,#33827,#33828,#33829,#33830,#33831,#33832,#33833,#33834,
#33835,#33836,#33837,#33838,#33839,#33840,#33841,#33842,#33843,#33844,#33845,
#33846,#33847,#33848,#33849,#33850,#33851,#33852,#33853,#33854,#33855,#33856,
#33857,#33858,#33859,#33860,#33861,#33862,#33863,#33864,#33865,#33866,#33867,
#33868,#33869,#33870,#33871,#33872,#33873,#33874,#33875,#33876,#33877,#33878,
#33879,#33880,#33881,#33882,#33883,#33884,#33885,#33886,#33887,#33888,#33889,
#33890,#33891,#33892,#33893,#33894,#33895));
#34217=CLOSED_SHELL('',(#33896,#33897,#33898,#33899,#33900,#33901,#33902,
#33903,#33904,#33905,#33906,#33907,#33908,#33909,#33910,#33911,#33912));
#34218=CLOSED_SHELL('',(#33913,#33914,#33915,#33916,#33917,#33918,#33919,
#33920,#33921,#33922,#33923,#33924,#33925,#33926,#33927,#33928,#33929,#33930,
#33931,#33932,#33933,#33934,#33935));
#34219=CLOSED_SHELL('',(#33936,#33937,#33938,#33939,#33940,#33941,#33942,
#33943,#33944,#33945,#33946,#33947,#33948,#33949,#33950,#33951,#33952,#33953,
#33954,#33955,#33956,#33957,#33958,#33959,#33960,#33961,#33962,#33963,#33964,
#33965,#33966,#33967,#33968,#33969,#33970,#33971,#33972,#33973,#33974,#33975,
#33976,#33977,#33978,#33979,#33980,#33981,#33982,#33983,#33984,#33985,#33986,
#33987,#33988,#33989,#33990,#33991,#33992,#33993,#33994,#33995,#33996,#33997,
#33998,#33999,#34000,#34001,#34002,#34003,#34004,#34005,#34006,#34007,#34008,
#34009,#34010,#34011,#34012,#34013,#34014,#34015,#34016,#34017,#34018,#34019,
#34020,#34021,#34022,#34023,#34024,#34025,#34026,#34027,#34028,#34029,#34030,
#34031,#34032,#34033,#34034,#34035,#34036,#34037,#34038,#34039,#34040,#34041,
#34042,#34043,#34044,#34045,#34046,#34047,#34048,#34049,#34050,#34051,#34052,
#34053,#34054,#34055,#34056,#34057,#34058,#34059,#34060,#34061,#34062,#34063,
#34064,#34065,#34066,#34067,#34068,#34069,#34070,#34071,#34072,#34073,#34074,
#34075,#34076,#34077,#34078,#34079,#34080,#34081,#34082,#34083,#34084,#34085,
#34086,#34087,#34088,#34089,#34090,#34091,#34092,#34093,#34094,#34095,#34096,
#34097,#34098,#34099,#34100,#34101,#34102,#34103,#34104,#34105,#34106,#34107,
#34108,#34109,#34110,#34111,#34112,#34113,#34114,#34115,#34116,#34117,#34118,
#34119,#34120,#34121,#34122,#34123,#34124,#34125,#34126,#34127,#34128,#34129,
#34130,#34131,#34132,#34133,#34134,#34135,#34136,#34137,#34138,#34139,#34140,
#34141,#34142,#34143,#34144,#34145,#34146,#34147,#34148,#34149,#34150,#34151,
#34152,#34153,#34154,#34155,#34156,#34157,#34158));
#34220=CLOSED_SHELL('',(#34159,#34160,#34161,#34162,#34163,#34164,#34165,
#34166,#34167,#34168,#34169,#34170,#34171,#34172,#34173,#34174,#34175,#34176,
#34177,#34178,#34179,#34180,#34181,#34182,#34183,#34184,#34185,#34186,#34187,
#34188,#34189,#34190,#34191,#34192,#34193,#34194,#34195,#34196,#34197,#34198,
#34199,#34200,#34201,#34202,#34203,#34204,#34205,#34206,#34207));
#34221=DERIVED_UNIT_ELEMENT(#34247,1.);
#34222=DERIVED_UNIT_ELEMENT(#71630,-3.);
#34223=DERIVED_UNIT_ELEMENT(#34247,1.);
#34224=DERIVED_UNIT_ELEMENT(#71630,-3.);
#34225=DERIVED_UNIT_ELEMENT(#34247,1.);
#34226=DERIVED_UNIT_ELEMENT(#71630,-3.);
#34227=DERIVED_UNIT_ELEMENT(#34247,1.);
#34228=DERIVED_UNIT_ELEMENT(#71630,-3.);
#34229=DERIVED_UNIT_ELEMENT(#34247,1.);
#34230=DERIVED_UNIT_ELEMENT(#71630,-3.);
#34231=DERIVED_UNIT_ELEMENT(#34247,1.);
#34232=DERIVED_UNIT_ELEMENT(#71630,-3.);
#34233=DERIVED_UNIT_ELEMENT(#34247,1.);
#34234=DERIVED_UNIT_ELEMENT(#71630,-3.);
#34235=DERIVED_UNIT_ELEMENT(#34247,1.);
#34236=DERIVED_UNIT_ELEMENT(#71630,-3.);
#34237=DERIVED_UNIT_ELEMENT(#34247,1.);
#34238=DERIVED_UNIT_ELEMENT(#71630,-3.);
#34239=DERIVED_UNIT_ELEMENT(#34247,1.);
#34240=DERIVED_UNIT_ELEMENT(#71630,-3.);
#34241=DERIVED_UNIT_ELEMENT(#34247,1.);
#34242=DERIVED_UNIT_ELEMENT(#71630,-3.);
#34243=DERIVED_UNIT_ELEMENT(#34247,1.);
#34244=DERIVED_UNIT_ELEMENT(#71630,-3.);
#34245=DERIVED_UNIT_ELEMENT(#34247,1.);
#34246=DERIVED_UNIT_ELEMENT(#71630,-3.);
#34247=(
MASS_UNIT()
NAMED_UNIT(*)
SI_UNIT(.KILO.,.GRAM.)
);
#34248=DERIVED_UNIT((#34221,#34222));
#34249=DERIVED_UNIT((#34223,#34224));
#34250=DERIVED_UNIT((#34225,#34226));
#34251=DERIVED_UNIT((#34227,#34228));
#34252=DERIVED_UNIT((#34229,#34230));
#34253=DERIVED_UNIT((#34231,#34232));
#34254=DERIVED_UNIT((#34233,#34234));
#34255=DERIVED_UNIT((#34235,#34236));
#34256=DERIVED_UNIT((#34237,#34238));
#34257=DERIVED_UNIT((#34239,#34240));
#34258=DERIVED_UNIT((#34241,#34242));
#34259=DERIVED_UNIT((#34243,#34244));
#34260=DERIVED_UNIT((#34245,#34246));
#34261=MEASURE_REPRESENTATION_ITEM('density measure',
POSITIVE_RATIO_MEASURE(7850.),#34248);
#34262=MEASURE_REPRESENTATION_ITEM('density measure',
POSITIVE_RATIO_MEASURE(7850.),#34249);
#34263=MEASURE_REPRESENTATION_ITEM('density measure',
POSITIVE_RATIO_MEASURE(7850.),#34250);
#34264=MEASURE_REPRESENTATION_ITEM('density measure',
POSITIVE_RATIO_MEASURE(7850.),#34251);
#34265=MEASURE_REPRESENTATION_ITEM('density measure',
POSITIVE_RATIO_MEASURE(7850.),#34252);
#34266=MEASURE_REPRESENTATION_ITEM('density measure',
POSITIVE_RATIO_MEASURE(7850.),#34253);
#34267=MEASURE_REPRESENTATION_ITEM('density measure',
POSITIVE_RATIO_MEASURE(7850.),#34254);
#34268=MEASURE_REPRESENTATION_ITEM('density measure',
POSITIVE_RATIO_MEASURE(7850.),#34255);
#34269=MEASURE_REPRESENTATION_ITEM('density measure',
POSITIVE_RATIO_MEASURE(7850.),#34256);
#34270=MEASURE_REPRESENTATION_ITEM('density measure',
POSITIVE_RATIO_MEASURE(7850.),#34257);
#34271=MEASURE_REPRESENTATION_ITEM('density measure',
POSITIVE_RATIO_MEASURE(7850.),#34258);
#34272=MEASURE_REPRESENTATION_ITEM('density measure',
POSITIVE_RATIO_MEASURE(7850.),#34259);
#34273=MEASURE_REPRESENTATION_ITEM('density measure',
POSITIVE_RATIO_MEASURE(7850.),#34260);
#34274=PROPERTY_DEFINITION_REPRESENTATION(#34339,#34300);
#34275=PROPERTY_DEFINITION_REPRESENTATION(#34340,#34301);
#34276=PROPERTY_DEFINITION_REPRESENTATION(#34341,#34302);
#34277=PROPERTY_DEFINITION_REPRESENTATION(#34342,#34303);
#34278=PROPERTY_DEFINITION_REPRESENTATION(#34343,#34304);
#34279=PROPERTY_DEFINITION_REPRESENTATION(#34344,#34305);
#34280=PROPERTY_DEFINITION_REPRESENTATION(#34345,#34306);
#34281=PROPERTY_DEFINITION_REPRESENTATION(#34346,#34307);
#34282=PROPERTY_DEFINITION_REPRESENTATION(#34347,#34308);
#34283=PROPERTY_DEFINITION_REPRESENTATION(#34348,#34309);
#34284=PROPERTY_DEFINITION_REPRESENTATION(#34349,#34310);
#34285=PROPERTY_DEFINITION_REPRESENTATION(#34350,#34311);
#34286=PROPERTY_DEFINITION_REPRESENTATION(#34351,#34312);
#34287=PROPERTY_DEFINITION_REPRESENTATION(#34352,#34313);
#34288=PROPERTY_DEFINITION_REPRESENTATION(#34353,#34314);
#34289=PROPERTY_DEFINITION_REPRESENTATION(#34354,#34315);
#34290=PROPERTY_DEFINITION_REPRESENTATION(#34355,#34316);
#34291=PROPERTY_DEFINITION_REPRESENTATION(#34356,#34317);
#34292=PROPERTY_DEFINITION_REPRESENTATION(#34357,#34318);
#34293=PROPERTY_DEFINITION_REPRESENTATION(#34358,#34319);
#34294=PROPERTY_DEFINITION_REPRESENTATION(#34359,#34320);
#34295=PROPERTY_DEFINITION_REPRESENTATION(#34360,#34321);
#34296=PROPERTY_DEFINITION_REPRESENTATION(#34361,#34322);
#34297=PROPERTY_DEFINITION_REPRESENTATION(#34362,#34323);
#34298=PROPERTY_DEFINITION_REPRESENTATION(#34363,#34324);
#34299=PROPERTY_DEFINITION_REPRESENTATION(#34364,#34325);
#34300=REPRESENTATION('material name',(#34326),#71615);
#34301=REPRESENTATION('density',(#34261),#71615);
#34302=REPRESENTATION('material name',(#34327),#71616);
#34303=REPRESENTATION('density',(#34262),#71616);
#34304=REPRESENTATION('material name',(#34328),#71617);
#34305=REPRESENTATION('density',(#34263),#71617);
#34306=REPRESENTATION('material name',(#34329),#71618);
#34307=REPRESENTATION('density',(#34264),#71618);
#34308=REPRESENTATION('material name',(#34330),#71619);
#34309=REPRESENTATION('density',(#34265),#71619);
#34310=REPRESENTATION('material name',(#34331),#71620);
#34311=REPRESENTATION('density',(#34266),#71620);
#34312=REPRESENTATION('material name',(#34332),#71621);
#34313=REPRESENTATION('density',(#34267),#71621);
#34314=REPRESENTATION('material name',(#34333),#71622);
#34315=REPRESENTATION('density',(#34268),#71622);
#34316=REPRESENTATION('material name',(#34334),#71623);
#34317=REPRESENTATION('density',(#34269),#71623);
#34318=REPRESENTATION('material name',(#34335),#71624);
#34319=REPRESENTATION('density',(#34270),#71624);
#34320=REPRESENTATION('material name',(#34336),#71625);
#34321=REPRESENTATION('density',(#34271),#71625);
#34322=REPRESENTATION('material name',(#34337),#71626);
#34323=REPRESENTATION('density',(#34272),#71626);
#34324=REPRESENTATION('material name',(#34338),#71627);
#34325=REPRESENTATION('density',(#34273),#71627);
#34326=DESCRIPTIVE_REPRESENTATION_ITEM('Steel','Steel');
#34327=DESCRIPTIVE_REPRESENTATION_ITEM('Steel','Steel');
#34328=DESCRIPTIVE_REPRESENTATION_ITEM('Steel','Steel');
#34329=DESCRIPTIVE_REPRESENTATION_ITEM('Steel','Steel');
#34330=DESCRIPTIVE_REPRESENTATION_ITEM('Steel','Steel');
#34331=DESCRIPTIVE_REPRESENTATION_ITEM('Steel','Steel');
#34332=DESCRIPTIVE_REPRESENTATION_ITEM('Steel','Steel');
#34333=DESCRIPTIVE_REPRESENTATION_ITEM('Steel','Steel');
#34334=DESCRIPTIVE_REPRESENTATION_ITEM('Steel','Steel');
#34335=DESCRIPTIVE_REPRESENTATION_ITEM('Steel','Steel');
#34336=DESCRIPTIVE_REPRESENTATION_ITEM('Steel','Steel');
#34337=DESCRIPTIVE_REPRESENTATION_ITEM('Steel','Steel');
#34338=DESCRIPTIVE_REPRESENTATION_ITEM('Steel','Steel');
#34339=PROPERTY_DEFINITION('material property','material name',#71698);
#34340=PROPERTY_DEFINITION('material property','density of part',#71698);
#34341=PROPERTY_DEFINITION('material property','material name',#71699);
#34342=PROPERTY_DEFINITION('material property','density of part',#71699);
#34343=PROPERTY_DEFINITION('material property','material name',#71700);
#34344=PROPERTY_DEFINITION('material property','density of part',#71700);
#34345=PROPERTY_DEFINITION('material property','material name',#71701);
#34346=PROPERTY_DEFINITION('material property','density of part',#71701);
#34347=PROPERTY_DEFINITION('material property','material name',#71702);
#34348=PROPERTY_DEFINITION('material property','density of part',#71702);
#34349=PROPERTY_DEFINITION('material property','material name',#71703);
#34350=PROPERTY_DEFINITION('material property','density of part',#71703);
#34351=PROPERTY_DEFINITION('material property','material name',#71704);
#34352=PROPERTY_DEFINITION('material property','density of part',#71704);
#34353=PROPERTY_DEFINITION('material property','material name',#71705);
#34354=PROPERTY_DEFINITION('material property','density of part',#71705);
#34355=PROPERTY_DEFINITION('material property','material name',#71706);
#34356=PROPERTY_DEFINITION('material property','density of part',#71706);
#34357=PROPERTY_DEFINITION('material property','material name',#71707);
#34358=PROPERTY_DEFINITION('material property','density of part',#71707);
#34359=PROPERTY_DEFINITION('material property','material name',#71708);
#34360=PROPERTY_DEFINITION('material property','density of part',#71708);
#34361=PROPERTY_DEFINITION('material property','material name',#71709);
#34362=PROPERTY_DEFINITION('material property','density of part',#71709);
#34363=PROPERTY_DEFINITION('material property','material name',#71710);
#34364=PROPERTY_DEFINITION('material property','density of part',#71710);
#34365=AXIS2_PLACEMENT_3D('',#47303,#37661,#37662);
#34366=AXIS2_PLACEMENT_3D('',#47304,#37663,#37664);
#34367=AXIS2_PLACEMENT_3D('',#47305,#37665,#37666);
#34368=AXIS2_PLACEMENT_3D('',#47308,#37667,#37668);
#34369=AXIS2_PLACEMENT_3D('',#47309,#37669,#37670);
#34370=AXIS2_PLACEMENT_3D('',#47313,#37672,#37673);
#34371=AXIS2_PLACEMENT_3D('',#47314,#37674,#37675);
#34372=AXIS2_PLACEMENT_3D('',#47315,#37676,#37677);
#34373=AXIS2_PLACEMENT_3D('',#47319,#37679,#37680);
#34374=AXIS2_PLACEMENT_3D('',#47320,#37681,#37682);
#34375=AXIS2_PLACEMENT_3D('',#47321,#37683,#37684);
#34376=AXIS2_PLACEMENT_3D('',#47323,#37685,#37686);
#34377=AXIS2_PLACEMENT_3D('',#47325,#37688,#37689);
#34378=AXIS2_PLACEMENT_3D('',#47328,#37691,#37692);
#34379=AXIS2_PLACEMENT_3D('',#47329,#37693,#37694);
#34380=AXIS2_PLACEMENT_3D('',#47331,#37695,#37696);
#34381=AXIS2_PLACEMENT_3D('',#47332,#37697,#37698);
#34382=AXIS2_PLACEMENT_3D('',#47334,#37699,#37700);
#34383=AXIS2_PLACEMENT_3D('',#47338,#37702,#37703);
#34384=AXIS2_PLACEMENT_3D('',#47339,#37704,#37705);
#34385=AXIS2_PLACEMENT_3D('',#47340,#37706,#37707);
#34386=AXIS2_PLACEMENT_3D('',#47342,#37708,#37709);
#34387=AXIS2_PLACEMENT_3D('',#47344,#37711,#37712);
#34388=AXIS2_PLACEMENT_3D('',#47346,#37713,#37714);
#34389=AXIS2_PLACEMENT_3D('',#47347,#37715,#37716);
#34390=AXIS2_PLACEMENT_3D('',#47349,#37717,#37718);
#34391=AXIS2_PLACEMENT_3D('',#47353,#37720,#37721);
#34392=AXIS2_PLACEMENT_3D('',#47354,#37722,#37723);
#34393=AXIS2_PLACEMENT_3D('',#47355,#37724,#37725);
#34394=AXIS2_PLACEMENT_3D('',#47359,#37727,#37728);
#34395=AXIS2_PLACEMENT_3D('',#47360,#37729,#37730);
#34396=AXIS2_PLACEMENT_3D('',#47361,#37731,#37732);
#34397=AXIS2_PLACEMENT_3D('',#47363,#37733,#37734);
#34398=AXIS2_PLACEMENT_3D('',#47364,#37735,#37736);
#34399=AXIS2_PLACEMENT_3D('',#47368,#37738,#37739);
#34400=AXIS2_PLACEMENT_3D('',#47369,#37740,#37741);
#34401=AXIS2_PLACEMENT_3D('',#47370,#37742,#37743);
#34402=AXIS2_PLACEMENT_3D('',#47373,#37745,#37746);
#34403=AXIS2_PLACEMENT_3D('',#47374,#37747,#37748);
#34404=AXIS2_PLACEMENT_3D('',#47377,#37749,#37750);
#34405=AXIS2_PLACEMENT_3D('',#47378,#37751,#37752);
#34406=AXIS2_PLACEMENT_3D('',#47382,#37754,#37755);
#34407=AXIS2_PLACEMENT_3D('',#47383,#37756,#37757);
#34408=AXIS2_PLACEMENT_3D('',#47384,#37758,#37759);
#34409=AXIS2_PLACEMENT_3D('',#47388,#37761,#37762);
#34410=AXIS2_PLACEMENT_3D('',#47389,#37763,#37764);
#34411=AXIS2_PLACEMENT_3D('',#47390,#37765,#37766);
#34412=AXIS2_PLACEMENT_3D('',#47392,#37767,#37768);
#34413=AXIS2_PLACEMENT_3D('',#47394,#37770,#37771);
#34414=AXIS2_PLACEMENT_3D('',#47398,#37773,#37774);
#34415=AXIS2_PLACEMENT_3D('',#47399,#37775,#37776);
#34416=AXIS2_PLACEMENT_3D('',#47400,#37777,#37778);
#34417=AXIS2_PLACEMENT_3D('',#47404,#37780,#37781);
#34418=AXIS2_PLACEMENT_3D('',#47405,#37782,#37783);
#34419=AXIS2_PLACEMENT_3D('',#47406,#37784,#37785);
#34420=AXIS2_PLACEMENT_3D('',#47410,#37787,#37788);
#34421=AXIS2_PLACEMENT_3D('',#47411,#37789,#37790);
#34422=AXIS2_PLACEMENT_3D('',#47412,#37791,#37792);
#34423=AXIS2_PLACEMENT_3D('',#47416,#37794,#37795);
#34424=AXIS2_PLACEMENT_3D('',#47417,#37796,#37797);
#34425=AXIS2_PLACEMENT_3D('',#47418,#37798,#37799);
#34426=AXIS2_PLACEMENT_3D('',#47422,#37801,#37802);
#34427=AXIS2_PLACEMENT_3D('',#47423,#37803,#37804);
#34428=AXIS2_PLACEMENT_3D('',#47424,#37805,#37806);
#34429=AXIS2_PLACEMENT_3D('',#47428,#37808,#37809);
#34430=AXIS2_PLACEMENT_3D('',#47430,#37810,#37811);
#34431=AXIS2_PLACEMENT_3D('',#47434,#37813,#37814);
#34432=AXIS2_PLACEMENT_3D('',#47436,#37815,#37816);
#34433=AXIS2_PLACEMENT_3D('',#47439,#37818,#37819);
#34434=AXIS2_PLACEMENT_3D('',#47441,#37820,#37821);
#34435=AXIS2_PLACEMENT_3D('',#47443,#37822,#37823);
#34436=AXIS2_PLACEMENT_3D('',#47447,#37825,#37826);
#34437=AXIS2_PLACEMENT_3D('',#47448,#37827,#37828);
#34438=AXIS2_PLACEMENT_3D('',#47453,#37830,#37831);
#34439=AXIS2_PLACEMENT_3D('',#47455,#37832,#37833);
#34440=AXIS2_PLACEMENT_3D('',#47457,#37834,#37835);
#34441=AXIS2_PLACEMENT_3D('',#47461,#37837,#37838);
#34442=AXIS2_PLACEMENT_3D('',#47463,#37839,#37840);
#34443=AXIS2_PLACEMENT_3D('',#47464,#37841,#37842);
#34444=AXIS2_PLACEMENT_3D('',#47469,#37844,#37845);
#34445=AXIS2_PLACEMENT_3D('',#47471,#37846,#37847);
#34446=AXIS2_PLACEMENT_3D('',#47473,#37848,#37849);
#34447=AXIS2_PLACEMENT_3D('',#47477,#37851,#37852);
#34448=AXIS2_PLACEMENT_3D('',#47479,#37853,#37854);
#34449=AXIS2_PLACEMENT_3D('',#47480,#37855,#37856);
#34450=AXIS2_PLACEMENT_3D('',#47485,#37858,#37859);
#34451=AXIS2_PLACEMENT_3D('',#47487,#37860,#37861);
#34452=AXIS2_PLACEMENT_3D('',#47489,#37862,#37863);
#34453=AXIS2_PLACEMENT_3D('',#47493,#37865,#37866);
#34454=AXIS2_PLACEMENT_3D('',#47495,#37867,#37868);
#34455=AXIS2_PLACEMENT_3D('',#47496,#37869,#37870);
#34456=AXIS2_PLACEMENT_3D('',#47501,#37872,#37873);
#34457=AXIS2_PLACEMENT_3D('',#47503,#37874,#37875);
#34458=AXIS2_PLACEMENT_3D('',#47505,#37876,#37877);
#34459=AXIS2_PLACEMENT_3D('',#47509,#37879,#37880);
#34460=AXIS2_PLACEMENT_3D('',#47511,#37881,#37882);
#34461=AXIS2_PLACEMENT_3D('',#47512,#37883,#37884);
#34462=AXIS2_PLACEMENT_3D('',#47517,#37886,#37887);
#34463=AXIS2_PLACEMENT_3D('',#47519,#37888,#37889);
#34464=AXIS2_PLACEMENT_3D('',#47521,#37890,#37891);
#34465=AXIS2_PLACEMENT_3D('',#47525,#37893,#37894);
#34466=AXIS2_PLACEMENT_3D('',#47527,#37895,#37896);
#34467=AXIS2_PLACEMENT_3D('',#47528,#37897,#37898);
#34468=AXIS2_PLACEMENT_3D('',#47533,#37900,#37901);
#34469=AXIS2_PLACEMENT_3D('',#47535,#37902,#37903);
#34470=AXIS2_PLACEMENT_3D('',#47537,#37904,#37905);
#34471=AXIS2_PLACEMENT_3D('',#47541,#37907,#37908);
#34472=AXIS2_PLACEMENT_3D('',#47543,#37909,#37910);
#34473=AXIS2_PLACEMENT_3D('',#47544,#37911,#37912);
#34474=AXIS2_PLACEMENT_3D('',#47549,#37914,#37915);
#34475=AXIS2_PLACEMENT_3D('',#47551,#37916,#37917);
#34476=AXIS2_PLACEMENT_3D('',#47553,#37918,#37919);
#34477=AXIS2_PLACEMENT_3D('',#47557,#37921,#37922);
#34478=AXIS2_PLACEMENT_3D('',#47559,#37923,#37924);
#34479=AXIS2_PLACEMENT_3D('',#47560,#37925,#37926);
#34480=AXIS2_PLACEMENT_3D('',#47565,#37928,#37929);
#34481=AXIS2_PLACEMENT_3D('',#47567,#37930,#37931);
#34482=AXIS2_PLACEMENT_3D('',#47569,#37932,#37933);
#34483=AXIS2_PLACEMENT_3D('',#47573,#37935,#37936);
#34484=AXIS2_PLACEMENT_3D('',#47575,#37937,#37938);
#34485=AXIS2_PLACEMENT_3D('',#47576,#37939,#37940);
#34486=AXIS2_PLACEMENT_3D('',#47581,#37942,#37943);
#34487=AXIS2_PLACEMENT_3D('',#47583,#37944,#37945);
#34488=AXIS2_PLACEMENT_3D('',#47585,#37946,#37947);
#34489=AXIS2_PLACEMENT_3D('',#47589,#37949,#37950);
#34490=AXIS2_PLACEMENT_3D('',#47591,#37951,#37952);
#34491=AXIS2_PLACEMENT_3D('',#47592,#37953,#37954);
#34492=AXIS2_PLACEMENT_3D('',#47597,#37956,#37957);
#34493=AXIS2_PLACEMENT_3D('',#47599,#37958,#37959);
#34494=AXIS2_PLACEMENT_3D('',#47601,#37960,#37961);
#34495=AXIS2_PLACEMENT_3D('',#47605,#37963,#37964);
#34496=AXIS2_PLACEMENT_3D('',#47607,#37965,#37966);
#34497=AXIS2_PLACEMENT_3D('',#47608,#37967,#37968);
#34498=AXIS2_PLACEMENT_3D('',#47613,#37970,#37971);
#34499=AXIS2_PLACEMENT_3D('',#47615,#37972,#37973);
#34500=AXIS2_PLACEMENT_3D('',#47617,#37974,#37975);
#34501=AXIS2_PLACEMENT_3D('',#47621,#37977,#37978);
#34502=AXIS2_PLACEMENT_3D('',#47623,#37979,#37980);
#34503=AXIS2_PLACEMENT_3D('',#47624,#37981,#37982);
#34504=AXIS2_PLACEMENT_3D('',#47629,#37984,#37985);
#34505=AXIS2_PLACEMENT_3D('',#47631,#37986,#37987);
#34506=AXIS2_PLACEMENT_3D('',#47633,#37988,#37989);
#34507=AXIS2_PLACEMENT_3D('',#47637,#37991,#37992);
#34508=AXIS2_PLACEMENT_3D('',#47639,#37993,#37994);
#34509=AXIS2_PLACEMENT_3D('',#47640,#37995,#37996);
#34510=AXIS2_PLACEMENT_3D('',#47645,#37998,#37999);
#34511=AXIS2_PLACEMENT_3D('',#47647,#38000,#38001);
#34512=AXIS2_PLACEMENT_3D('',#47649,#38002,#38003);
#34513=AXIS2_PLACEMENT_3D('',#47653,#38005,#38006);
#34514=AXIS2_PLACEMENT_3D('',#47655,#38007,#38008);
#34515=AXIS2_PLACEMENT_3D('',#47656,#38009,#38010);
#34516=AXIS2_PLACEMENT_3D('',#47661,#38012,#38013);
#34517=AXIS2_PLACEMENT_3D('',#47663,#38014,#38015);
#34518=AXIS2_PLACEMENT_3D('',#47665,#38016,#38017);
#34519=AXIS2_PLACEMENT_3D('',#47669,#38019,#38020);
#34520=AXIS2_PLACEMENT_3D('',#47671,#38021,#38022);
#34521=AXIS2_PLACEMENT_3D('',#47672,#38023,#38024);
#34522=AXIS2_PLACEMENT_3D('',#47677,#38026,#38027);
#34523=AXIS2_PLACEMENT_3D('',#47679,#38028,#38029);
#34524=AXIS2_PLACEMENT_3D('',#47681,#38030,#38031);
#34525=AXIS2_PLACEMENT_3D('',#47685,#38033,#38034);
#34526=AXIS2_PLACEMENT_3D('',#47687,#38035,#38036);
#34527=AXIS2_PLACEMENT_3D('',#47688,#38037,#38038);
#34528=AXIS2_PLACEMENT_3D('',#47693,#38040,#38041);
#34529=AXIS2_PLACEMENT_3D('',#47695,#38042,#38043);
#34530=AXIS2_PLACEMENT_3D('',#47697,#38044,#38045);
#34531=AXIS2_PLACEMENT_3D('',#47701,#38047,#38048);
#34532=AXIS2_PLACEMENT_3D('',#47703,#38049,#38050);
#34533=AXIS2_PLACEMENT_3D('',#47704,#38051,#38052);
#34534=AXIS2_PLACEMENT_3D('',#47709,#38054,#38055);
#34535=AXIS2_PLACEMENT_3D('',#47711,#38056,#38057);
#34536=AXIS2_PLACEMENT_3D('',#47713,#38058,#38059);
#34537=AXIS2_PLACEMENT_3D('',#47717,#38061,#38062);
#34538=AXIS2_PLACEMENT_3D('',#47719,#38063,#38064);
#34539=AXIS2_PLACEMENT_3D('',#47720,#38065,#38066);
#34540=AXIS2_PLACEMENT_3D('',#47725,#38068,#38069);
#34541=AXIS2_PLACEMENT_3D('',#47727,#38070,#38071);
#34542=AXIS2_PLACEMENT_3D('',#47729,#38072,#38073);
#34543=AXIS2_PLACEMENT_3D('',#47733,#38075,#38076);
#34544=AXIS2_PLACEMENT_3D('',#47735,#38077,#38078);
#34545=AXIS2_PLACEMENT_3D('',#47736,#38079,#38080);
#34546=AXIS2_PLACEMENT_3D('',#47741,#38082,#38083);
#34547=AXIS2_PLACEMENT_3D('',#47743,#38084,#38085);
#34548=AXIS2_PLACEMENT_3D('',#47745,#38086,#38087);
#34549=AXIS2_PLACEMENT_3D('',#47749,#38089,#38090);
#34550=AXIS2_PLACEMENT_3D('',#47751,#38091,#38092);
#34551=AXIS2_PLACEMENT_3D('',#47752,#38093,#38094);
#34552=AXIS2_PLACEMENT_3D('',#47757,#38096,#38097);
#34553=AXIS2_PLACEMENT_3D('',#47759,#38098,#38099);
#34554=AXIS2_PLACEMENT_3D('',#47761,#38100,#38101);
#34555=AXIS2_PLACEMENT_3D('',#47765,#38103,#38104);
#34556=AXIS2_PLACEMENT_3D('',#47767,#38105,#38106);
#34557=AXIS2_PLACEMENT_3D('',#47768,#38107,#38108);
#34558=AXIS2_PLACEMENT_3D('',#47773,#38110,#38111);
#34559=AXIS2_PLACEMENT_3D('',#47775,#38112,#38113);
#34560=AXIS2_PLACEMENT_3D('',#47777,#38114,#38115);
#34561=AXIS2_PLACEMENT_3D('',#47781,#38117,#38118);
#34562=AXIS2_PLACEMENT_3D('',#47783,#38119,#38120);
#34563=AXIS2_PLACEMENT_3D('',#47784,#38121,#38122);
#34564=AXIS2_PLACEMENT_3D('',#47789,#38124,#38125);
#34565=AXIS2_PLACEMENT_3D('',#47791,#38126,#38127);
#34566=AXIS2_PLACEMENT_3D('',#47793,#38128,#38129);
#34567=AXIS2_PLACEMENT_3D('',#47797,#38131,#38132);
#34568=AXIS2_PLACEMENT_3D('',#47799,#38133,#38134);
#34569=AXIS2_PLACEMENT_3D('',#47800,#38135,#38136);
#34570=AXIS2_PLACEMENT_3D('',#47805,#38138,#38139);
#34571=AXIS2_PLACEMENT_3D('',#47807,#38140,#38141);
#34572=AXIS2_PLACEMENT_3D('',#47809,#38142,#38143);
#34573=AXIS2_PLACEMENT_3D('',#47813,#38145,#38146);
#34574=AXIS2_PLACEMENT_3D('',#47815,#38147,#38148);
#34575=AXIS2_PLACEMENT_3D('',#47816,#38149,#38150);
#34576=AXIS2_PLACEMENT_3D('',#47821,#38152,#38153);
#34577=AXIS2_PLACEMENT_3D('',#47823,#38154,#38155);
#34578=AXIS2_PLACEMENT_3D('',#47825,#38156,#38157);
#34579=AXIS2_PLACEMENT_3D('',#47829,#38159,#38160);
#34580=AXIS2_PLACEMENT_3D('',#47831,#38161,#38162);
#34581=AXIS2_PLACEMENT_3D('',#47832,#38163,#38164);
#34582=AXIS2_PLACEMENT_3D('',#47837,#38166,#38167);
#34583=AXIS2_PLACEMENT_3D('',#47839,#38168,#38169);
#34584=AXIS2_PLACEMENT_3D('',#47841,#38170,#38171);
#34585=AXIS2_PLACEMENT_3D('',#47845,#38173,#38174);
#34586=AXIS2_PLACEMENT_3D('',#47847,#38175,#38176);
#34587=AXIS2_PLACEMENT_3D('',#47848,#38177,#38178);
#34588=AXIS2_PLACEMENT_3D('',#47853,#38180,#38181);
#34589=AXIS2_PLACEMENT_3D('',#47855,#38182,#38183);
#34590=AXIS2_PLACEMENT_3D('',#47857,#38184,#38185);
#34591=AXIS2_PLACEMENT_3D('',#47861,#38187,#38188);
#34592=AXIS2_PLACEMENT_3D('',#47863,#38189,#38190);
#34593=AXIS2_PLACEMENT_3D('',#47864,#38191,#38192);
#34594=AXIS2_PLACEMENT_3D('',#47869,#38194,#38195);
#34595=AXIS2_PLACEMENT_3D('',#47871,#38196,#38197);
#34596=AXIS2_PLACEMENT_3D('',#47873,#38198,#38199);
#34597=AXIS2_PLACEMENT_3D('',#47877,#38201,#38202);
#34598=AXIS2_PLACEMENT_3D('',#47879,#38203,#38204);
#34599=AXIS2_PLACEMENT_3D('',#47880,#38205,#38206);
#34600=AXIS2_PLACEMENT_3D('',#47885,#38208,#38209);
#34601=AXIS2_PLACEMENT_3D('',#47887,#38210,#38211);
#34602=AXIS2_PLACEMENT_3D('',#47889,#38212,#38213);
#34603=AXIS2_PLACEMENT_3D('',#47893,#38215,#38216);
#34604=AXIS2_PLACEMENT_3D('',#47895,#38217,#38218);
#34605=AXIS2_PLACEMENT_3D('',#47896,#38219,#38220);
#34606=AXIS2_PLACEMENT_3D('',#47901,#38222,#38223);
#34607=AXIS2_PLACEMENT_3D('',#47903,#38224,#38225);
#34608=AXIS2_PLACEMENT_3D('',#47905,#38226,#38227);
#34609=AXIS2_PLACEMENT_3D('',#47909,#38229,#38230);
#34610=AXIS2_PLACEMENT_3D('',#47911,#38231,#38232);
#34611=AXIS2_PLACEMENT_3D('',#47912,#38233,#38234);
#34612=AXIS2_PLACEMENT_3D('',#47917,#38236,#38237);
#34613=AXIS2_PLACEMENT_3D('',#47919,#38238,#38239);
#34614=AXIS2_PLACEMENT_3D('',#47921,#38240,#38241);
#34615=AXIS2_PLACEMENT_3D('',#47925,#38243,#38244);
#34616=AXIS2_PLACEMENT_3D('',#47927,#38245,#38246);
#34617=AXIS2_PLACEMENT_3D('',#47928,#38247,#38248);
#34618=AXIS2_PLACEMENT_3D('',#47933,#38250,#38251);
#34619=AXIS2_PLACEMENT_3D('',#47935,#38252,#38253);
#34620=AXIS2_PLACEMENT_3D('',#47937,#38254,#38255);
#34621=AXIS2_PLACEMENT_3D('',#47941,#38257,#38258);
#34622=AXIS2_PLACEMENT_3D('',#47943,#38259,#38260);
#34623=AXIS2_PLACEMENT_3D('',#47944,#38261,#38262);
#34624=AXIS2_PLACEMENT_3D('',#47949,#38264,#38265);
#34625=AXIS2_PLACEMENT_3D('',#47951,#38266,#38267);
#34626=AXIS2_PLACEMENT_3D('',#47953,#38268,#38269);
#34627=AXIS2_PLACEMENT_3D('',#47957,#38271,#38272);
#34628=AXIS2_PLACEMENT_3D('',#47959,#38273,#38274);
#34629=AXIS2_PLACEMENT_3D('',#47960,#38275,#38276);
#34630=AXIS2_PLACEMENT_3D('',#47965,#38278,#38279);
#34631=AXIS2_PLACEMENT_3D('',#47967,#38280,#38281);
#34632=AXIS2_PLACEMENT_3D('',#47969,#38282,#38283);
#34633=AXIS2_PLACEMENT_3D('',#47973,#38285,#38286);
#34634=AXIS2_PLACEMENT_3D('',#47975,#38287,#38288);
#34635=AXIS2_PLACEMENT_3D('',#47976,#38289,#38290);
#34636=AXIS2_PLACEMENT_3D('',#47981,#38292,#38293);
#34637=AXIS2_PLACEMENT_3D('',#47983,#38294,#38295);
#34638=AXIS2_PLACEMENT_3D('',#47985,#38296,#38297);
#34639=AXIS2_PLACEMENT_3D('',#47989,#38299,#38300);
#34640=AXIS2_PLACEMENT_3D('',#47991,#38301,#38302);
#34641=AXIS2_PLACEMENT_3D('',#47992,#38303,#38304);
#34642=AXIS2_PLACEMENT_3D('',#47997,#38306,#38307);
#34643=AXIS2_PLACEMENT_3D('',#47999,#38308,#38309);
#34644=AXIS2_PLACEMENT_3D('',#48001,#38310,#38311);
#34645=AXIS2_PLACEMENT_3D('',#48005,#38313,#38314);
#34646=AXIS2_PLACEMENT_3D('',#48007,#38315,#38316);
#34647=AXIS2_PLACEMENT_3D('',#48008,#38317,#38318);
#34648=AXIS2_PLACEMENT_3D('',#48013,#38320,#38321);
#34649=AXIS2_PLACEMENT_3D('',#48015,#38322,#38323);
#34650=AXIS2_PLACEMENT_3D('',#48017,#38324,#38325);
#34651=AXIS2_PLACEMENT_3D('',#48021,#38327,#38328);
#34652=AXIS2_PLACEMENT_3D('',#48023,#38329,#38330);
#34653=AXIS2_PLACEMENT_3D('',#48024,#38331,#38332);
#34654=AXIS2_PLACEMENT_3D('',#48029,#38334,#38335);
#34655=AXIS2_PLACEMENT_3D('',#48031,#38336,#38337);
#34656=AXIS2_PLACEMENT_3D('',#48033,#38338,#38339);
#34657=AXIS2_PLACEMENT_3D('',#48037,#38341,#38342);
#34658=AXIS2_PLACEMENT_3D('',#48039,#38343,#38344);
#34659=AXIS2_PLACEMENT_3D('',#48040,#38345,#38346);
#34660=AXIS2_PLACEMENT_3D('',#48045,#38348,#38349);
#34661=AXIS2_PLACEMENT_3D('',#48047,#38350,#38351);
#34662=AXIS2_PLACEMENT_3D('',#48049,#38352,#38353);
#34663=AXIS2_PLACEMENT_3D('',#48053,#38355,#38356);
#34664=AXIS2_PLACEMENT_3D('',#48055,#38357,#38358);
#34665=AXIS2_PLACEMENT_3D('',#48056,#38359,#38360);
#34666=AXIS2_PLACEMENT_3D('',#48061,#38362,#38363);
#34667=AXIS2_PLACEMENT_3D('',#48063,#38364,#38365);
#34668=AXIS2_PLACEMENT_3D('',#48065,#38366,#38367);
#34669=AXIS2_PLACEMENT_3D('',#48069,#38369,#38370);
#34670=AXIS2_PLACEMENT_3D('',#48071,#38371,#38372);
#34671=AXIS2_PLACEMENT_3D('',#48072,#38373,#38374);
#34672=AXIS2_PLACEMENT_3D('',#48077,#38376,#38377);
#34673=AXIS2_PLACEMENT_3D('',#48079,#38378,#38379);
#34674=AXIS2_PLACEMENT_3D('',#48081,#38380,#38381);
#34675=AXIS2_PLACEMENT_3D('',#48085,#38383,#38384);
#34676=AXIS2_PLACEMENT_3D('',#48087,#38385,#38386);
#34677=AXIS2_PLACEMENT_3D('',#48088,#38387,#38388);
#34678=AXIS2_PLACEMENT_3D('',#48093,#38390,#38391);
#34679=AXIS2_PLACEMENT_3D('',#48095,#38392,#38393);
#34680=AXIS2_PLACEMENT_3D('',#48097,#38394,#38395);
#34681=AXIS2_PLACEMENT_3D('',#48101,#38397,#38398);
#34682=AXIS2_PLACEMENT_3D('',#48103,#38399,#38400);
#34683=AXIS2_PLACEMENT_3D('',#48104,#38401,#38402);
#34684=AXIS2_PLACEMENT_3D('',#48109,#38404,#38405);
#34685=AXIS2_PLACEMENT_3D('',#48111,#38406,#38407);
#34686=AXIS2_PLACEMENT_3D('',#48113,#38408,#38409);
#34687=AXIS2_PLACEMENT_3D('',#48117,#38411,#38412);
#34688=AXIS2_PLACEMENT_3D('',#48119,#38413,#38414);
#34689=AXIS2_PLACEMENT_3D('',#48120,#38415,#38416);
#34690=AXIS2_PLACEMENT_3D('',#48125,#38418,#38419);
#34691=AXIS2_PLACEMENT_3D('',#48127,#38420,#38421);
#34692=AXIS2_PLACEMENT_3D('',#48129,#38422,#38423);
#34693=AXIS2_PLACEMENT_3D('',#48133,#38425,#38426);
#34694=AXIS2_PLACEMENT_3D('',#48135,#38427,#38428);
#34695=AXIS2_PLACEMENT_3D('',#48136,#38429,#38430);
#34696=AXIS2_PLACEMENT_3D('',#48141,#38432,#38433);
#34697=AXIS2_PLACEMENT_3D('',#48143,#38434,#38435);
#34698=AXIS2_PLACEMENT_3D('',#48145,#38436,#38437);
#34699=AXIS2_PLACEMENT_3D('',#48149,#38439,#38440);
#34700=AXIS2_PLACEMENT_3D('',#48151,#38441,#38442);
#34701=AXIS2_PLACEMENT_3D('',#48152,#38443,#38444);
#34702=AXIS2_PLACEMENT_3D('',#48157,#38446,#38447);
#34703=AXIS2_PLACEMENT_3D('',#48159,#38448,#38449);
#34704=AXIS2_PLACEMENT_3D('',#48161,#38450,#38451);
#34705=AXIS2_PLACEMENT_3D('',#48165,#38453,#38454);
#34706=AXIS2_PLACEMENT_3D('',#48167,#38455,#38456);
#34707=AXIS2_PLACEMENT_3D('',#48168,#38457,#38458);
#34708=AXIS2_PLACEMENT_3D('',#48173,#38460,#38461);
#34709=AXIS2_PLACEMENT_3D('',#48175,#38462,#38463);
#34710=AXIS2_PLACEMENT_3D('',#48177,#38464,#38465);
#34711=AXIS2_PLACEMENT_3D('',#48181,#38467,#38468);
#34712=AXIS2_PLACEMENT_3D('',#48183,#38469,#38470);
#34713=AXIS2_PLACEMENT_3D('',#48184,#38471,#38472);
#34714=AXIS2_PLACEMENT_3D('',#48189,#38474,#38475);
#34715=AXIS2_PLACEMENT_3D('',#48191,#38476,#38477);
#34716=AXIS2_PLACEMENT_3D('',#48193,#38478,#38479);
#34717=AXIS2_PLACEMENT_3D('',#48197,#38481,#38482);
#34718=AXIS2_PLACEMENT_3D('',#48199,#38483,#38484);
#34719=AXIS2_PLACEMENT_3D('',#48200,#38485,#38486);
#34720=AXIS2_PLACEMENT_3D('',#48205,#38488,#38489);
#34721=AXIS2_PLACEMENT_3D('',#48207,#38490,#38491);
#34722=AXIS2_PLACEMENT_3D('',#48209,#38492,#38493);
#34723=AXIS2_PLACEMENT_3D('',#48213,#38495,#38496);
#34724=AXIS2_PLACEMENT_3D('',#48215,#38497,#38498);
#34725=AXIS2_PLACEMENT_3D('',#48216,#38499,#38500);
#34726=AXIS2_PLACEMENT_3D('',#48221,#38502,#38503);
#34727=AXIS2_PLACEMENT_3D('',#48223,#38504,#38505);
#34728=AXIS2_PLACEMENT_3D('',#48225,#38506,#38507);
#34729=AXIS2_PLACEMENT_3D('',#48229,#38509,#38510);
#34730=AXIS2_PLACEMENT_3D('',#48231,#38511,#38512);
#34731=AXIS2_PLACEMENT_3D('',#48232,#38513,#38514);
#34732=AXIS2_PLACEMENT_3D('',#48237,#38516,#38517);
#34733=AXIS2_PLACEMENT_3D('',#48239,#38518,#38519);
#34734=AXIS2_PLACEMENT_3D('',#48241,#38520,#38521);
#34735=AXIS2_PLACEMENT_3D('',#48245,#38523,#38524);
#34736=AXIS2_PLACEMENT_3D('',#48247,#38525,#38526);
#34737=AXIS2_PLACEMENT_3D('',#48248,#38527,#38528);
#34738=AXIS2_PLACEMENT_3D('',#48253,#38530,#38531);
#34739=AXIS2_PLACEMENT_3D('',#48255,#38532,#38533);
#34740=AXIS2_PLACEMENT_3D('',#48257,#38534,#38535);
#34741=AXIS2_PLACEMENT_3D('',#48261,#38537,#38538);
#34742=AXIS2_PLACEMENT_3D('',#48263,#38539,#38540);
#34743=AXIS2_PLACEMENT_3D('',#48264,#38541,#38542);
#34744=AXIS2_PLACEMENT_3D('',#48269,#38544,#38545);
#34745=AXIS2_PLACEMENT_3D('',#48271,#38546,#38547);
#34746=AXIS2_PLACEMENT_3D('',#48273,#38548,#38549);
#34747=AXIS2_PLACEMENT_3D('',#48277,#38551,#38552);
#34748=AXIS2_PLACEMENT_3D('',#48279,#38553,#38554);
#34749=AXIS2_PLACEMENT_3D('',#48280,#38555,#38556);
#34750=AXIS2_PLACEMENT_3D('',#48285,#38558,#38559);
#34751=AXIS2_PLACEMENT_3D('',#48287,#38560,#38561);
#34752=AXIS2_PLACEMENT_3D('',#48289,#38562,#38563);
#34753=AXIS2_PLACEMENT_3D('',#48293,#38565,#38566);
#34754=AXIS2_PLACEMENT_3D('',#48295,#38567,#38568);
#34755=AXIS2_PLACEMENT_3D('',#48296,#38569,#38570);
#34756=AXIS2_PLACEMENT_3D('',#48301,#38572,#38573);
#34757=AXIS2_PLACEMENT_3D('',#48303,#38574,#38575);
#34758=AXIS2_PLACEMENT_3D('',#48305,#38576,#38577);
#34759=AXIS2_PLACEMENT_3D('',#48309,#38579,#38580);
#34760=AXIS2_PLACEMENT_3D('',#48311,#38581,#38582);
#34761=AXIS2_PLACEMENT_3D('',#48312,#38583,#38584);
#34762=AXIS2_PLACEMENT_3D('',#48317,#38586,#38587);
#34763=AXIS2_PLACEMENT_3D('',#48319,#38588,#38589);
#34764=AXIS2_PLACEMENT_3D('',#48321,#38590,#38591);
#34765=AXIS2_PLACEMENT_3D('',#48325,#38593,#38594);
#34766=AXIS2_PLACEMENT_3D('',#48327,#38595,#38596);
#34767=AXIS2_PLACEMENT_3D('',#48328,#38597,#38598);
#34768=AXIS2_PLACEMENT_3D('',#48333,#38600,#38601);
#34769=AXIS2_PLACEMENT_3D('',#48335,#38602,#38603);
#34770=AXIS2_PLACEMENT_3D('',#48337,#38604,#38605);
#34771=AXIS2_PLACEMENT_3D('',#48341,#38607,#38608);
#34772=AXIS2_PLACEMENT_3D('',#48343,#38609,#38610);
#34773=AXIS2_PLACEMENT_3D('',#48344,#38611,#38612);
#34774=AXIS2_PLACEMENT_3D('',#48349,#38614,#38615);
#34775=AXIS2_PLACEMENT_3D('',#48351,#38616,#38617);
#34776=AXIS2_PLACEMENT_3D('',#48353,#38618,#38619);
#34777=AXIS2_PLACEMENT_3D('',#48357,#38621,#38622);
#34778=AXIS2_PLACEMENT_3D('',#48359,#38623,#38624);
#34779=AXIS2_PLACEMENT_3D('',#48360,#38625,#38626);
#34780=AXIS2_PLACEMENT_3D('',#48365,#38628,#38629);
#34781=AXIS2_PLACEMENT_3D('',#48367,#38630,#38631);
#34782=AXIS2_PLACEMENT_3D('',#48369,#38632,#38633);
#34783=AXIS2_PLACEMENT_3D('',#48373,#38635,#38636);
#34784=AXIS2_PLACEMENT_3D('',#48375,#38637,#38638);
#34785=AXIS2_PLACEMENT_3D('',#48376,#38639,#38640);
#34786=AXIS2_PLACEMENT_3D('',#48381,#38642,#38643);
#34787=AXIS2_PLACEMENT_3D('',#48383,#38644,#38645);
#34788=AXIS2_PLACEMENT_3D('',#48385,#38646,#38647);
#34789=AXIS2_PLACEMENT_3D('',#48389,#38649,#38650);
#34790=AXIS2_PLACEMENT_3D('',#48391,#38651,#38652);
#34791=AXIS2_PLACEMENT_3D('',#48392,#38653,#38654);
#34792=AXIS2_PLACEMENT_3D('',#48397,#38656,#38657);
#34793=AXIS2_PLACEMENT_3D('',#48399,#38658,#38659);
#34794=AXIS2_PLACEMENT_3D('',#48401,#38660,#38661);
#34795=AXIS2_PLACEMENT_3D('',#48405,#38663,#38664);
#34796=AXIS2_PLACEMENT_3D('',#48407,#38665,#38666);
#34797=AXIS2_PLACEMENT_3D('',#48408,#38667,#38668);
#34798=AXIS2_PLACEMENT_3D('',#48413,#38670,#38671);
#34799=AXIS2_PLACEMENT_3D('',#48415,#38672,#38673);
#34800=AXIS2_PLACEMENT_3D('',#48417,#38674,#38675);
#34801=AXIS2_PLACEMENT_3D('',#48421,#38677,#38678);
#34802=AXIS2_PLACEMENT_3D('',#48423,#38679,#38680);
#34803=AXIS2_PLACEMENT_3D('',#48424,#38681,#38682);
#34804=AXIS2_PLACEMENT_3D('',#48429,#38684,#38685);
#34805=AXIS2_PLACEMENT_3D('',#48431,#38686,#38687);
#34806=AXIS2_PLACEMENT_3D('',#48433,#38688,#38689);
#34807=AXIS2_PLACEMENT_3D('',#48437,#38691,#38692);
#34808=AXIS2_PLACEMENT_3D('',#48439,#38693,#38694);
#34809=AXIS2_PLACEMENT_3D('',#48440,#38695,#38696);
#34810=AXIS2_PLACEMENT_3D('',#48445,#38698,#38699);
#34811=AXIS2_PLACEMENT_3D('',#48447,#38700,#38701);
#34812=AXIS2_PLACEMENT_3D('',#48449,#38702,#38703);
#34813=AXIS2_PLACEMENT_3D('',#48453,#38705,#38706);
#34814=AXIS2_PLACEMENT_3D('',#48455,#38707,#38708);
#34815=AXIS2_PLACEMENT_3D('',#48456,#38709,#38710);
#34816=AXIS2_PLACEMENT_3D('',#48461,#38712,#38713);
#34817=AXIS2_PLACEMENT_3D('',#48463,#38714,#38715);
#34818=AXIS2_PLACEMENT_3D('',#48465,#38716,#38717);
#34819=AXIS2_PLACEMENT_3D('',#48469,#38719,#38720);
#34820=AXIS2_PLACEMENT_3D('',#48471,#38721,#38722);
#34821=AXIS2_PLACEMENT_3D('',#48472,#38723,#38724);
#34822=AXIS2_PLACEMENT_3D('',#48477,#38726,#38727);
#34823=AXIS2_PLACEMENT_3D('',#48479,#38728,#38729);
#34824=AXIS2_PLACEMENT_3D('',#48481,#38730,#38731);
#34825=AXIS2_PLACEMENT_3D('',#48485,#38733,#38734);
#34826=AXIS2_PLACEMENT_3D('',#48487,#38735,#38736);
#34827=AXIS2_PLACEMENT_3D('',#48488,#38737,#38738);
#34828=AXIS2_PLACEMENT_3D('',#48493,#38740,#38741);
#34829=AXIS2_PLACEMENT_3D('',#48495,#38742,#38743);
#34830=AXIS2_PLACEMENT_3D('',#48497,#38744,#38745);
#34831=AXIS2_PLACEMENT_3D('',#48501,#38747,#38748);
#34832=AXIS2_PLACEMENT_3D('',#48503,#38749,#38750);
#34833=AXIS2_PLACEMENT_3D('',#48504,#38751,#38752);
#34834=AXIS2_PLACEMENT_3D('',#48509,#38754,#38755);
#34835=AXIS2_PLACEMENT_3D('',#48511,#38756,#38757);
#34836=AXIS2_PLACEMENT_3D('',#48513,#38758,#38759);
#34837=AXIS2_PLACEMENT_3D('',#48517,#38761,#38762);
#34838=AXIS2_PLACEMENT_3D('',#48519,#38763,#38764);
#34839=AXIS2_PLACEMENT_3D('',#48520,#38765,#38766);
#34840=AXIS2_PLACEMENT_3D('',#48525,#38768,#38769);
#34841=AXIS2_PLACEMENT_3D('',#48527,#38770,#38771);
#34842=AXIS2_PLACEMENT_3D('',#48529,#38772,#38773);
#34843=AXIS2_PLACEMENT_3D('',#48533,#38775,#38776);
#34844=AXIS2_PLACEMENT_3D('',#48535,#38777,#38778);
#34845=AXIS2_PLACEMENT_3D('',#48536,#38779,#38780);
#34846=AXIS2_PLACEMENT_3D('',#48541,#38782,#38783);
#34847=AXIS2_PLACEMENT_3D('',#48543,#38784,#38785);
#34848=AXIS2_PLACEMENT_3D('',#48545,#38786,#38787);
#34849=AXIS2_PLACEMENT_3D('',#48549,#38789,#38790);
#34850=AXIS2_PLACEMENT_3D('',#48551,#38791,#38792);
#34851=AXIS2_PLACEMENT_3D('',#48552,#38793,#38794);
#34852=AXIS2_PLACEMENT_3D('',#48557,#38796,#38797);
#34853=AXIS2_PLACEMENT_3D('',#48559,#38798,#38799);
#34854=AXIS2_PLACEMENT_3D('',#48561,#38800,#38801);
#34855=AXIS2_PLACEMENT_3D('',#48565,#38803,#38804);
#34856=AXIS2_PLACEMENT_3D('',#48567,#38805,#38806);
#34857=AXIS2_PLACEMENT_3D('',#48568,#38807,#38808);
#34858=AXIS2_PLACEMENT_3D('',#48573,#38810,#38811);
#34859=AXIS2_PLACEMENT_3D('',#48575,#38812,#38813);
#34860=AXIS2_PLACEMENT_3D('',#48577,#38814,#38815);
#34861=AXIS2_PLACEMENT_3D('',#48581,#38817,#38818);
#34862=AXIS2_PLACEMENT_3D('',#48583,#38819,#38820);
#34863=AXIS2_PLACEMENT_3D('',#48584,#38821,#38822);
#34864=AXIS2_PLACEMENT_3D('',#48585,#38823,#38824);
#34865=AXIS2_PLACEMENT_3D('',#48588,#38825,#38826);
#34866=AXIS2_PLACEMENT_3D('',#48595,#38827,#38828);
#34867=AXIS2_PLACEMENT_3D('',#48600,#38829,#38830);
#34868=AXIS2_PLACEMENT_3D('',#48602,#38831,#38832);
#34869=AXIS2_PLACEMENT_3D('',#48608,#38833,#38834);
#34870=AXIS2_PLACEMENT_3D('',#48609,#38835,#38836);
#34871=AXIS2_PLACEMENT_3D('',#48611,#38837,#38838);
#34872=AXIS2_PLACEMENT_3D('',#48617,#38839,#38840);
#34873=AXIS2_PLACEMENT_3D('',#48618,#38841,#38842);
#34874=AXIS2_PLACEMENT_3D('',#48620,#38843,#38844);
#34875=AXIS2_PLACEMENT_3D('',#48626,#38845,#38846);
#34876=AXIS2_PLACEMENT_3D('',#48627,#38847,#38848);
#34877=AXIS2_PLACEMENT_3D('',#48629,#38849,#38850);
#34878=AXIS2_PLACEMENT_3D('',#48635,#38851,#38852);
#34879=AXIS2_PLACEMENT_3D('',#48636,#38853,#38854);
#34880=AXIS2_PLACEMENT_3D('',#48638,#38855,#38856);
#34881=AXIS2_PLACEMENT_3D('',#48644,#38857,#38858);
#34882=AXIS2_PLACEMENT_3D('',#48645,#38859,#38860);
#34883=AXIS2_PLACEMENT_3D('',#48647,#38861,#38862);
#34884=AXIS2_PLACEMENT_3D('',#48649,#38863,#38864);
#34885=AXIS2_PLACEMENT_3D('',#48654,#38865,#38866);
#34886=AXIS2_PLACEMENT_3D('',#48656,#38867,#38868);
#34887=AXIS2_PLACEMENT_3D('',#48658,#38869,#38870);
#34888=AXIS2_PLACEMENT_3D('',#48663,#38871,#38872);
#34889=AXIS2_PLACEMENT_3D('',#48665,#38873,#38874);
#34890=AXIS2_PLACEMENT_3D('',#48667,#38875,#38876);
#34891=AXIS2_PLACEMENT_3D('',#48672,#38877,#38878);
#34892=AXIS2_PLACEMENT_3D('',#48673,#38879,#38880);
#34893=AXIS2_PLACEMENT_3D('',#48674,#38881,#38882);
#34894=AXIS2_PLACEMENT_3D('',#48675,#38883,#38884);
#34895=AXIS2_PLACEMENT_3D('',#48679,#38886,#38887);
#34896=AXIS2_PLACEMENT_3D('',#48681,#38889,#38890);
#34897=AXIS2_PLACEMENT_3D('',#48684,#38892,#38893);
#34898=AXIS2_PLACEMENT_3D('',#48685,#38894,#38895);
#34899=AXIS2_PLACEMENT_3D('',#48688,#38897,#38898);
#34900=AXIS2_PLACEMENT_3D('',#48689,#38899,#38900);
#34901=AXIS2_PLACEMENT_3D('',#48692,#38902,#38903);
#34902=AXIS2_PLACEMENT_3D('',#48693,#38904,#38905);
#34903=AXIS2_PLACEMENT_3D('',#48696,#38907,#38908);
#34904=AXIS2_PLACEMENT_3D('',#48697,#38909,#38910);
#34905=AXIS2_PLACEMENT_3D('',#48700,#38912,#38913);
#34906=AXIS2_PLACEMENT_3D('',#48701,#38914,#38915);
#34907=AXIS2_PLACEMENT_3D('',#48703,#38916,#38917);
#34908=AXIS2_PLACEMENT_3D('',#48705,#38918,#38919);
#34909=AXIS2_PLACEMENT_3D('',#48707,#38920,#38921);
#34910=AXIS2_PLACEMENT_3D('',#48709,#38922,#38923);
#34911=AXIS2_PLACEMENT_3D('',#48711,#38924,#38925);
#34912=AXIS2_PLACEMENT_3D('',#48712,#38926,#38927);
#34913=AXIS2_PLACEMENT_3D('',#48720,#38932,#38933);
#34914=AXIS2_PLACEMENT_3D('',#48724,#38936,#38937);
#34915=AXIS2_PLACEMENT_3D('',#48730,#38941,#38942);
#34916=AXIS2_PLACEMENT_3D('',#48736,#38946,#38947);
#34917=AXIS2_PLACEMENT_3D('',#48740,#38950,#38951);
#34918=AXIS2_PLACEMENT_3D('',#48744,#38954,#38955);
#34919=AXIS2_PLACEMENT_3D('',#48747,#38958,#38959);
#34920=AXIS2_PLACEMENT_3D('',#48754,#38963,#38964);
#34921=AXIS2_PLACEMENT_3D('',#48757,#38967,#38968);
#34922=AXIS2_PLACEMENT_3D('',#48760,#38971,#38972);
#34923=AXIS2_PLACEMENT_3D('',#48763,#38975,#38976);
#34924=AXIS2_PLACEMENT_3D('',#48765,#38978,#38979);
#34925=AXIS2_PLACEMENT_3D('',#48766,#38980,#38981);
#34926=AXIS2_PLACEMENT_3D('',#48767,#38982,#38983);
#34927=AXIS2_PLACEMENT_3D('',#48774,#38987,#38988);
#34928=AXIS2_PLACEMENT_3D('',#48781,#38992,#38993);
#34929=AXIS2_PLACEMENT_3D('',#48788,#38997,#38998);
#34930=AXIS2_PLACEMENT_3D('',#48791,#39001,#39002);
#34931=AXIS2_PLACEMENT_3D('',#48798,#39006,#39007);
#34932=AXIS2_PLACEMENT_3D('',#48801,#39010,#39011);
#34933=AXIS2_PLACEMENT_3D('',#48804,#39014,#39015);
#34934=AXIS2_PLACEMENT_3D('',#48807,#39018,#39019);
#34935=AXIS2_PLACEMENT_3D('',#48810,#39022,#39023);
#34936=AXIS2_PLACEMENT_3D('',#48813,#39026,#39027);
#34937=AXIS2_PLACEMENT_3D('',#48816,#39030,#39031);
#34938=AXIS2_PLACEMENT_3D('',#48819,#39034,#39035);
#34939=AXIS2_PLACEMENT_3D('',#48820,#39036,#39037);
#34940=AXIS2_PLACEMENT_3D('',#48821,#39038,#39039);
#34941=AXIS2_PLACEMENT_3D('',#48822,#39040,#39041);
#34942=AXIS2_PLACEMENT_3D('',#48829,#39045,#39046);
#34943=AXIS2_PLACEMENT_3D('',#48837,#39051,#39052);
#34944=AXIS2_PLACEMENT_3D('',#48840,#39055,#39056);
#34945=AXIS2_PLACEMENT_3D('',#48847,#39060,#39061);
#34946=AXIS2_PLACEMENT_3D('',#48855,#39066,#39067);
#34947=AXIS2_PLACEMENT_3D('',#48858,#39070,#39071);
#34948=AXIS2_PLACEMENT_3D('',#48861,#39074,#39075);
#34949=AXIS2_PLACEMENT_3D('',#48866,#39079,#39080);
#34950=AXIS2_PLACEMENT_3D('',#48868,#39082,#39083);
#34951=AXIS2_PLACEMENT_3D('',#48872,#39086,#39087);
#34952=AXIS2_PLACEMENT_3D('',#48875,#39090,#39091);
#34953=AXIS2_PLACEMENT_3D('',#48876,#39092,#39093);
#34954=AXIS2_PLACEMENT_3D('',#48877,#39094,#39095);
#34955=AXIS2_PLACEMENT_3D('',#48884,#39099,#39100);
#34956=AXIS2_PLACEMENT_3D('',#48891,#39104,#39105);
#34957=AXIS2_PLACEMENT_3D('',#48898,#39109,#39110);
#34958=AXIS2_PLACEMENT_3D('',#48901,#39113,#39114);
#34959=AXIS2_PLACEMENT_3D('',#48908,#39118,#39119);
#34960=AXIS2_PLACEMENT_3D('',#48911,#39122,#39123);
#34961=AXIS2_PLACEMENT_3D('',#48914,#39126,#39127);
#34962=AXIS2_PLACEMENT_3D('',#48917,#39130,#39131);
#34963=AXIS2_PLACEMENT_3D('',#48920,#39134,#39135);
#34964=AXIS2_PLACEMENT_3D('',#48923,#39138,#39139);
#34965=AXIS2_PLACEMENT_3D('',#48926,#39142,#39143);
#34966=AXIS2_PLACEMENT_3D('',#48929,#39146,#39147);
#34967=AXIS2_PLACEMENT_3D('',#48930,#39148,#39149);
#34968=AXIS2_PLACEMENT_3D('',#48931,#39150,#39151);
#34969=AXIS2_PLACEMENT_3D('',#48932,#39152,#39153);
#34970=AXIS2_PLACEMENT_3D('',#48939,#39157,#39158);
#34971=AXIS2_PLACEMENT_3D('',#48946,#39162,#39163);
#34972=AXIS2_PLACEMENT_3D('',#48953,#39167,#39168);
#34973=AXIS2_PLACEMENT_3D('',#48956,#39171,#39172);
#34974=AXIS2_PLACEMENT_3D('',#48963,#39176,#39177);
#34975=AXIS2_PLACEMENT_3D('',#48966,#39180,#39181);
#34976=AXIS2_PLACEMENT_3D('',#48969,#39184,#39185);
#34977=AXIS2_PLACEMENT_3D('',#48972,#39188,#39189);
#34978=AXIS2_PLACEMENT_3D('',#48975,#39192,#39193);
#34979=AXIS2_PLACEMENT_3D('',#48978,#39196,#39197);
#34980=AXIS2_PLACEMENT_3D('',#48981,#39200,#39201);
#34981=AXIS2_PLACEMENT_3D('',#48984,#39204,#39205);
#34982=AXIS2_PLACEMENT_3D('',#48985,#39206,#39207);
#34983=AXIS2_PLACEMENT_3D('',#48986,#39208,#39209);
#34984=AXIS2_PLACEMENT_3D('',#48987,#39210,#39211);
#34985=AXIS2_PLACEMENT_3D('',#48995,#39216,#39217);
#34986=AXIS2_PLACEMENT_3D('',#48999,#39220,#39221);
#34987=AXIS2_PLACEMENT_3D('',#49005,#39225,#39226);
#34988=AXIS2_PLACEMENT_3D('',#49011,#39230,#39231);
#34989=AXIS2_PLACEMENT_3D('',#49015,#39234,#39235);
#34990=AXIS2_PLACEMENT_3D('',#49019,#39238,#39239);
#34991=AXIS2_PLACEMENT_3D('',#49022,#39242,#39243);
#34992=AXIS2_PLACEMENT_3D('',#49029,#39247,#39248);
#34993=AXIS2_PLACEMENT_3D('',#49032,#39251,#39252);
#34994=AXIS2_PLACEMENT_3D('',#49035,#39255,#39256);
#34995=AXIS2_PLACEMENT_3D('',#49038,#39259,#39260);
#34996=AXIS2_PLACEMENT_3D('',#49040,#39262,#39263);
#34997=AXIS2_PLACEMENT_3D('',#49041,#39264,#39265);
#34998=AXIS2_PLACEMENT_3D('',#49042,#39266,#39267);
#34999=AXIS2_PLACEMENT_3D('',#49049,#39271,#39272);
#35000=AXIS2_PLACEMENT_3D('',#49056,#39276,#39277);
#35001=AXIS2_PLACEMENT_3D('',#49063,#39281,#39282);
#35002=AXIS2_PLACEMENT_3D('',#49066,#39285,#39286);
#35003=AXIS2_PLACEMENT_3D('',#49073,#39290,#39291);
#35004=AXIS2_PLACEMENT_3D('',#49076,#39294,#39295);
#35005=AXIS2_PLACEMENT_3D('',#49079,#39298,#39299);
#35006=AXIS2_PLACEMENT_3D('',#49082,#39302,#39303);
#35007=AXIS2_PLACEMENT_3D('',#49085,#39306,#39307);
#35008=AXIS2_PLACEMENT_3D('',#49088,#39310,#39311);
#35009=AXIS2_PLACEMENT_3D('',#49091,#39314,#39315);
#35010=AXIS2_PLACEMENT_3D('',#49094,#39318,#39319);
#35011=AXIS2_PLACEMENT_3D('',#49095,#39320,#39321);
#35012=AXIS2_PLACEMENT_3D('',#49096,#39322,#39323);
#35013=AXIS2_PLACEMENT_3D('',#49097,#39324,#39325);
#35014=AXIS2_PLACEMENT_3D('',#49104,#39329,#39330);
#35015=AXIS2_PLACEMENT_3D('',#49112,#39335,#39336);
#35016=AXIS2_PLACEMENT_3D('',#49115,#39339,#39340);
#35017=AXIS2_PLACEMENT_3D('',#49122,#39344,#39345);
#35018=AXIS2_PLACEMENT_3D('',#49130,#39350,#39351);
#35019=AXIS2_PLACEMENT_3D('',#49133,#39354,#39355);
#35020=AXIS2_PLACEMENT_3D('',#49136,#39358,#39359);
#35021=AXIS2_PLACEMENT_3D('',#49141,#39363,#39364);
#35022=AXIS2_PLACEMENT_3D('',#49143,#39366,#39367);
#35023=AXIS2_PLACEMENT_3D('',#49147,#39370,#39371);
#35024=AXIS2_PLACEMENT_3D('',#49150,#39374,#39375);
#35025=AXIS2_PLACEMENT_3D('',#49151,#39376,#39377);
#35026=AXIS2_PLACEMENT_3D('',#49152,#39378,#39379);
#35027=AXIS2_PLACEMENT_3D('',#49159,#39383,#39384);
#35028=AXIS2_PLACEMENT_3D('',#49166,#39388,#39389);
#35029=AXIS2_PLACEMENT_3D('',#49173,#39393,#39394);
#35030=AXIS2_PLACEMENT_3D('',#49176,#39397,#39398);
#35031=AXIS2_PLACEMENT_3D('',#49183,#39402,#39403);
#35032=AXIS2_PLACEMENT_3D('',#49186,#39406,#39407);
#35033=AXIS2_PLACEMENT_3D('',#49189,#39410,#39411);
#35034=AXIS2_PLACEMENT_3D('',#49192,#39414,#39415);
#35035=AXIS2_PLACEMENT_3D('',#49195,#39418,#39419);
#35036=AXIS2_PLACEMENT_3D('',#49198,#39422,#39423);
#35037=AXIS2_PLACEMENT_3D('',#49201,#39426,#39427);
#35038=AXIS2_PLACEMENT_3D('',#49204,#39430,#39431);
#35039=AXIS2_PLACEMENT_3D('',#49205,#39432,#39433);
#35040=AXIS2_PLACEMENT_3D('',#49206,#39434,#39435);
#35041=AXIS2_PLACEMENT_3D('',#49207,#39436,#39437);
#35042=AXIS2_PLACEMENT_3D('',#49214,#39441,#39442);
#35043=AXIS2_PLACEMENT_3D('',#49221,#39446,#39447);
#35044=AXIS2_PLACEMENT_3D('',#49228,#39451,#39452);
#35045=AXIS2_PLACEMENT_3D('',#49231,#39455,#39456);
#35046=AXIS2_PLACEMENT_3D('',#49238,#39460,#39461);
#35047=AXIS2_PLACEMENT_3D('',#49241,#39464,#39465);
#35048=AXIS2_PLACEMENT_3D('',#49244,#39468,#39469);
#35049=AXIS2_PLACEMENT_3D('',#49247,#39472,#39473);
#35050=AXIS2_PLACEMENT_3D('',#49250,#39476,#39477);
#35051=AXIS2_PLACEMENT_3D('',#49253,#39480,#39481);
#35052=AXIS2_PLACEMENT_3D('',#49256,#39484,#39485);
#35053=AXIS2_PLACEMENT_3D('',#49259,#39488,#39489);
#35054=AXIS2_PLACEMENT_3D('',#49260,#39490,#39491);
#35055=AXIS2_PLACEMENT_3D('',#49261,#39492,#39493);
#35056=AXIS2_PLACEMENT_3D('',#49262,#39494,#39495);
#35057=AXIS2_PLACEMENT_3D('',#49270,#39500,#39501);
#35058=AXIS2_PLACEMENT_3D('',#49274,#39504,#39505);
#35059=AXIS2_PLACEMENT_3D('',#49280,#39509,#39510);
#35060=AXIS2_PLACEMENT_3D('',#49286,#39514,#39515);
#35061=AXIS2_PLACEMENT_3D('',#49290,#39518,#39519);
#35062=AXIS2_PLACEMENT_3D('',#49294,#39522,#39523);
#35063=AXIS2_PLACEMENT_3D('',#49297,#39526,#39527);
#35064=AXIS2_PLACEMENT_3D('',#49304,#39531,#39532);
#35065=AXIS2_PLACEMENT_3D('',#49307,#39535,#39536);
#35066=AXIS2_PLACEMENT_3D('',#49310,#39539,#39540);
#35067=AXIS2_PLACEMENT_3D('',#49313,#39543,#39544);
#35068=AXIS2_PLACEMENT_3D('',#49315,#39546,#39547);
#35069=AXIS2_PLACEMENT_3D('',#49316,#39548,#39549);
#35070=AXIS2_PLACEMENT_3D('',#49317,#39550,#39551);
#35071=AXIS2_PLACEMENT_3D('',#49324,#39555,#39556);
#35072=AXIS2_PLACEMENT_3D('',#49331,#39560,#39561);
#35073=AXIS2_PLACEMENT_3D('',#49338,#39565,#39566);
#35074=AXIS2_PLACEMENT_3D('',#49341,#39569,#39570);
#35075=AXIS2_PLACEMENT_3D('',#49348,#39574,#39575);
#35076=AXIS2_PLACEMENT_3D('',#49351,#39578,#39579);
#35077=AXIS2_PLACEMENT_3D('',#49354,#39582,#39583);
#35078=AXIS2_PLACEMENT_3D('',#49357,#39586,#39587);
#35079=AXIS2_PLACEMENT_3D('',#49360,#39590,#39591);
#35080=AXIS2_PLACEMENT_3D('',#49363,#39594,#39595);
#35081=AXIS2_PLACEMENT_3D('',#49366,#39598,#39599);
#35082=AXIS2_PLACEMENT_3D('',#49369,#39602,#39603);
#35083=AXIS2_PLACEMENT_3D('',#49370,#39604,#39605);
#35084=AXIS2_PLACEMENT_3D('',#49371,#39606,#39607);
#35085=AXIS2_PLACEMENT_3D('',#49372,#39608,#39609);
#35086=AXIS2_PLACEMENT_3D('',#49379,#39613,#39614);
#35087=AXIS2_PLACEMENT_3D('',#49387,#39619,#39620);
#35088=AXIS2_PLACEMENT_3D('',#49390,#39623,#39624);
#35089=AXIS2_PLACEMENT_3D('',#49397,#39628,#39629);
#35090=AXIS2_PLACEMENT_3D('',#49405,#39634,#39635);
#35091=AXIS2_PLACEMENT_3D('',#49408,#39638,#39639);
#35092=AXIS2_PLACEMENT_3D('',#49411,#39642,#39643);
#35093=AXIS2_PLACEMENT_3D('',#49416,#39647,#39648);
#35094=AXIS2_PLACEMENT_3D('',#49418,#39650,#39651);
#35095=AXIS2_PLACEMENT_3D('',#49422,#39654,#39655);
#35096=AXIS2_PLACEMENT_3D('',#49425,#39658,#39659);
#35097=AXIS2_PLACEMENT_3D('',#49426,#39660,#39661);
#35098=AXIS2_PLACEMENT_3D('',#49427,#39662,#39663);
#35099=AXIS2_PLACEMENT_3D('',#49434,#39667,#39668);
#35100=AXIS2_PLACEMENT_3D('',#49441,#39672,#39673);
#35101=AXIS2_PLACEMENT_3D('',#49448,#39677,#39678);
#35102=AXIS2_PLACEMENT_3D('',#49451,#39681,#39682);
#35103=AXIS2_PLACEMENT_3D('',#49458,#39686,#39687);
#35104=AXIS2_PLACEMENT_3D('',#49461,#39690,#39691);
#35105=AXIS2_PLACEMENT_3D('',#49464,#39694,#39695);
#35106=AXIS2_PLACEMENT_3D('',#49467,#39698,#39699);
#35107=AXIS2_PLACEMENT_3D('',#49470,#39702,#39703);
#35108=AXIS2_PLACEMENT_3D('',#49473,#39706,#39707);
#35109=AXIS2_PLACEMENT_3D('',#49476,#39710,#39711);
#35110=AXIS2_PLACEMENT_3D('',#49479,#39714,#39715);
#35111=AXIS2_PLACEMENT_3D('',#49480,#39716,#39717);
#35112=AXIS2_PLACEMENT_3D('',#49481,#39718,#39719);
#35113=AXIS2_PLACEMENT_3D('',#49482,#39720,#39721);
#35114=AXIS2_PLACEMENT_3D('',#49489,#39725,#39726);
#35115=AXIS2_PLACEMENT_3D('',#49496,#39730,#39731);
#35116=AXIS2_PLACEMENT_3D('',#49503,#39735,#39736);
#35117=AXIS2_PLACEMENT_3D('',#49506,#39739,#39740);
#35118=AXIS2_PLACEMENT_3D('',#49513,#39744,#39745);
#35119=AXIS2_PLACEMENT_3D('',#49516,#39748,#39749);
#35120=AXIS2_PLACEMENT_3D('',#49519,#39752,#39753);
#35121=AXIS2_PLACEMENT_3D('',#49522,#39756,#39757);
#35122=AXIS2_PLACEMENT_3D('',#49525,#39760,#39761);
#35123=AXIS2_PLACEMENT_3D('',#49528,#39764,#39765);
#35124=AXIS2_PLACEMENT_3D('',#49531,#39768,#39769);
#35125=AXIS2_PLACEMENT_3D('',#49534,#39772,#39773);
#35126=AXIS2_PLACEMENT_3D('',#49535,#39774,#39775);
#35127=AXIS2_PLACEMENT_3D('',#49536,#39776,#39777);
#35128=AXIS2_PLACEMENT_3D('',#49537,#39778,#39779);
#35129=AXIS2_PLACEMENT_3D('',#49545,#39784,#39785);
#35130=AXIS2_PLACEMENT_3D('',#49549,#39788,#39789);
#35131=AXIS2_PLACEMENT_3D('',#49555,#39793,#39794);
#35132=AXIS2_PLACEMENT_3D('',#49561,#39798,#39799);
#35133=AXIS2_PLACEMENT_3D('',#49565,#39802,#39803);
#35134=AXIS2_PLACEMENT_3D('',#49569,#39806,#39807);
#35135=AXIS2_PLACEMENT_3D('',#49572,#39810,#39811);
#35136=AXIS2_PLACEMENT_3D('',#49579,#39815,#39816);
#35137=AXIS2_PLACEMENT_3D('',#49582,#39819,#39820);
#35138=AXIS2_PLACEMENT_3D('',#49585,#39823,#39824);
#35139=AXIS2_PLACEMENT_3D('',#49588,#39827,#39828);
#35140=AXIS2_PLACEMENT_3D('',#49590,#39830,#39831);
#35141=AXIS2_PLACEMENT_3D('',#49591,#39832,#39833);
#35142=AXIS2_PLACEMENT_3D('',#49592,#39834,#39835);
#35143=AXIS2_PLACEMENT_3D('',#49599,#39839,#39840);
#35144=AXIS2_PLACEMENT_3D('',#49606,#39844,#39845);
#35145=AXIS2_PLACEMENT_3D('',#49613,#39849,#39850);
#35146=AXIS2_PLACEMENT_3D('',#49616,#39853,#39854);
#35147=AXIS2_PLACEMENT_3D('',#49623,#39858,#39859);
#35148=AXIS2_PLACEMENT_3D('',#49626,#39862,#39863);
#35149=AXIS2_PLACEMENT_3D('',#49629,#39866,#39867);
#35150=AXIS2_PLACEMENT_3D('',#49632,#39870,#39871);
#35151=AXIS2_PLACEMENT_3D('',#49635,#39874,#39875);
#35152=AXIS2_PLACEMENT_3D('',#49638,#39878,#39879);
#35153=AXIS2_PLACEMENT_3D('',#49641,#39882,#39883);
#35154=AXIS2_PLACEMENT_3D('',#49644,#39886,#39887);
#35155=AXIS2_PLACEMENT_3D('',#49645,#39888,#39889);
#35156=AXIS2_PLACEMENT_3D('',#49646,#39890,#39891);
#35157=AXIS2_PLACEMENT_3D('',#49647,#39892,#39893);
#35158=AXIS2_PLACEMENT_3D('',#49654,#39897,#39898);
#35159=AXIS2_PLACEMENT_3D('',#49662,#39903,#39904);
#35160=AXIS2_PLACEMENT_3D('',#49665,#39907,#39908);
#35161=AXIS2_PLACEMENT_3D('',#49672,#39912,#39913);
#35162=AXIS2_PLACEMENT_3D('',#49680,#39918,#39919);
#35163=AXIS2_PLACEMENT_3D('',#49683,#39922,#39923);
#35164=AXIS2_PLACEMENT_3D('',#49686,#39926,#39927);
#35165=AXIS2_PLACEMENT_3D('',#49691,#39931,#39932);
#35166=AXIS2_PLACEMENT_3D('',#49693,#39934,#39935);
#35167=AXIS2_PLACEMENT_3D('',#49697,#39938,#39939);
#35168=AXIS2_PLACEMENT_3D('',#49700,#39942,#39943);
#35169=AXIS2_PLACEMENT_3D('',#49701,#39944,#39945);
#35170=AXIS2_PLACEMENT_3D('',#49702,#39946,#39947);
#35171=AXIS2_PLACEMENT_3D('',#49709,#39951,#39952);
#35172=AXIS2_PLACEMENT_3D('',#49716,#39956,#39957);
#35173=AXIS2_PLACEMENT_3D('',#49723,#39961,#39962);
#35174=AXIS2_PLACEMENT_3D('',#49726,#39965,#39966);
#35175=AXIS2_PLACEMENT_3D('',#49733,#39970,#39971);
#35176=AXIS2_PLACEMENT_3D('',#49736,#39974,#39975);
#35177=AXIS2_PLACEMENT_3D('',#49739,#39978,#39979);
#35178=AXIS2_PLACEMENT_3D('',#49742,#39982,#39983);
#35179=AXIS2_PLACEMENT_3D('',#49745,#39986,#39987);
#35180=AXIS2_PLACEMENT_3D('',#49748,#39990,#39991);
#35181=AXIS2_PLACEMENT_3D('',#49751,#39994,#39995);
#35182=AXIS2_PLACEMENT_3D('',#49754,#39998,#39999);
#35183=AXIS2_PLACEMENT_3D('',#49755,#40000,#40001);
#35184=AXIS2_PLACEMENT_3D('',#49756,#40002,#40003);
#35185=AXIS2_PLACEMENT_3D('',#49757,#40004,#40005);
#35186=AXIS2_PLACEMENT_3D('',#49764,#40009,#40010);
#35187=AXIS2_PLACEMENT_3D('',#49771,#40014,#40015);
#35188=AXIS2_PLACEMENT_3D('',#49778,#40019,#40020);
#35189=AXIS2_PLACEMENT_3D('',#49781,#40023,#40024);
#35190=AXIS2_PLACEMENT_3D('',#49788,#40028,#40029);
#35191=AXIS2_PLACEMENT_3D('',#49791,#40032,#40033);
#35192=AXIS2_PLACEMENT_3D('',#49794,#40036,#40037);
#35193=AXIS2_PLACEMENT_3D('',#49797,#40040,#40041);
#35194=AXIS2_PLACEMENT_3D('',#49800,#40044,#40045);
#35195=AXIS2_PLACEMENT_3D('',#49803,#40048,#40049);
#35196=AXIS2_PLACEMENT_3D('',#49806,#40052,#40053);
#35197=AXIS2_PLACEMENT_3D('',#49809,#40056,#40057);
#35198=AXIS2_PLACEMENT_3D('',#49810,#40058,#40059);
#35199=AXIS2_PLACEMENT_3D('',#49811,#40060,#40061);
#35200=AXIS2_PLACEMENT_3D('',#49812,#40062,#40063);
#35201=AXIS2_PLACEMENT_3D('',#49820,#40068,#40069);
#35202=AXIS2_PLACEMENT_3D('',#49824,#40072,#40073);
#35203=AXIS2_PLACEMENT_3D('',#49830,#40077,#40078);
#35204=AXIS2_PLACEMENT_3D('',#49836,#40082,#40083);
#35205=AXIS2_PLACEMENT_3D('',#49840,#40086,#40087);
#35206=AXIS2_PLACEMENT_3D('',#49844,#40090,#40091);
#35207=AXIS2_PLACEMENT_3D('',#49847,#40094,#40095);
#35208=AXIS2_PLACEMENT_3D('',#49854,#40099,#40100);
#35209=AXIS2_PLACEMENT_3D('',#49857,#40103,#40104);
#35210=AXIS2_PLACEMENT_3D('',#49860,#40107,#40108);
#35211=AXIS2_PLACEMENT_3D('',#49863,#40111,#40112);
#35212=AXIS2_PLACEMENT_3D('',#49865,#40114,#40115);
#35213=AXIS2_PLACEMENT_3D('',#49866,#40116,#40117);
#35214=AXIS2_PLACEMENT_3D('',#49867,#40118,#40119);
#35215=AXIS2_PLACEMENT_3D('',#49874,#40123,#40124);
#35216=AXIS2_PLACEMENT_3D('',#49881,#40128,#40129);
#35217=AXIS2_PLACEMENT_3D('',#49888,#40133,#40134);
#35218=AXIS2_PLACEMENT_3D('',#49891,#40137,#40138);
#35219=AXIS2_PLACEMENT_3D('',#49898,#40142,#40143);
#35220=AXIS2_PLACEMENT_3D('',#49901,#40146,#40147);
#35221=AXIS2_PLACEMENT_3D('',#49904,#40150,#40151);
#35222=AXIS2_PLACEMENT_3D('',#49907,#40154,#40155);
#35223=AXIS2_PLACEMENT_3D('',#49910,#40158,#40159);
#35224=AXIS2_PLACEMENT_3D('',#49913,#40162,#40163);
#35225=AXIS2_PLACEMENT_3D('',#49916,#40166,#40167);
#35226=AXIS2_PLACEMENT_3D('',#49919,#40170,#40171);
#35227=AXIS2_PLACEMENT_3D('',#49920,#40172,#40173);
#35228=AXIS2_PLACEMENT_3D('',#49921,#40174,#40175);
#35229=AXIS2_PLACEMENT_3D('',#49922,#40176,#40177);
#35230=AXIS2_PLACEMENT_3D('',#49929,#40181,#40182);
#35231=AXIS2_PLACEMENT_3D('',#49937,#40187,#40188);
#35232=AXIS2_PLACEMENT_3D('',#49940,#40191,#40192);
#35233=AXIS2_PLACEMENT_3D('',#49947,#40196,#40197);
#35234=AXIS2_PLACEMENT_3D('',#49955,#40202,#40203);
#35235=AXIS2_PLACEMENT_3D('',#49958,#40206,#40207);
#35236=AXIS2_PLACEMENT_3D('',#49961,#40210,#40211);
#35237=AXIS2_PLACEMENT_3D('',#49966,#40215,#40216);
#35238=AXIS2_PLACEMENT_3D('',#49968,#40218,#40219);
#35239=AXIS2_PLACEMENT_3D('',#49972,#40222,#40223);
#35240=AXIS2_PLACEMENT_3D('',#49975,#40226,#40227);
#35241=AXIS2_PLACEMENT_3D('',#49976,#40228,#40229);
#35242=AXIS2_PLACEMENT_3D('',#49977,#40230,#40231);
#35243=AXIS2_PLACEMENT_3D('',#49984,#40235,#40236);
#35244=AXIS2_PLACEMENT_3D('',#49991,#40240,#40241);
#35245=AXIS2_PLACEMENT_3D('',#49998,#40245,#40246);
#35246=AXIS2_PLACEMENT_3D('',#50001,#40249,#40250);
#35247=AXIS2_PLACEMENT_3D('',#50008,#40254,#40255);
#35248=AXIS2_PLACEMENT_3D('',#50011,#40258,#40259);
#35249=AXIS2_PLACEMENT_3D('',#50014,#40262,#40263);
#35250=AXIS2_PLACEMENT_3D('',#50017,#40266,#40267);
#35251=AXIS2_PLACEMENT_3D('',#50020,#40270,#40271);
#35252=AXIS2_PLACEMENT_3D('',#50023,#40274,#40275);
#35253=AXIS2_PLACEMENT_3D('',#50026,#40278,#40279);
#35254=AXIS2_PLACEMENT_3D('',#50029,#40282,#40283);
#35255=AXIS2_PLACEMENT_3D('',#50030,#40284,#40285);
#35256=AXIS2_PLACEMENT_3D('',#50031,#40286,#40287);
#35257=AXIS2_PLACEMENT_3D('',#50032,#40288,#40289);
#35258=AXIS2_PLACEMENT_3D('',#50039,#40293,#40294);
#35259=AXIS2_PLACEMENT_3D('',#50046,#40298,#40299);
#35260=AXIS2_PLACEMENT_3D('',#50053,#40303,#40304);
#35261=AXIS2_PLACEMENT_3D('',#50056,#40307,#40308);
#35262=AXIS2_PLACEMENT_3D('',#50063,#40312,#40313);
#35263=AXIS2_PLACEMENT_3D('',#50066,#40316,#40317);
#35264=AXIS2_PLACEMENT_3D('',#50069,#40320,#40321);
#35265=AXIS2_PLACEMENT_3D('',#50072,#40324,#40325);
#35266=AXIS2_PLACEMENT_3D('',#50075,#40328,#40329);
#35267=AXIS2_PLACEMENT_3D('',#50078,#40332,#40333);
#35268=AXIS2_PLACEMENT_3D('',#50081,#40336,#40337);
#35269=AXIS2_PLACEMENT_3D('',#50084,#40340,#40341);
#35270=AXIS2_PLACEMENT_3D('',#50085,#40342,#40343);
#35271=AXIS2_PLACEMENT_3D('',#50086,#40344,#40345);
#35272=AXIS2_PLACEMENT_3D('',#50087,#40346,#40347);
#35273=AXIS2_PLACEMENT_3D('',#50095,#40352,#40353);
#35274=AXIS2_PLACEMENT_3D('',#50099,#40356,#40357);
#35275=AXIS2_PLACEMENT_3D('',#50105,#40361,#40362);
#35276=AXIS2_PLACEMENT_3D('',#50111,#40366,#40367);
#35277=AXIS2_PLACEMENT_3D('',#50115,#40370,#40371);
#35278=AXIS2_PLACEMENT_3D('',#50119,#40374,#40375);
#35279=AXIS2_PLACEMENT_3D('',#50122,#40378,#40379);
#35280=AXIS2_PLACEMENT_3D('',#50129,#40383,#40384);
#35281=AXIS2_PLACEMENT_3D('',#50132,#40387,#40388);
#35282=AXIS2_PLACEMENT_3D('',#50135,#40391,#40392);
#35283=AXIS2_PLACEMENT_3D('',#50138,#40395,#40396);
#35284=AXIS2_PLACEMENT_3D('',#50140,#40398,#40399);
#35285=AXIS2_PLACEMENT_3D('',#50141,#40400,#40401);
#35286=AXIS2_PLACEMENT_3D('',#50142,#40402,#40403);
#35287=AXIS2_PLACEMENT_3D('',#50149,#40407,#40408);
#35288=AXIS2_PLACEMENT_3D('',#50156,#40412,#40413);
#35289=AXIS2_PLACEMENT_3D('',#50163,#40417,#40418);
#35290=AXIS2_PLACEMENT_3D('',#50166,#40421,#40422);
#35291=AXIS2_PLACEMENT_3D('',#50173,#40426,#40427);
#35292=AXIS2_PLACEMENT_3D('',#50176,#40430,#40431);
#35293=AXIS2_PLACEMENT_3D('',#50179,#40434,#40435);
#35294=AXIS2_PLACEMENT_3D('',#50182,#40438,#40439);
#35295=AXIS2_PLACEMENT_3D('',#50185,#40442,#40443);
#35296=AXIS2_PLACEMENT_3D('',#50188,#40446,#40447);
#35297=AXIS2_PLACEMENT_3D('',#50191,#40450,#40451);
#35298=AXIS2_PLACEMENT_3D('',#50194,#40454,#40455);
#35299=AXIS2_PLACEMENT_3D('',#50195,#40456,#40457);
#35300=AXIS2_PLACEMENT_3D('',#50196,#40458,#40459);
#35301=AXIS2_PLACEMENT_3D('',#50197,#40460,#40461);
#35302=AXIS2_PLACEMENT_3D('',#50204,#40465,#40466);
#35303=AXIS2_PLACEMENT_3D('',#50212,#40471,#40472);
#35304=AXIS2_PLACEMENT_3D('',#50215,#40475,#40476);
#35305=AXIS2_PLACEMENT_3D('',#50222,#40480,#40481);
#35306=AXIS2_PLACEMENT_3D('',#50230,#40486,#40487);
#35307=AXIS2_PLACEMENT_3D('',#50233,#40490,#40491);
#35308=AXIS2_PLACEMENT_3D('',#50236,#40494,#40495);
#35309=AXIS2_PLACEMENT_3D('',#50241,#40499,#40500);
#35310=AXIS2_PLACEMENT_3D('',#50243,#40502,#40503);
#35311=AXIS2_PLACEMENT_3D('',#50247,#40506,#40507);
#35312=AXIS2_PLACEMENT_3D('',#50250,#40510,#40511);
#35313=AXIS2_PLACEMENT_3D('',#50251,#40512,#40513);
#35314=AXIS2_PLACEMENT_3D('',#50252,#40514,#40515);
#35315=AXIS2_PLACEMENT_3D('',#50259,#40519,#40520);
#35316=AXIS2_PLACEMENT_3D('',#50266,#40524,#40525);
#35317=AXIS2_PLACEMENT_3D('',#50273,#40529,#40530);
#35318=AXIS2_PLACEMENT_3D('',#50276,#40533,#40534);
#35319=AXIS2_PLACEMENT_3D('',#50283,#40538,#40539);
#35320=AXIS2_PLACEMENT_3D('',#50286,#40542,#40543);
#35321=AXIS2_PLACEMENT_3D('',#50289,#40546,#40547);
#35322=AXIS2_PLACEMENT_3D('',#50292,#40550,#40551);
#35323=AXIS2_PLACEMENT_3D('',#50295,#40554,#40555);
#35324=AXIS2_PLACEMENT_3D('',#50298,#40558,#40559);
#35325=AXIS2_PLACEMENT_3D('',#50301,#40562,#40563);
#35326=AXIS2_PLACEMENT_3D('',#50304,#40566,#40567);
#35327=AXIS2_PLACEMENT_3D('',#50305,#40568,#40569);
#35328=AXIS2_PLACEMENT_3D('',#50306,#40570,#40571);
#35329=AXIS2_PLACEMENT_3D('',#50307,#40572,#40573);
#35330=AXIS2_PLACEMENT_3D('',#50314,#40577,#40578);
#35331=AXIS2_PLACEMENT_3D('',#50321,#40582,#40583);
#35332=AXIS2_PLACEMENT_3D('',#50328,#40587,#40588);
#35333=AXIS2_PLACEMENT_3D('',#50331,#40591,#40592);
#35334=AXIS2_PLACEMENT_3D('',#50338,#40596,#40597);
#35335=AXIS2_PLACEMENT_3D('',#50341,#40600,#40601);
#35336=AXIS2_PLACEMENT_3D('',#50344,#40604,#40605);
#35337=AXIS2_PLACEMENT_3D('',#50347,#40608,#40609);
#35338=AXIS2_PLACEMENT_3D('',#50350,#40612,#40613);
#35339=AXIS2_PLACEMENT_3D('',#50353,#40616,#40617);
#35340=AXIS2_PLACEMENT_3D('',#50356,#40620,#40621);
#35341=AXIS2_PLACEMENT_3D('',#50359,#40624,#40625);
#35342=AXIS2_PLACEMENT_3D('',#50360,#40626,#40627);
#35343=AXIS2_PLACEMENT_3D('',#50361,#40628,#40629);
#35344=AXIS2_PLACEMENT_3D('',#50362,#40630,#40631);
#35345=AXIS2_PLACEMENT_3D('',#50370,#40636,#40637);
#35346=AXIS2_PLACEMENT_3D('',#50374,#40640,#40641);
#35347=AXIS2_PLACEMENT_3D('',#50380,#40645,#40646);
#35348=AXIS2_PLACEMENT_3D('',#50386,#40650,#40651);
#35349=AXIS2_PLACEMENT_3D('',#50390,#40654,#40655);
#35350=AXIS2_PLACEMENT_3D('',#50394,#40658,#40659);
#35351=AXIS2_PLACEMENT_3D('',#50397,#40662,#40663);
#35352=AXIS2_PLACEMENT_3D('',#50404,#40667,#40668);
#35353=AXIS2_PLACEMENT_3D('',#50407,#40671,#40672);
#35354=AXIS2_PLACEMENT_3D('',#50410,#40675,#40676);
#35355=AXIS2_PLACEMENT_3D('',#50413,#40679,#40680);
#35356=AXIS2_PLACEMENT_3D('',#50415,#40682,#40683);
#35357=AXIS2_PLACEMENT_3D('',#50416,#40684,#40685);
#35358=AXIS2_PLACEMENT_3D('',#50417,#40686,#40687);
#35359=AXIS2_PLACEMENT_3D('',#50424,#40691,#40692);
#35360=AXIS2_PLACEMENT_3D('',#50431,#40696,#40697);
#35361=AXIS2_PLACEMENT_3D('',#50438,#40701,#40702);
#35362=AXIS2_PLACEMENT_3D('',#50441,#40705,#40706);
#35363=AXIS2_PLACEMENT_3D('',#50448,#40710,#40711);
#35364=AXIS2_PLACEMENT_3D('',#50451,#40714,#40715);
#35365=AXIS2_PLACEMENT_3D('',#50454,#40718,#40719);
#35366=AXIS2_PLACEMENT_3D('',#50457,#40722,#40723);
#35367=AXIS2_PLACEMENT_3D('',#50460,#40726,#40727);
#35368=AXIS2_PLACEMENT_3D('',#50463,#40730,#40731);
#35369=AXIS2_PLACEMENT_3D('',#50466,#40734,#40735);
#35370=AXIS2_PLACEMENT_3D('',#50469,#40738,#40739);
#35371=AXIS2_PLACEMENT_3D('',#50470,#40740,#40741);
#35372=AXIS2_PLACEMENT_3D('',#50471,#40742,#40743);
#35373=AXIS2_PLACEMENT_3D('',#50472,#40744,#40745);
#35374=AXIS2_PLACEMENT_3D('',#50479,#40749,#40750);
#35375=AXIS2_PLACEMENT_3D('',#50487,#40755,#40756);
#35376=AXIS2_PLACEMENT_3D('',#50490,#40759,#40760);
#35377=AXIS2_PLACEMENT_3D('',#50497,#40764,#40765);
#35378=AXIS2_PLACEMENT_3D('',#50505,#40770,#40771);
#35379=AXIS2_PLACEMENT_3D('',#50508,#40774,#40775);
#35380=AXIS2_PLACEMENT_3D('',#50511,#40778,#40779);
#35381=AXIS2_PLACEMENT_3D('',#50516,#40783,#40784);
#35382=AXIS2_PLACEMENT_3D('',#50518,#40786,#40787);
#35383=AXIS2_PLACEMENT_3D('',#50522,#40790,#40791);
#35384=AXIS2_PLACEMENT_3D('',#50525,#40794,#40795);
#35385=AXIS2_PLACEMENT_3D('',#50526,#40796,#40797);
#35386=AXIS2_PLACEMENT_3D('',#50527,#40798,#40799);
#35387=AXIS2_PLACEMENT_3D('',#50534,#40803,#40804);
#35388=AXIS2_PLACEMENT_3D('',#50541,#40808,#40809);
#35389=AXIS2_PLACEMENT_3D('',#50548,#40813,#40814);
#35390=AXIS2_PLACEMENT_3D('',#50551,#40817,#40818);
#35391=AXIS2_PLACEMENT_3D('',#50558,#40822,#40823);
#35392=AXIS2_PLACEMENT_3D('',#50561,#40826,#40827);
#35393=AXIS2_PLACEMENT_3D('',#50564,#40830,#40831);
#35394=AXIS2_PLACEMENT_3D('',#50567,#40834,#40835);
#35395=AXIS2_PLACEMENT_3D('',#50570,#40838,#40839);
#35396=AXIS2_PLACEMENT_3D('',#50573,#40842,#40843);
#35397=AXIS2_PLACEMENT_3D('',#50576,#40846,#40847);
#35398=AXIS2_PLACEMENT_3D('',#50579,#40850,#40851);
#35399=AXIS2_PLACEMENT_3D('',#50580,#40852,#40853);
#35400=AXIS2_PLACEMENT_3D('',#50581,#40854,#40855);
#35401=AXIS2_PLACEMENT_3D('',#50582,#40856,#40857);
#35402=AXIS2_PLACEMENT_3D('',#50589,#40861,#40862);
#35403=AXIS2_PLACEMENT_3D('',#50596,#40866,#40867);
#35404=AXIS2_PLACEMENT_3D('',#50603,#40871,#40872);
#35405=AXIS2_PLACEMENT_3D('',#50606,#40875,#40876);
#35406=AXIS2_PLACEMENT_3D('',#50613,#40880,#40881);
#35407=AXIS2_PLACEMENT_3D('',#50616,#40884,#40885);
#35408=AXIS2_PLACEMENT_3D('',#50619,#40888,#40889);
#35409=AXIS2_PLACEMENT_3D('',#50622,#40892,#40893);
#35410=AXIS2_PLACEMENT_3D('',#50625,#40896,#40897);
#35411=AXIS2_PLACEMENT_3D('',#50628,#40900,#40901);
#35412=AXIS2_PLACEMENT_3D('',#50631,#40904,#40905);
#35413=AXIS2_PLACEMENT_3D('',#50634,#40908,#40909);
#35414=AXIS2_PLACEMENT_3D('',#50635,#40910,#40911);
#35415=AXIS2_PLACEMENT_3D('',#50636,#40912,#40913);
#35416=AXIS2_PLACEMENT_3D('',#50637,#40914,#40915);
#35417=AXIS2_PLACEMENT_3D('',#50645,#40920,#40921);
#35418=AXIS2_PLACEMENT_3D('',#50649,#40924,#40925);
#35419=AXIS2_PLACEMENT_3D('',#50655,#40929,#40930);
#35420=AXIS2_PLACEMENT_3D('',#50661,#40934,#40935);
#35421=AXIS2_PLACEMENT_3D('',#50665,#40938,#40939);
#35422=AXIS2_PLACEMENT_3D('',#50669,#40942,#40943);
#35423=AXIS2_PLACEMENT_3D('',#50672,#40946,#40947);
#35424=AXIS2_PLACEMENT_3D('',#50679,#40951,#40952);
#35425=AXIS2_PLACEMENT_3D('',#50682,#40955,#40956);
#35426=AXIS2_PLACEMENT_3D('',#50685,#40959,#40960);
#35427=AXIS2_PLACEMENT_3D('',#50688,#40963,#40964);
#35428=AXIS2_PLACEMENT_3D('',#50690,#40966,#40967);
#35429=AXIS2_PLACEMENT_3D('',#50691,#40968,#40969);
#35430=AXIS2_PLACEMENT_3D('',#50692,#40970,#40971);
#35431=AXIS2_PLACEMENT_3D('',#50699,#40975,#40976);
#35432=AXIS2_PLACEMENT_3D('',#50706,#40980,#40981);
#35433=AXIS2_PLACEMENT_3D('',#50713,#40985,#40986);
#35434=AXIS2_PLACEMENT_3D('',#50716,#40989,#40990);
#35435=AXIS2_PLACEMENT_3D('',#50723,#40994,#40995);
#35436=AXIS2_PLACEMENT_3D('',#50726,#40998,#40999);
#35437=AXIS2_PLACEMENT_3D('',#50729,#41002,#41003);
#35438=AXIS2_PLACEMENT_3D('',#50732,#41006,#41007);
#35439=AXIS2_PLACEMENT_3D('',#50735,#41010,#41011);
#35440=AXIS2_PLACEMENT_3D('',#50738,#41014,#41015);
#35441=AXIS2_PLACEMENT_3D('',#50741,#41018,#41019);
#35442=AXIS2_PLACEMENT_3D('',#50744,#41022,#41023);
#35443=AXIS2_PLACEMENT_3D('',#50745,#41024,#41025);
#35444=AXIS2_PLACEMENT_3D('',#50746,#41026,#41027);
#35445=AXIS2_PLACEMENT_3D('',#50747,#41028,#41029);
#35446=AXIS2_PLACEMENT_3D('',#50754,#41033,#41034);
#35447=AXIS2_PLACEMENT_3D('',#50762,#41039,#41040);
#35448=AXIS2_PLACEMENT_3D('',#50765,#41043,#41044);
#35449=AXIS2_PLACEMENT_3D('',#50772,#41048,#41049);
#35450=AXIS2_PLACEMENT_3D('',#50780,#41054,#41055);
#35451=AXIS2_PLACEMENT_3D('',#50783,#41058,#41059);
#35452=AXIS2_PLACEMENT_3D('',#50786,#41062,#41063);
#35453=AXIS2_PLACEMENT_3D('',#50791,#41067,#41068);
#35454=AXIS2_PLACEMENT_3D('',#50793,#41070,#41071);
#35455=AXIS2_PLACEMENT_3D('',#50797,#41074,#41075);
#35456=AXIS2_PLACEMENT_3D('',#50800,#41078,#41079);
#35457=AXIS2_PLACEMENT_3D('',#50801,#41080,#41081);
#35458=AXIS2_PLACEMENT_3D('',#50802,#41082,#41083);
#35459=AXIS2_PLACEMENT_3D('',#50809,#41087,#41088);
#35460=AXIS2_PLACEMENT_3D('',#50816,#41092,#41093);
#35461=AXIS2_PLACEMENT_3D('',#50823,#41097,#41098);
#35462=AXIS2_PLACEMENT_3D('',#50826,#41101,#41102);
#35463=AXIS2_PLACEMENT_3D('',#50833,#41106,#41107);
#35464=AXIS2_PLACEMENT_3D('',#50836,#41110,#41111);
#35465=AXIS2_PLACEMENT_3D('',#50839,#41114,#41115);
#35466=AXIS2_PLACEMENT_3D('',#50842,#41118,#41119);
#35467=AXIS2_PLACEMENT_3D('',#50845,#41122,#41123);
#35468=AXIS2_PLACEMENT_3D('',#50848,#41126,#41127);
#35469=AXIS2_PLACEMENT_3D('',#50851,#41130,#41131);
#35470=AXIS2_PLACEMENT_3D('',#50854,#41134,#41135);
#35471=AXIS2_PLACEMENT_3D('',#50855,#41136,#41137);
#35472=AXIS2_PLACEMENT_3D('',#50856,#41138,#41139);
#35473=AXIS2_PLACEMENT_3D('',#50857,#41140,#41141);
#35474=AXIS2_PLACEMENT_3D('',#50864,#41145,#41146);
#35475=AXIS2_PLACEMENT_3D('',#50871,#41150,#41151);
#35476=AXIS2_PLACEMENT_3D('',#50878,#41155,#41156);
#35477=AXIS2_PLACEMENT_3D('',#50881,#41159,#41160);
#35478=AXIS2_PLACEMENT_3D('',#50888,#41164,#41165);
#35479=AXIS2_PLACEMENT_3D('',#50891,#41168,#41169);
#35480=AXIS2_PLACEMENT_3D('',#50894,#41172,#41173);
#35481=AXIS2_PLACEMENT_3D('',#50897,#41176,#41177);
#35482=AXIS2_PLACEMENT_3D('',#50900,#41180,#41181);
#35483=AXIS2_PLACEMENT_3D('',#50903,#41184,#41185);
#35484=AXIS2_PLACEMENT_3D('',#50906,#41188,#41189);
#35485=AXIS2_PLACEMENT_3D('',#50909,#41192,#41193);
#35486=AXIS2_PLACEMENT_3D('',#50910,#41194,#41195);
#35487=AXIS2_PLACEMENT_3D('',#50911,#41196,#41197);
#35488=AXIS2_PLACEMENT_3D('',#50912,#41198,#41199);
#35489=AXIS2_PLACEMENT_3D('',#50920,#41204,#41205);
#35490=AXIS2_PLACEMENT_3D('',#50924,#41208,#41209);
#35491=AXIS2_PLACEMENT_3D('',#50930,#41213,#41214);
#35492=AXIS2_PLACEMENT_3D('',#50936,#41218,#41219);
#35493=AXIS2_PLACEMENT_3D('',#50940,#41222,#41223);
#35494=AXIS2_PLACEMENT_3D('',#50944,#41226,#41227);
#35495=AXIS2_PLACEMENT_3D('',#50947,#41230,#41231);
#35496=AXIS2_PLACEMENT_3D('',#50954,#41235,#41236);
#35497=AXIS2_PLACEMENT_3D('',#50957,#41239,#41240);
#35498=AXIS2_PLACEMENT_3D('',#50960,#41243,#41244);
#35499=AXIS2_PLACEMENT_3D('',#50963,#41247,#41248);
#35500=AXIS2_PLACEMENT_3D('',#50965,#41250,#41251);
#35501=AXIS2_PLACEMENT_3D('',#50966,#41252,#41253);
#35502=AXIS2_PLACEMENT_3D('',#50967,#41254,#41255);
#35503=AXIS2_PLACEMENT_3D('',#50974,#41259,#41260);
#35504=AXIS2_PLACEMENT_3D('',#50981,#41264,#41265);
#35505=AXIS2_PLACEMENT_3D('',#50988,#41269,#41270);
#35506=AXIS2_PLACEMENT_3D('',#50991,#41273,#41274);
#35507=AXIS2_PLACEMENT_3D('',#50998,#41278,#41279);
#35508=AXIS2_PLACEMENT_3D('',#51001,#41282,#41283);
#35509=AXIS2_PLACEMENT_3D('',#51004,#41286,#41287);
#35510=AXIS2_PLACEMENT_3D('',#51007,#41290,#41291);
#35511=AXIS2_PLACEMENT_3D('',#51010,#41294,#41295);
#35512=AXIS2_PLACEMENT_3D('',#51013,#41298,#41299);
#35513=AXIS2_PLACEMENT_3D('',#51016,#41302,#41303);
#35514=AXIS2_PLACEMENT_3D('',#51019,#41306,#41307);
#35515=AXIS2_PLACEMENT_3D('',#51020,#41308,#41309);
#35516=AXIS2_PLACEMENT_3D('',#51021,#41310,#41311);
#35517=AXIS2_PLACEMENT_3D('',#51022,#41312,#41313);
#35518=AXIS2_PLACEMENT_3D('',#51029,#41317,#41318);
#35519=AXIS2_PLACEMENT_3D('',#51037,#41323,#41324);
#35520=AXIS2_PLACEMENT_3D('',#51040,#41327,#41328);
#35521=AXIS2_PLACEMENT_3D('',#51047,#41332,#41333);
#35522=AXIS2_PLACEMENT_3D('',#51055,#41338,#41339);
#35523=AXIS2_PLACEMENT_3D('',#51058,#41342,#41343);
#35524=AXIS2_PLACEMENT_3D('',#51061,#41346,#41347);
#35525=AXIS2_PLACEMENT_3D('',#51066,#41351,#41352);
#35526=AXIS2_PLACEMENT_3D('',#51068,#41354,#41355);
#35527=AXIS2_PLACEMENT_3D('',#51072,#41358,#41359);
#35528=AXIS2_PLACEMENT_3D('',#51075,#41362,#41363);
#35529=AXIS2_PLACEMENT_3D('',#51076,#41364,#41365);
#35530=AXIS2_PLACEMENT_3D('',#51077,#41366,#41367);
#35531=AXIS2_PLACEMENT_3D('',#51084,#41371,#41372);
#35532=AXIS2_PLACEMENT_3D('',#51091,#41376,#41377);
#35533=AXIS2_PLACEMENT_3D('',#51098,#41381,#41382);
#35534=AXIS2_PLACEMENT_3D('',#51101,#41385,#41386);
#35535=AXIS2_PLACEMENT_3D('',#51108,#41390,#41391);
#35536=AXIS2_PLACEMENT_3D('',#51111,#41394,#41395);
#35537=AXIS2_PLACEMENT_3D('',#51114,#41398,#41399);
#35538=AXIS2_PLACEMENT_3D('',#51117,#41402,#41403);
#35539=AXIS2_PLACEMENT_3D('',#51120,#41406,#41407);
#35540=AXIS2_PLACEMENT_3D('',#51123,#41410,#41411);
#35541=AXIS2_PLACEMENT_3D('',#51126,#41414,#41415);
#35542=AXIS2_PLACEMENT_3D('',#51129,#41418,#41419);
#35543=AXIS2_PLACEMENT_3D('',#51130,#41420,#41421);
#35544=AXIS2_PLACEMENT_3D('',#51131,#41422,#41423);
#35545=AXIS2_PLACEMENT_3D('',#51132,#41424,#41425);
#35546=AXIS2_PLACEMENT_3D('',#51139,#41429,#41430);
#35547=AXIS2_PLACEMENT_3D('',#51146,#41434,#41435);
#35548=AXIS2_PLACEMENT_3D('',#51153,#41439,#41440);
#35549=AXIS2_PLACEMENT_3D('',#51156,#41443,#41444);
#35550=AXIS2_PLACEMENT_3D('',#51163,#41448,#41449);
#35551=AXIS2_PLACEMENT_3D('',#51166,#41452,#41453);
#35552=AXIS2_PLACEMENT_3D('',#51169,#41456,#41457);
#35553=AXIS2_PLACEMENT_3D('',#51172,#41460,#41461);
#35554=AXIS2_PLACEMENT_3D('',#51175,#41464,#41465);
#35555=AXIS2_PLACEMENT_3D('',#51178,#41468,#41469);
#35556=AXIS2_PLACEMENT_3D('',#51181,#41472,#41473);
#35557=AXIS2_PLACEMENT_3D('',#51184,#41476,#41477);
#35558=AXIS2_PLACEMENT_3D('',#51185,#41478,#41479);
#35559=AXIS2_PLACEMENT_3D('',#51186,#41480,#41481);
#35560=AXIS2_PLACEMENT_3D('',#51187,#41482,#41483);
#35561=AXIS2_PLACEMENT_3D('',#51195,#41488,#41489);
#35562=AXIS2_PLACEMENT_3D('',#51199,#41492,#41493);
#35563=AXIS2_PLACEMENT_3D('',#51205,#41497,#41498);
#35564=AXIS2_PLACEMENT_3D('',#51211,#41502,#41503);
#35565=AXIS2_PLACEMENT_3D('',#51215,#41506,#41507);
#35566=AXIS2_PLACEMENT_3D('',#51219,#41510,#41511);
#35567=AXIS2_PLACEMENT_3D('',#51222,#41514,#41515);
#35568=AXIS2_PLACEMENT_3D('',#51229,#41519,#41520);
#35569=AXIS2_PLACEMENT_3D('',#51232,#41523,#41524);
#35570=AXIS2_PLACEMENT_3D('',#51235,#41527,#41528);
#35571=AXIS2_PLACEMENT_3D('',#51238,#41531,#41532);
#35572=AXIS2_PLACEMENT_3D('',#51240,#41534,#41535);
#35573=AXIS2_PLACEMENT_3D('',#51241,#41536,#41537);
#35574=AXIS2_PLACEMENT_3D('',#51242,#41538,#41539);
#35575=AXIS2_PLACEMENT_3D('',#51249,#41543,#41544);
#35576=AXIS2_PLACEMENT_3D('',#51256,#41548,#41549);
#35577=AXIS2_PLACEMENT_3D('',#51263,#41553,#41554);
#35578=AXIS2_PLACEMENT_3D('',#51266,#41557,#41558);
#35579=AXIS2_PLACEMENT_3D('',#51273,#41562,#41563);
#35580=AXIS2_PLACEMENT_3D('',#51276,#41566,#41567);
#35581=AXIS2_PLACEMENT_3D('',#51279,#41570,#41571);
#35582=AXIS2_PLACEMENT_3D('',#51282,#41574,#41575);
#35583=AXIS2_PLACEMENT_3D('',#51285,#41578,#41579);
#35584=AXIS2_PLACEMENT_3D('',#51288,#41582,#41583);
#35585=AXIS2_PLACEMENT_3D('',#51291,#41586,#41587);
#35586=AXIS2_PLACEMENT_3D('',#51294,#41590,#41591);
#35587=AXIS2_PLACEMENT_3D('',#51295,#41592,#41593);
#35588=AXIS2_PLACEMENT_3D('',#51296,#41594,#41595);
#35589=AXIS2_PLACEMENT_3D('',#51297,#41596,#41597);
#35590=AXIS2_PLACEMENT_3D('',#51304,#41601,#41602);
#35591=AXIS2_PLACEMENT_3D('',#51312,#41607,#41608);
#35592=AXIS2_PLACEMENT_3D('',#51315,#41611,#41612);
#35593=AXIS2_PLACEMENT_3D('',#51322,#41616,#41617);
#35594=AXIS2_PLACEMENT_3D('',#51330,#41622,#41623);
#35595=AXIS2_PLACEMENT_3D('',#51333,#41626,#41627);
#35596=AXIS2_PLACEMENT_3D('',#51336,#41630,#41631);
#35597=AXIS2_PLACEMENT_3D('',#51341,#41635,#41636);
#35598=AXIS2_PLACEMENT_3D('',#51343,#41638,#41639);
#35599=AXIS2_PLACEMENT_3D('',#51347,#41642,#41643);
#35600=AXIS2_PLACEMENT_3D('',#51350,#41646,#41647);
#35601=AXIS2_PLACEMENT_3D('',#51351,#41648,#41649);
#35602=AXIS2_PLACEMENT_3D('',#51352,#41650,#41651);
#35603=AXIS2_PLACEMENT_3D('',#51359,#41655,#41656);
#35604=AXIS2_PLACEMENT_3D('',#51366,#41660,#41661);
#35605=AXIS2_PLACEMENT_3D('',#51373,#41665,#41666);
#35606=AXIS2_PLACEMENT_3D('',#51376,#41669,#41670);
#35607=AXIS2_PLACEMENT_3D('',#51383,#41674,#41675);
#35608=AXIS2_PLACEMENT_3D('',#51386,#41678,#41679);
#35609=AXIS2_PLACEMENT_3D('',#51389,#41682,#41683);
#35610=AXIS2_PLACEMENT_3D('',#51392,#41686,#41687);
#35611=AXIS2_PLACEMENT_3D('',#51395,#41690,#41691);
#35612=AXIS2_PLACEMENT_3D('',#51398,#41694,#41695);
#35613=AXIS2_PLACEMENT_3D('',#51401,#41698,#41699);
#35614=AXIS2_PLACEMENT_3D('',#51404,#41702,#41703);
#35615=AXIS2_PLACEMENT_3D('',#51405,#41704,#41705);
#35616=AXIS2_PLACEMENT_3D('',#51406,#41706,#41707);
#35617=AXIS2_PLACEMENT_3D('',#51407,#41708,#41709);
#35618=AXIS2_PLACEMENT_3D('',#51414,#41713,#41714);
#35619=AXIS2_PLACEMENT_3D('',#51421,#41718,#41719);
#35620=AXIS2_PLACEMENT_3D('',#51428,#41723,#41724);
#35621=AXIS2_PLACEMENT_3D('',#51431,#41727,#41728);
#35622=AXIS2_PLACEMENT_3D('',#51438,#41732,#41733);
#35623=AXIS2_PLACEMENT_3D('',#51441,#41736,#41737);
#35624=AXIS2_PLACEMENT_3D('',#51444,#41740,#41741);
#35625=AXIS2_PLACEMENT_3D('',#51447,#41744,#41745);
#35626=AXIS2_PLACEMENT_3D('',#51450,#41748,#41749);
#35627=AXIS2_PLACEMENT_3D('',#51453,#41752,#41753);
#35628=AXIS2_PLACEMENT_3D('',#51456,#41756,#41757);
#35629=AXIS2_PLACEMENT_3D('',#51459,#41760,#41761);
#35630=AXIS2_PLACEMENT_3D('',#51460,#41762,#41763);
#35631=AXIS2_PLACEMENT_3D('',#51461,#41764,#41765);
#35632=AXIS2_PLACEMENT_3D('',#51462,#41766,#41767);
#35633=AXIS2_PLACEMENT_3D('',#51470,#41772,#41773);
#35634=AXIS2_PLACEMENT_3D('',#51474,#41776,#41777);
#35635=AXIS2_PLACEMENT_3D('',#51480,#41781,#41782);
#35636=AXIS2_PLACEMENT_3D('',#51486,#41786,#41787);
#35637=AXIS2_PLACEMENT_3D('',#51490,#41790,#41791);
#35638=AXIS2_PLACEMENT_3D('',#51494,#41794,#41795);
#35639=AXIS2_PLACEMENT_3D('',#51497,#41798,#41799);
#35640=AXIS2_PLACEMENT_3D('',#51504,#41803,#41804);
#35641=AXIS2_PLACEMENT_3D('',#51507,#41807,#41808);
#35642=AXIS2_PLACEMENT_3D('',#51510,#41811,#41812);
#35643=AXIS2_PLACEMENT_3D('',#51513,#41815,#41816);
#35644=AXIS2_PLACEMENT_3D('',#51515,#41818,#41819);
#35645=AXIS2_PLACEMENT_3D('',#51516,#41820,#41821);
#35646=AXIS2_PLACEMENT_3D('',#51517,#41822,#41823);
#35647=AXIS2_PLACEMENT_3D('',#51524,#41827,#41828);
#35648=AXIS2_PLACEMENT_3D('',#51531,#41832,#41833);
#35649=AXIS2_PLACEMENT_3D('',#51538,#41837,#41838);
#35650=AXIS2_PLACEMENT_3D('',#51541,#41841,#41842);
#35651=AXIS2_PLACEMENT_3D('',#51548,#41846,#41847);
#35652=AXIS2_PLACEMENT_3D('',#51551,#41850,#41851);
#35653=AXIS2_PLACEMENT_3D('',#51554,#41854,#41855);
#35654=AXIS2_PLACEMENT_3D('',#51557,#41858,#41859);
#35655=AXIS2_PLACEMENT_3D('',#51560,#41862,#41863);
#35656=AXIS2_PLACEMENT_3D('',#51563,#41866,#41867);
#35657=AXIS2_PLACEMENT_3D('',#51566,#41870,#41871);
#35658=AXIS2_PLACEMENT_3D('',#51569,#41874,#41875);
#35659=AXIS2_PLACEMENT_3D('',#51570,#41876,#41877);
#35660=AXIS2_PLACEMENT_3D('',#51571,#41878,#41879);
#35661=AXIS2_PLACEMENT_3D('',#51572,#41880,#41881);
#35662=AXIS2_PLACEMENT_3D('',#51579,#41885,#41886);
#35663=AXIS2_PLACEMENT_3D('',#51587,#41891,#41892);
#35664=AXIS2_PLACEMENT_3D('',#51590,#41895,#41896);
#35665=AXIS2_PLACEMENT_3D('',#51597,#41900,#41901);
#35666=AXIS2_PLACEMENT_3D('',#51605,#41906,#41907);
#35667=AXIS2_PLACEMENT_3D('',#51608,#41910,#41911);
#35668=AXIS2_PLACEMENT_3D('',#51611,#41914,#41915);
#35669=AXIS2_PLACEMENT_3D('',#51616,#41919,#41920);
#35670=AXIS2_PLACEMENT_3D('',#51618,#41922,#41923);
#35671=AXIS2_PLACEMENT_3D('',#51622,#41926,#41927);
#35672=AXIS2_PLACEMENT_3D('',#51625,#41930,#41931);
#35673=AXIS2_PLACEMENT_3D('',#51626,#41932,#41933);
#35674=AXIS2_PLACEMENT_3D('',#51627,#41934,#41935);
#35675=AXIS2_PLACEMENT_3D('',#51634,#41939,#41940);
#35676=AXIS2_PLACEMENT_3D('',#51641,#41944,#41945);
#35677=AXIS2_PLACEMENT_3D('',#51648,#41949,#41950);
#35678=AXIS2_PLACEMENT_3D('',#51651,#41953,#41954);
#35679=AXIS2_PLACEMENT_3D('',#51658,#41958,#41959);
#35680=AXIS2_PLACEMENT_3D('',#51661,#41962,#41963);
#35681=AXIS2_PLACEMENT_3D('',#51664,#41966,#41967);
#35682=AXIS2_PLACEMENT_3D('',#51667,#41970,#41971);
#35683=AXIS2_PLACEMENT_3D('',#51670,#41974,#41975);
#35684=AXIS2_PLACEMENT_3D('',#51673,#41978,#41979);
#35685=AXIS2_PLACEMENT_3D('',#51676,#41982,#41983);
#35686=AXIS2_PLACEMENT_3D('',#51679,#41986,#41987);
#35687=AXIS2_PLACEMENT_3D('',#51680,#41988,#41989);
#35688=AXIS2_PLACEMENT_3D('',#51681,#41990,#41991);
#35689=AXIS2_PLACEMENT_3D('',#51682,#41992,#41993);
#35690=AXIS2_PLACEMENT_3D('',#51689,#41997,#41998);
#35691=AXIS2_PLACEMENT_3D('',#51696,#42002,#42003);
#35692=AXIS2_PLACEMENT_3D('',#51703,#42007,#42008);
#35693=AXIS2_PLACEMENT_3D('',#51706,#42011,#42012);
#35694=AXIS2_PLACEMENT_3D('',#51713,#42016,#42017);
#35695=AXIS2_PLACEMENT_3D('',#51716,#42020,#42021);
#35696=AXIS2_PLACEMENT_3D('',#51719,#42024,#42025);
#35697=AXIS2_PLACEMENT_3D('',#51722,#42028,#42029);
#35698=AXIS2_PLACEMENT_3D('',#51725,#42032,#42033);
#35699=AXIS2_PLACEMENT_3D('',#51728,#42036,#42037);
#35700=AXIS2_PLACEMENT_3D('',#51731,#42040,#42041);
#35701=AXIS2_PLACEMENT_3D('',#51734,#42044,#42045);
#35702=AXIS2_PLACEMENT_3D('',#51735,#42046,#42047);
#35703=AXIS2_PLACEMENT_3D('',#51736,#42048,#42049);
#35704=AXIS2_PLACEMENT_3D('',#51737,#42050,#42051);
#35705=AXIS2_PLACEMENT_3D('',#51745,#42056,#42057);
#35706=AXIS2_PLACEMENT_3D('',#51749,#42060,#42061);
#35707=AXIS2_PLACEMENT_3D('',#51755,#42065,#42066);
#35708=AXIS2_PLACEMENT_3D('',#51761,#42070,#42071);
#35709=AXIS2_PLACEMENT_3D('',#51765,#42074,#42075);
#35710=AXIS2_PLACEMENT_3D('',#51769,#42078,#42079);
#35711=AXIS2_PLACEMENT_3D('',#51772,#42082,#42083);
#35712=AXIS2_PLACEMENT_3D('',#51779,#42087,#42088);
#35713=AXIS2_PLACEMENT_3D('',#51782,#42091,#42092);
#35714=AXIS2_PLACEMENT_3D('',#51785,#42095,#42096);
#35715=AXIS2_PLACEMENT_3D('',#51788,#42099,#42100);
#35716=AXIS2_PLACEMENT_3D('',#51790,#42102,#42103);
#35717=AXIS2_PLACEMENT_3D('',#51791,#42104,#42105);
#35718=AXIS2_PLACEMENT_3D('',#51792,#42106,#42107);
#35719=AXIS2_PLACEMENT_3D('',#51799,#42111,#42112);
#35720=AXIS2_PLACEMENT_3D('',#51806,#42116,#42117);
#35721=AXIS2_PLACEMENT_3D('',#51813,#42121,#42122);
#35722=AXIS2_PLACEMENT_3D('',#51816,#42125,#42126);
#35723=AXIS2_PLACEMENT_3D('',#51823,#42130,#42131);
#35724=AXIS2_PLACEMENT_3D('',#51826,#42134,#42135);
#35725=AXIS2_PLACEMENT_3D('',#51829,#42138,#42139);
#35726=AXIS2_PLACEMENT_3D('',#51832,#42142,#42143);
#35727=AXIS2_PLACEMENT_3D('',#51835,#42146,#42147);
#35728=AXIS2_PLACEMENT_3D('',#51838,#42150,#42151);
#35729=AXIS2_PLACEMENT_3D('',#51841,#42154,#42155);
#35730=AXIS2_PLACEMENT_3D('',#51844,#42158,#42159);
#35731=AXIS2_PLACEMENT_3D('',#51845,#42160,#42161);
#35732=AXIS2_PLACEMENT_3D('',#51846,#42162,#42163);
#35733=AXIS2_PLACEMENT_3D('',#51847,#42164,#42165);
#35734=AXIS2_PLACEMENT_3D('',#51854,#42169,#42170);
#35735=AXIS2_PLACEMENT_3D('',#51862,#42175,#42176);
#35736=AXIS2_PLACEMENT_3D('',#51865,#42179,#42180);
#35737=AXIS2_PLACEMENT_3D('',#51872,#42184,#42185);
#35738=AXIS2_PLACEMENT_3D('',#51880,#42190,#42191);
#35739=AXIS2_PLACEMENT_3D('',#51883,#42194,#42195);
#35740=AXIS2_PLACEMENT_3D('',#51886,#42198,#42199);
#35741=AXIS2_PLACEMENT_3D('',#51891,#42203,#42204);
#35742=AXIS2_PLACEMENT_3D('',#51893,#42206,#42207);
#35743=AXIS2_PLACEMENT_3D('',#51897,#42210,#42211);
#35744=AXIS2_PLACEMENT_3D('',#51900,#42214,#42215);
#35745=AXIS2_PLACEMENT_3D('',#51901,#42216,#42217);
#35746=AXIS2_PLACEMENT_3D('',#51902,#42218,#42219);
#35747=AXIS2_PLACEMENT_3D('',#51909,#42223,#42224);
#35748=AXIS2_PLACEMENT_3D('',#51916,#42228,#42229);
#35749=AXIS2_PLACEMENT_3D('',#51923,#42233,#42234);
#35750=AXIS2_PLACEMENT_3D('',#51926,#42237,#42238);
#35751=AXIS2_PLACEMENT_3D('',#51933,#42242,#42243);
#35752=AXIS2_PLACEMENT_3D('',#51936,#42246,#42247);
#35753=AXIS2_PLACEMENT_3D('',#51939,#42250,#42251);
#35754=AXIS2_PLACEMENT_3D('',#51942,#42254,#42255);
#35755=AXIS2_PLACEMENT_3D('',#51945,#42258,#42259);
#35756=AXIS2_PLACEMENT_3D('',#51948,#42262,#42263);
#35757=AXIS2_PLACEMENT_3D('',#51951,#42266,#42267);
#35758=AXIS2_PLACEMENT_3D('',#51954,#42270,#42271);
#35759=AXIS2_PLACEMENT_3D('',#51955,#42272,#42273);
#35760=AXIS2_PLACEMENT_3D('',#51956,#42274,#42275);
#35761=AXIS2_PLACEMENT_3D('',#51957,#42276,#42277);
#35762=AXIS2_PLACEMENT_3D('',#51964,#42281,#42282);
#35763=AXIS2_PLACEMENT_3D('',#51971,#42286,#42287);
#35764=AXIS2_PLACEMENT_3D('',#51978,#42291,#42292);
#35765=AXIS2_PLACEMENT_3D('',#51981,#42295,#42296);
#35766=AXIS2_PLACEMENT_3D('',#51988,#42300,#42301);
#35767=AXIS2_PLACEMENT_3D('',#51991,#42304,#42305);
#35768=AXIS2_PLACEMENT_3D('',#51994,#42308,#42309);
#35769=AXIS2_PLACEMENT_3D('',#51997,#42312,#42313);
#35770=AXIS2_PLACEMENT_3D('',#52000,#42316,#42317);
#35771=AXIS2_PLACEMENT_3D('',#52003,#42320,#42321);
#35772=AXIS2_PLACEMENT_3D('',#52006,#42324,#42325);
#35773=AXIS2_PLACEMENT_3D('',#52009,#42328,#42329);
#35774=AXIS2_PLACEMENT_3D('',#52010,#42330,#42331);
#35775=AXIS2_PLACEMENT_3D('',#52011,#42332,#42333);
#35776=AXIS2_PLACEMENT_3D('',#52012,#42334,#42335);
#35777=AXIS2_PLACEMENT_3D('',#52020,#42340,#42341);
#35778=AXIS2_PLACEMENT_3D('',#52024,#42344,#42345);
#35779=AXIS2_PLACEMENT_3D('',#52030,#42349,#42350);
#35780=AXIS2_PLACEMENT_3D('',#52036,#42354,#42355);
#35781=AXIS2_PLACEMENT_3D('',#52040,#42358,#42359);
#35782=AXIS2_PLACEMENT_3D('',#52044,#42362,#42363);
#35783=AXIS2_PLACEMENT_3D('',#52047,#42366,#42367);
#35784=AXIS2_PLACEMENT_3D('',#52054,#42371,#42372);
#35785=AXIS2_PLACEMENT_3D('',#52057,#42375,#42376);
#35786=AXIS2_PLACEMENT_3D('',#52060,#42379,#42380);
#35787=AXIS2_PLACEMENT_3D('',#52063,#42383,#42384);
#35788=AXIS2_PLACEMENT_3D('',#52065,#42386,#42387);
#35789=AXIS2_PLACEMENT_3D('',#52066,#42388,#42389);
#35790=AXIS2_PLACEMENT_3D('',#52067,#42390,#42391);
#35791=AXIS2_PLACEMENT_3D('',#52074,#42395,#42396);
#35792=AXIS2_PLACEMENT_3D('',#52081,#42400,#42401);
#35793=AXIS2_PLACEMENT_3D('',#52088,#42405,#42406);
#35794=AXIS2_PLACEMENT_3D('',#52091,#42409,#42410);
#35795=AXIS2_PLACEMENT_3D('',#52098,#42414,#42415);
#35796=AXIS2_PLACEMENT_3D('',#52101,#42418,#42419);
#35797=AXIS2_PLACEMENT_3D('',#52104,#42422,#42423);
#35798=AXIS2_PLACEMENT_3D('',#52107,#42426,#42427);
#35799=AXIS2_PLACEMENT_3D('',#52110,#42430,#42431);
#35800=AXIS2_PLACEMENT_3D('',#52113,#42434,#42435);
#35801=AXIS2_PLACEMENT_3D('',#52116,#42438,#42439);
#35802=AXIS2_PLACEMENT_3D('',#52119,#42442,#42443);
#35803=AXIS2_PLACEMENT_3D('',#52120,#42444,#42445);
#35804=AXIS2_PLACEMENT_3D('',#52121,#42446,#42447);
#35805=AXIS2_PLACEMENT_3D('',#52122,#42448,#42449);
#35806=AXIS2_PLACEMENT_3D('',#52129,#42453,#42454);
#35807=AXIS2_PLACEMENT_3D('',#52137,#42459,#42460);
#35808=AXIS2_PLACEMENT_3D('',#52140,#42463,#42464);
#35809=AXIS2_PLACEMENT_3D('',#52147,#42468,#42469);
#35810=AXIS2_PLACEMENT_3D('',#52155,#42474,#42475);
#35811=AXIS2_PLACEMENT_3D('',#52158,#42478,#42479);
#35812=AXIS2_PLACEMENT_3D('',#52161,#42482,#42483);
#35813=AXIS2_PLACEMENT_3D('',#52166,#42487,#42488);
#35814=AXIS2_PLACEMENT_3D('',#52168,#42490,#42491);
#35815=AXIS2_PLACEMENT_3D('',#52172,#42494,#42495);
#35816=AXIS2_PLACEMENT_3D('',#52175,#42498,#42499);
#35817=AXIS2_PLACEMENT_3D('',#52176,#42500,#42501);
#35818=AXIS2_PLACEMENT_3D('',#52177,#42502,#42503);
#35819=AXIS2_PLACEMENT_3D('',#52184,#42507,#42508);
#35820=AXIS2_PLACEMENT_3D('',#52191,#42512,#42513);
#35821=AXIS2_PLACEMENT_3D('',#52198,#42517,#42518);
#35822=AXIS2_PLACEMENT_3D('',#52201,#42521,#42522);
#35823=AXIS2_PLACEMENT_3D('',#52208,#42526,#42527);
#35824=AXIS2_PLACEMENT_3D('',#52211,#42530,#42531);
#35825=AXIS2_PLACEMENT_3D('',#52214,#42534,#42535);
#35826=AXIS2_PLACEMENT_3D('',#52217,#42538,#42539);
#35827=AXIS2_PLACEMENT_3D('',#52220,#42542,#42543);
#35828=AXIS2_PLACEMENT_3D('',#52223,#42546,#42547);
#35829=AXIS2_PLACEMENT_3D('',#52226,#42550,#42551);
#35830=AXIS2_PLACEMENT_3D('',#52229,#42554,#42555);
#35831=AXIS2_PLACEMENT_3D('',#52230,#42556,#42557);
#35832=AXIS2_PLACEMENT_3D('',#52231,#42558,#42559);
#35833=AXIS2_PLACEMENT_3D('',#52232,#42560,#42561);
#35834=AXIS2_PLACEMENT_3D('',#52239,#42565,#42566);
#35835=AXIS2_PLACEMENT_3D('',#52246,#42570,#42571);
#35836=AXIS2_PLACEMENT_3D('',#52253,#42575,#42576);
#35837=AXIS2_PLACEMENT_3D('',#52256,#42579,#42580);
#35838=AXIS2_PLACEMENT_3D('',#52263,#42584,#42585);
#35839=AXIS2_PLACEMENT_3D('',#52266,#42588,#42589);
#35840=AXIS2_PLACEMENT_3D('',#52269,#42592,#42593);
#35841=AXIS2_PLACEMENT_3D('',#52272,#42596,#42597);
#35842=AXIS2_PLACEMENT_3D('',#52275,#42600,#42601);
#35843=AXIS2_PLACEMENT_3D('',#52278,#42604,#42605);
#35844=AXIS2_PLACEMENT_3D('',#52281,#42608,#42609);
#35845=AXIS2_PLACEMENT_3D('',#52284,#42612,#42613);
#35846=AXIS2_PLACEMENT_3D('',#52285,#42614,#42615);
#35847=AXIS2_PLACEMENT_3D('',#52286,#42616,#42617);
#35848=AXIS2_PLACEMENT_3D('',#52287,#42618,#42619);
#35849=AXIS2_PLACEMENT_3D('',#52295,#42624,#42625);
#35850=AXIS2_PLACEMENT_3D('',#52299,#42628,#42629);
#35851=AXIS2_PLACEMENT_3D('',#52305,#42633,#42634);
#35852=AXIS2_PLACEMENT_3D('',#52311,#42638,#42639);
#35853=AXIS2_PLACEMENT_3D('',#52315,#42642,#42643);
#35854=AXIS2_PLACEMENT_3D('',#52319,#42646,#42647);
#35855=AXIS2_PLACEMENT_3D('',#52322,#42650,#42651);
#35856=AXIS2_PLACEMENT_3D('',#52329,#42655,#42656);
#35857=AXIS2_PLACEMENT_3D('',#52332,#42659,#42660);
#35858=AXIS2_PLACEMENT_3D('',#52335,#42663,#42664);
#35859=AXIS2_PLACEMENT_3D('',#52338,#42667,#42668);
#35860=AXIS2_PLACEMENT_3D('',#52340,#42670,#42671);
#35861=AXIS2_PLACEMENT_3D('',#52341,#42672,#42673);
#35862=AXIS2_PLACEMENT_3D('',#52342,#42674,#42675);
#35863=AXIS2_PLACEMENT_3D('',#52349,#42679,#42680);
#35864=AXIS2_PLACEMENT_3D('',#52356,#42684,#42685);
#35865=AXIS2_PLACEMENT_3D('',#52363,#42689,#42690);
#35866=AXIS2_PLACEMENT_3D('',#52366,#42693,#42694);
#35867=AXIS2_PLACEMENT_3D('',#52373,#42698,#42699);
#35868=AXIS2_PLACEMENT_3D('',#52376,#42702,#42703);
#35869=AXIS2_PLACEMENT_3D('',#52379,#42706,#42707);
#35870=AXIS2_PLACEMENT_3D('',#52382,#42710,#42711);
#35871=AXIS2_PLACEMENT_3D('',#52385,#42714,#42715);
#35872=AXIS2_PLACEMENT_3D('',#52388,#42718,#42719);
#35873=AXIS2_PLACEMENT_3D('',#52391,#42722,#42723);
#35874=AXIS2_PLACEMENT_3D('',#52394,#42726,#42727);
#35875=AXIS2_PLACEMENT_3D('',#52395,#42728,#42729);
#35876=AXIS2_PLACEMENT_3D('',#52396,#42730,#42731);
#35877=AXIS2_PLACEMENT_3D('',#52397,#42732,#42733);
#35878=AXIS2_PLACEMENT_3D('',#52404,#42737,#42738);
#35879=AXIS2_PLACEMENT_3D('',#52412,#42743,#42744);
#35880=AXIS2_PLACEMENT_3D('',#52415,#42747,#42748);
#35881=AXIS2_PLACEMENT_3D('',#52422,#42752,#42753);
#35882=AXIS2_PLACEMENT_3D('',#52430,#42758,#42759);
#35883=AXIS2_PLACEMENT_3D('',#52433,#42762,#42763);
#35884=AXIS2_PLACEMENT_3D('',#52436,#42766,#42767);
#35885=AXIS2_PLACEMENT_3D('',#52441,#42771,#42772);
#35886=AXIS2_PLACEMENT_3D('',#52443,#42774,#42775);
#35887=AXIS2_PLACEMENT_3D('',#52447,#42778,#42779);
#35888=AXIS2_PLACEMENT_3D('',#52450,#42782,#42783);
#35889=AXIS2_PLACEMENT_3D('',#52451,#42784,#42785);
#35890=AXIS2_PLACEMENT_3D('',#52452,#42786,#42787);
#35891=AXIS2_PLACEMENT_3D('',#52459,#42791,#42792);
#35892=AXIS2_PLACEMENT_3D('',#52466,#42796,#42797);
#35893=AXIS2_PLACEMENT_3D('',#52473,#42801,#42802);
#35894=AXIS2_PLACEMENT_3D('',#52476,#42805,#42806);
#35895=AXIS2_PLACEMENT_3D('',#52483,#42810,#42811);
#35896=AXIS2_PLACEMENT_3D('',#52486,#42814,#42815);
#35897=AXIS2_PLACEMENT_3D('',#52489,#42818,#42819);
#35898=AXIS2_PLACEMENT_3D('',#52492,#42822,#42823);
#35899=AXIS2_PLACEMENT_3D('',#52495,#42826,#42827);
#35900=AXIS2_PLACEMENT_3D('',#52498,#42830,#42831);
#35901=AXIS2_PLACEMENT_3D('',#52501,#42834,#42835);
#35902=AXIS2_PLACEMENT_3D('',#52504,#42838,#42839);
#35903=AXIS2_PLACEMENT_3D('',#52505,#42840,#42841);
#35904=AXIS2_PLACEMENT_3D('',#52506,#42842,#42843);
#35905=AXIS2_PLACEMENT_3D('',#52507,#42844,#42845);
#35906=AXIS2_PLACEMENT_3D('',#52514,#42849,#42850);
#35907=AXIS2_PLACEMENT_3D('',#52521,#42854,#42855);
#35908=AXIS2_PLACEMENT_3D('',#52528,#42859,#42860);
#35909=AXIS2_PLACEMENT_3D('',#52531,#42863,#42864);
#35910=AXIS2_PLACEMENT_3D('',#52538,#42868,#42869);
#35911=AXIS2_PLACEMENT_3D('',#52541,#42872,#42873);
#35912=AXIS2_PLACEMENT_3D('',#52544,#42876,#42877);
#35913=AXIS2_PLACEMENT_3D('',#52547,#42880,#42881);
#35914=AXIS2_PLACEMENT_3D('',#52550,#42884,#42885);
#35915=AXIS2_PLACEMENT_3D('',#52553,#42888,#42889);
#35916=AXIS2_PLACEMENT_3D('',#52556,#42892,#42893);
#35917=AXIS2_PLACEMENT_3D('',#52559,#42896,#42897);
#35918=AXIS2_PLACEMENT_3D('',#52560,#42898,#42899);
#35919=AXIS2_PLACEMENT_3D('',#52561,#42900,#42901);
#35920=AXIS2_PLACEMENT_3D('',#52562,#42902,#42903);
#35921=AXIS2_PLACEMENT_3D('',#52565,#42904,#42905);
#35922=AXIS2_PLACEMENT_3D('',#52566,#42906,#42907);
#35923=AXIS2_PLACEMENT_3D('',#52570,#42909,#42910);
#35924=AXIS2_PLACEMENT_3D('',#52571,#42911,#42912);
#35925=AXIS2_PLACEMENT_3D('',#52572,#42913,#42914);
#35926=AXIS2_PLACEMENT_3D('',#52576,#42916,#42917);
#35927=AXIS2_PLACEMENT_3D('',#52577,#42918,#42919);
#35928=AXIS2_PLACEMENT_3D('',#52578,#42920,#42921);
#35929=AXIS2_PLACEMENT_3D('',#52580,#42922,#42923);
#35930=AXIS2_PLACEMENT_3D('',#52582,#42925,#42926);
#35931=AXIS2_PLACEMENT_3D('',#52589,#42930,#42931);
#35932=AXIS2_PLACEMENT_3D('',#52596,#42935,#42936);
#35933=AXIS2_PLACEMENT_3D('',#52603,#42940,#42941);
#35934=AXIS2_PLACEMENT_3D('',#52606,#42944,#42945);
#35935=AXIS2_PLACEMENT_3D('',#52613,#42949,#42950);
#35936=AXIS2_PLACEMENT_3D('',#52616,#42953,#42954);
#35937=AXIS2_PLACEMENT_3D('',#52619,#42957,#42958);
#35938=AXIS2_PLACEMENT_3D('',#52622,#42961,#42962);
#35939=AXIS2_PLACEMENT_3D('',#52625,#42965,#42966);
#35940=AXIS2_PLACEMENT_3D('',#52628,#42969,#42970);
#35941=AXIS2_PLACEMENT_3D('',#52631,#42973,#42974);
#35942=AXIS2_PLACEMENT_3D('',#52634,#42977,#42978);
#35943=AXIS2_PLACEMENT_3D('',#52635,#42979,#42980);
#35944=AXIS2_PLACEMENT_3D('',#52636,#42981,#42982);
#35945=AXIS2_PLACEMENT_3D('',#52637,#42983,#42984);
#35946=AXIS2_PLACEMENT_3D('',#52644,#42988,#42989);
#35947=AXIS2_PLACEMENT_3D('',#52651,#42993,#42994);
#35948=AXIS2_PLACEMENT_3D('',#52658,#42998,#42999);
#35949=AXIS2_PLACEMENT_3D('',#52661,#43002,#43003);
#35950=AXIS2_PLACEMENT_3D('',#52668,#43007,#43008);
#35951=AXIS2_PLACEMENT_3D('',#52671,#43011,#43012);
#35952=AXIS2_PLACEMENT_3D('',#52674,#43015,#43016);
#35953=AXIS2_PLACEMENT_3D('',#52677,#43019,#43020);
#35954=AXIS2_PLACEMENT_3D('',#52680,#43023,#43024);
#35955=AXIS2_PLACEMENT_3D('',#52683,#43027,#43028);
#35956=AXIS2_PLACEMENT_3D('',#52686,#43031,#43032);
#35957=AXIS2_PLACEMENT_3D('',#52689,#43035,#43036);
#35958=AXIS2_PLACEMENT_3D('',#52690,#43037,#43038);
#35959=AXIS2_PLACEMENT_3D('',#52691,#43039,#43040);
#35960=AXIS2_PLACEMENT_3D('',#52692,#43041,#43042);
#35961=AXIS2_PLACEMENT_3D('',#52695,#43043,#43044);
#35962=AXIS2_PLACEMENT_3D('',#52696,#43045,#43046);
#35963=AXIS2_PLACEMENT_3D('',#52700,#43048,#43049);
#35964=AXIS2_PLACEMENT_3D('',#52701,#43050,#43051);
#35965=AXIS2_PLACEMENT_3D('',#52702,#43052,#43053);
#35966=AXIS2_PLACEMENT_3D('',#52706,#43055,#43056);
#35967=AXIS2_PLACEMENT_3D('',#52707,#43057,#43058);
#35968=AXIS2_PLACEMENT_3D('',#52708,#43059,#43060);
#35969=AXIS2_PLACEMENT_3D('',#52710,#43062,#43063);
#35970=AXIS2_PLACEMENT_3D('',#52712,#43064,#43065);
#35971=AXIS2_PLACEMENT_3D('',#52714,#43067,#43068);
#35972=AXIS2_PLACEMENT_3D('',#52716,#43069,#43070);
#35973=AXIS2_PLACEMENT_3D('',#52717,#43071,#43072);
#35974=AXIS2_PLACEMENT_3D('',#52719,#43073,#43074);
#35975=AXIS2_PLACEMENT_3D('',#52721,#43076,#43077);
#35976=AXIS2_PLACEMENT_3D('',#52724,#43079,#43080);
#35977=AXIS2_PLACEMENT_3D('',#52725,#43081,#43082);
#35978=AXIS2_PLACEMENT_3D('',#52727,#43084,#43085);
#35979=AXIS2_PLACEMENT_3D('',#52728,#43086,#43087);
#35980=AXIS2_PLACEMENT_3D('',#52729,#43088,#43089);
#35981=AXIS2_PLACEMENT_3D('',#52730,#43090,#43091);
#35982=AXIS2_PLACEMENT_3D('',#52731,#43092,#43093);
#35983=AXIS2_PLACEMENT_3D('',#52732,#43094,#43095);
#35984=AXIS2_PLACEMENT_3D('',#52733,#43096,#43097);
#35985=AXIS2_PLACEMENT_3D('',#52734,#43098,#43099);
#35986=AXIS2_PLACEMENT_3D('',#52735,#43100,#43101);
#35987=AXIS2_PLACEMENT_3D('',#52736,#43102,#43103);
#35988=AXIS2_PLACEMENT_3D('',#52737,#43104,#43105);
#35989=AXIS2_PLACEMENT_3D('',#52738,#43106,#43107);
#35990=AXIS2_PLACEMENT_3D('',#52739,#43108,#43109);
#35991=AXIS2_PLACEMENT_3D('',#52740,#43110,#43111);
#35992=AXIS2_PLACEMENT_3D('',#52741,#43112,#43113);
#35993=AXIS2_PLACEMENT_3D('',#52742,#43114,#43115);
#35994=AXIS2_PLACEMENT_3D('',#52743,#43116,#43117);
#35995=AXIS2_PLACEMENT_3D('',#52744,#43118,#43119);
#35996=AXIS2_PLACEMENT_3D('',#52745,#43120,#43121);
#35997=AXIS2_PLACEMENT_3D('',#52746,#43122,#43123);
#35998=AXIS2_PLACEMENT_3D('',#52747,#43124,#43125);
#35999=AXIS2_PLACEMENT_3D('',#52748,#43126,#43127);
#36000=AXIS2_PLACEMENT_3D('',#52749,#43128,#43129);
#36001=AXIS2_PLACEMENT_3D('',#52750,#43130,#43131);
#36002=AXIS2_PLACEMENT_3D('',#52751,#43132,#43133);
#36003=AXIS2_PLACEMENT_3D('',#52752,#43134,#43135);
#36004=AXIS2_PLACEMENT_3D('',#52753,#43136,#43137);
#36005=AXIS2_PLACEMENT_3D('',#52754,#43138,#43139);
#36006=AXIS2_PLACEMENT_3D('',#52755,#43140,#43141);
#36007=AXIS2_PLACEMENT_3D('',#52756,#43142,#43143);
#36008=AXIS2_PLACEMENT_3D('',#52757,#43144,#43145);
#36009=AXIS2_PLACEMENT_3D('',#52758,#43146,#43147);
#36010=AXIS2_PLACEMENT_3D('',#52759,#43148,#43149);
#36011=AXIS2_PLACEMENT_3D('',#52760,#43150,#43151);
#36012=AXIS2_PLACEMENT_3D('',#52761,#43152,#43153);
#36013=AXIS2_PLACEMENT_3D('',#52762,#43154,#43155);
#36014=AXIS2_PLACEMENT_3D('',#52763,#43156,#43157);
#36015=AXIS2_PLACEMENT_3D('',#52764,#43158,#43159);
#36016=AXIS2_PLACEMENT_3D('',#52765,#43160,#43161);
#36017=AXIS2_PLACEMENT_3D('',#52766,#43162,#43163);
#36018=AXIS2_PLACEMENT_3D('',#52767,#43164,#43165);
#36019=AXIS2_PLACEMENT_3D('',#52768,#43166,#43167);
#36020=AXIS2_PLACEMENT_3D('',#52769,#43168,#43169);
#36021=AXIS2_PLACEMENT_3D('',#52770,#43170,#43171);
#36022=AXIS2_PLACEMENT_3D('',#52771,#43172,#43173);
#36023=AXIS2_PLACEMENT_3D('',#52772,#43174,#43175);
#36024=AXIS2_PLACEMENT_3D('',#52773,#43176,#43177);
#36025=AXIS2_PLACEMENT_3D('',#52774,#43178,#43179);
#36026=AXIS2_PLACEMENT_3D('',#52775,#43180,#43181);
#36027=AXIS2_PLACEMENT_3D('',#52776,#43182,#43183);
#36028=AXIS2_PLACEMENT_3D('',#52777,#43184,#43185);
#36029=AXIS2_PLACEMENT_3D('',#52778,#43186,#43187);
#36030=AXIS2_PLACEMENT_3D('',#52779,#43188,#43189);
#36031=AXIS2_PLACEMENT_3D('',#52780,#43190,#43191);
#36032=AXIS2_PLACEMENT_3D('',#52781,#43192,#43193);
#36033=AXIS2_PLACEMENT_3D('',#52782,#43194,#43195);
#36034=AXIS2_PLACEMENT_3D('',#52783,#43196,#43197);
#36035=AXIS2_PLACEMENT_3D('',#52784,#43198,#43199);
#36036=AXIS2_PLACEMENT_3D('',#52785,#43200,#43201);
#36037=AXIS2_PLACEMENT_3D('',#52786,#43202,#43203);
#36038=AXIS2_PLACEMENT_3D('',#52787,#43204,#43205);
#36039=AXIS2_PLACEMENT_3D('',#52788,#43206,#43207);
#36040=AXIS2_PLACEMENT_3D('',#52789,#43208,#43209);
#36041=AXIS2_PLACEMENT_3D('',#52790,#43210,#43211);
#36042=AXIS2_PLACEMENT_3D('',#52791,#43212,#43213);
#36043=AXIS2_PLACEMENT_3D('',#52792,#43214,#43215);
#36044=AXIS2_PLACEMENT_3D('',#52793,#43216,#43217);
#36045=AXIS2_PLACEMENT_3D('',#52794,#43218,#43219);
#36046=AXIS2_PLACEMENT_3D('',#52795,#43220,#43221);
#36047=AXIS2_PLACEMENT_3D('',#52796,#43222,#43223);
#36048=AXIS2_PLACEMENT_3D('',#52797,#43224,#43225);
#36049=AXIS2_PLACEMENT_3D('',#52798,#43226,#43227);
#36050=AXIS2_PLACEMENT_3D('',#52799,#43228,#43229);
#36051=AXIS2_PLACEMENT_3D('',#52800,#43230,#43231);
#36052=AXIS2_PLACEMENT_3D('',#52801,#43232,#43233);
#36053=AXIS2_PLACEMENT_3D('',#52802,#43234,#43235);
#36054=AXIS2_PLACEMENT_3D('',#52803,#43236,#43237);
#36055=AXIS2_PLACEMENT_3D('',#52804,#43238,#43239);
#36056=AXIS2_PLACEMENT_3D('',#52805,#43240,#43241);
#36057=AXIS2_PLACEMENT_3D('',#52806,#43242,#43243);
#36058=AXIS2_PLACEMENT_3D('',#52807,#43244,#43245);
#36059=AXIS2_PLACEMENT_3D('',#52808,#43246,#43247);
#36060=AXIS2_PLACEMENT_3D('',#52809,#43248,#43249);
#36061=AXIS2_PLACEMENT_3D('',#52810,#43250,#43251);
#36062=AXIS2_PLACEMENT_3D('',#52811,#43252,#43253);
#36063=AXIS2_PLACEMENT_3D('',#52812,#43254,#43255);
#36064=AXIS2_PLACEMENT_3D('',#52813,#43256,#43257);
#36065=AXIS2_PLACEMENT_3D('',#52814,#43258,#43259);
#36066=AXIS2_PLACEMENT_3D('',#52815,#43260,#43261);
#36067=AXIS2_PLACEMENT_3D('',#52816,#43262,#43263);
#36068=AXIS2_PLACEMENT_3D('',#52817,#43264,#43265);
#36069=AXIS2_PLACEMENT_3D('',#52818,#43266,#43267);
#36070=AXIS2_PLACEMENT_3D('',#52819,#43268,#43269);
#36071=AXIS2_PLACEMENT_3D('',#52820,#43270,#43271);
#36072=AXIS2_PLACEMENT_3D('',#52821,#43272,#43273);
#36073=AXIS2_PLACEMENT_3D('',#52822,#43274,#43275);
#36074=AXIS2_PLACEMENT_3D('',#52823,#43276,#43277);
#36075=AXIS2_PLACEMENT_3D('',#52824,#43278,#43279);
#36076=AXIS2_PLACEMENT_3D('',#52825,#43280,#43281);
#36077=AXIS2_PLACEMENT_3D('',#52826,#43282,#43283);
#36078=AXIS2_PLACEMENT_3D('',#52827,#43284,#43285);
#36079=AXIS2_PLACEMENT_3D('',#52828,#43286,#43287);
#36080=AXIS2_PLACEMENT_3D('',#52829,#43288,#43289);
#36081=AXIS2_PLACEMENT_3D('',#52830,#43290,#43291);
#36082=AXIS2_PLACEMENT_3D('',#52831,#43292,#43293);
#36083=AXIS2_PLACEMENT_3D('',#52832,#43294,#43295);
#36084=AXIS2_PLACEMENT_3D('',#52833,#43296,#43297);
#36085=AXIS2_PLACEMENT_3D('',#52834,#43298,#43299);
#36086=AXIS2_PLACEMENT_3D('',#52835,#43300,#43301);
#36087=AXIS2_PLACEMENT_3D('',#52836,#43302,#43303);
#36088=AXIS2_PLACEMENT_3D('',#52837,#43304,#43305);
#36089=AXIS2_PLACEMENT_3D('',#52838,#43306,#43307);
#36090=AXIS2_PLACEMENT_3D('',#52839,#43308,#43309);
#36091=AXIS2_PLACEMENT_3D('',#52840,#43310,#43311);
#36092=AXIS2_PLACEMENT_3D('',#52841,#43312,#43313);
#36093=AXIS2_PLACEMENT_3D('',#52842,#43314,#43315);
#36094=AXIS2_PLACEMENT_3D('',#52843,#43316,#43317);
#36095=AXIS2_PLACEMENT_3D('',#52844,#43318,#43319);
#36096=AXIS2_PLACEMENT_3D('',#52845,#43320,#43321);
#36097=AXIS2_PLACEMENT_3D('',#52846,#43322,#43323);
#36098=AXIS2_PLACEMENT_3D('',#52847,#43324,#43325);
#36099=AXIS2_PLACEMENT_3D('',#52848,#43326,#43327);
#36100=AXIS2_PLACEMENT_3D('',#52849,#43328,#43329);
#36101=AXIS2_PLACEMENT_3D('',#52850,#43330,#43331);
#36102=AXIS2_PLACEMENT_3D('',#52851,#43332,#43333);
#36103=AXIS2_PLACEMENT_3D('',#52852,#43334,#43335);
#36104=AXIS2_PLACEMENT_3D('',#52853,#43336,#43337);
#36105=AXIS2_PLACEMENT_3D('',#52854,#43338,#43339);
#36106=AXIS2_PLACEMENT_3D('',#52855,#43340,#43341);
#36107=AXIS2_PLACEMENT_3D('',#52856,#43342,#43343);
#36108=AXIS2_PLACEMENT_3D('',#52857,#43344,#43345);
#36109=AXIS2_PLACEMENT_3D('',#52858,#43346,#43347);
#36110=AXIS2_PLACEMENT_3D('',#52859,#43348,#43349);
#36111=AXIS2_PLACEMENT_3D('',#52860,#43350,#43351);
#36112=AXIS2_PLACEMENT_3D('',#52861,#43352,#43353);
#36113=AXIS2_PLACEMENT_3D('',#52862,#43354,#43355);
#36114=AXIS2_PLACEMENT_3D('',#52863,#43356,#43357);
#36115=AXIS2_PLACEMENT_3D('',#52864,#43358,#43359);
#36116=AXIS2_PLACEMENT_3D('',#52865,#43360,#43361);
#36117=AXIS2_PLACEMENT_3D('',#52866,#43362,#43363);
#36118=AXIS2_PLACEMENT_3D('',#52867,#43364,#43365);
#36119=AXIS2_PLACEMENT_3D('',#52868,#43366,#43367);
#36120=AXIS2_PLACEMENT_3D('',#52869,#43368,#43369);
#36121=AXIS2_PLACEMENT_3D('',#52870,#43370,#43371);
#36122=AXIS2_PLACEMENT_3D('',#52871,#43372,#43373);
#36123=AXIS2_PLACEMENT_3D('',#52874,#43375,#43376);
#36124=AXIS2_PLACEMENT_3D('',#52875,#43377,#43378);
#36125=AXIS2_PLACEMENT_3D('',#52878,#43380,#43381);
#36126=AXIS2_PLACEMENT_3D('',#52879,#43382,#43383);
#36127=AXIS2_PLACEMENT_3D('',#52882,#43385,#43386);
#36128=AXIS2_PLACEMENT_3D('',#52883,#43387,#43388);
#36129=AXIS2_PLACEMENT_3D('',#52886,#43390,#43391);
#36130=AXIS2_PLACEMENT_3D('',#52887,#43392,#43393);
#36131=AXIS2_PLACEMENT_3D('',#52890,#43395,#43396);
#36132=AXIS2_PLACEMENT_3D('',#52891,#43397,#43398);
#36133=AXIS2_PLACEMENT_3D('',#52893,#43399,#43400);
#36134=AXIS2_PLACEMENT_3D('',#52896,#43402,#43403);
#36135=AXIS2_PLACEMENT_3D('',#52897,#43404,#43405);
#36136=AXIS2_PLACEMENT_3D('',#52900,#43407,#43408);
#36137=AXIS2_PLACEMENT_3D('',#52901,#43409,#43410);
#36138=AXIS2_PLACEMENT_3D('',#52904,#43412,#43413);
#36139=AXIS2_PLACEMENT_3D('',#52905,#43414,#43415);
#36140=AXIS2_PLACEMENT_3D('',#52908,#43417,#43418);
#36141=AXIS2_PLACEMENT_3D('',#52909,#43419,#43420);
#36142=AXIS2_PLACEMENT_3D('',#52912,#43422,#43423);
#36143=AXIS2_PLACEMENT_3D('',#52913,#43424,#43425);
#36144=AXIS2_PLACEMENT_3D('',#52914,#43426,#43427);
#36145=AXIS2_PLACEMENT_3D('',#52915,#43428,#43429);
#36146=AXIS2_PLACEMENT_3D('',#52916,#43430,#43431);
#36147=AXIS2_PLACEMENT_3D('',#52919,#43433,#43434);
#36148=AXIS2_PLACEMENT_3D('',#52920,#43435,#43436);
#36149=AXIS2_PLACEMENT_3D('',#52921,#43437,#43438);
#36150=AXIS2_PLACEMENT_3D('',#52924,#43440,#43441);
#36151=AXIS2_PLACEMENT_3D('',#52925,#43442,#43443);
#36152=AXIS2_PLACEMENT_3D('',#52926,#43444,#43445);
#36153=AXIS2_PLACEMENT_3D('',#52929,#43447,#43448);
#36154=AXIS2_PLACEMENT_3D('',#52930,#43449,#43450);
#36155=AXIS2_PLACEMENT_3D('',#52932,#43451,#43452);
#36156=AXIS2_PLACEMENT_3D('',#52933,#43453,#43454);
#36157=AXIS2_PLACEMENT_3D('',#52936,#43456,#43457);
#36158=AXIS2_PLACEMENT_3D('',#52937,#43458,#43459);
#36159=AXIS2_PLACEMENT_3D('',#52939,#43461,#43462);
#36160=AXIS2_PLACEMENT_3D('',#52941,#43463,#43464);
#36161=AXIS2_PLACEMENT_3D('',#52943,#43466,#43467);
#36162=AXIS2_PLACEMENT_3D('',#52945,#43468,#43469);
#36163=AXIS2_PLACEMENT_3D('',#52946,#43470,#43471);
#36164=AXIS2_PLACEMENT_3D('',#52949,#43473,#43474);
#36165=AXIS2_PLACEMENT_3D('',#52950,#43475,#43476);
#36166=AXIS2_PLACEMENT_3D('',#52952,#43478,#43479);
#36167=AXIS2_PLACEMENT_3D('',#52953,#43480,#43481);
#36168=AXIS2_PLACEMENT_3D('',#53007,#43483,#43484);
#36169=AXIS2_PLACEMENT_3D('',#53044,#43486,#43487);
#36170=AXIS2_PLACEMENT_3D('',#53082,#43489,#43490);
#36171=AXIS2_PLACEMENT_3D('',#53120,#43492,#43493);
#36172=AXIS2_PLACEMENT_3D('',#53157,#43495,#43496);
#36173=AXIS2_PLACEMENT_3D('',#53194,#43498,#43499);
#36174=AXIS2_PLACEMENT_3D('',#53215,#43501,#43502);
#36175=AXIS2_PLACEMENT_3D('',#53228,#43503,#43504);
#36176=AXIS2_PLACEMENT_3D('',#53266,#43506,#43507);
#36177=AXIS2_PLACEMENT_3D('',#53303,#43509,#43510);
#36178=AXIS2_PLACEMENT_3D('',#53305,#43511,#43512);
#36179=AXIS2_PLACEMENT_3D('',#53308,#43514,#43515);
#36180=AXIS2_PLACEMENT_3D('',#53309,#43516,#43517);
#36181=AXIS2_PLACEMENT_3D('',#53312,#43519,#43520);
#36182=AXIS2_PLACEMENT_3D('',#53314,#43521,#43522);
#36183=AXIS2_PLACEMENT_3D('',#53315,#43523,#43524);
#36184=AXIS2_PLACEMENT_3D('',#53324,#43529,#43530);
#36185=AXIS2_PLACEMENT_3D('',#53330,#43534,#43535);
#36186=AXIS2_PLACEMENT_3D('',#53343,#43542,#43543);
#36187=AXIS2_PLACEMENT_3D('',#53349,#43547,#43548);
#36188=AXIS2_PLACEMENT_3D('',#53355,#43552,#43553);
#36189=AXIS2_PLACEMENT_3D('',#53363,#43558,#43559);
#36190=AXIS2_PLACEMENT_3D('',#53370,#43563,#43564);
#36191=AXIS2_PLACEMENT_3D('',#53375,#43568,#43569);
#36192=AXIS2_PLACEMENT_3D('',#53380,#43573,#43574);
#36193=AXIS2_PLACEMENT_3D('',#53387,#43578,#43579);
#36194=AXIS2_PLACEMENT_3D('',#53395,#43584,#43585);
#36195=AXIS2_PLACEMENT_3D('',#53398,#43588,#43589);
#36196=AXIS2_PLACEMENT_3D('',#53405,#43593,#43594);
#36197=AXIS2_PLACEMENT_3D('',#53413,#43599,#43600);
#36198=AXIS2_PLACEMENT_3D('',#53416,#43603,#43604);
#36199=AXIS2_PLACEMENT_3D('',#53423,#43608,#43609);
#36200=AXIS2_PLACEMENT_3D('',#53431,#43614,#43615);
#36201=AXIS2_PLACEMENT_3D('',#53434,#43618,#43619);
#36202=AXIS2_PLACEMENT_3D('',#53441,#43623,#43624);
#36203=AXIS2_PLACEMENT_3D('',#53449,#43629,#43630);
#36204=AXIS2_PLACEMENT_3D('',#53452,#43633,#43634);
#36205=AXIS2_PLACEMENT_3D('',#53459,#43638,#43639);
#36206=AXIS2_PLACEMENT_3D('',#53467,#43644,#43645);
#36207=AXIS2_PLACEMENT_3D('',#53470,#43648,#43649);
#36208=AXIS2_PLACEMENT_3D('',#53478,#43654,#43655);
#36209=AXIS2_PLACEMENT_3D('',#53485,#43660,#43661);
#36210=AXIS2_PLACEMENT_3D('',#53487,#43663,#43664);
#36211=AXIS2_PLACEMENT_3D('',#53491,#43667,#43668);
#36212=AXIS2_PLACEMENT_3D('',#53493,#43670,#43671);
#36213=AXIS2_PLACEMENT_3D('',#53497,#43674,#43675);
#36214=AXIS2_PLACEMENT_3D('',#53499,#43677,#43678);
#36215=AXIS2_PLACEMENT_3D('',#53503,#43681,#43682);
#36216=AXIS2_PLACEMENT_3D('',#53508,#43686,#43687);
#36217=AXIS2_PLACEMENT_3D('',#53510,#43689,#43690);
#36218=AXIS2_PLACEMENT_3D('',#53513,#43693,#43694);
#36219=AXIS2_PLACEMENT_3D('',#53515,#43695,#43696);
#36220=AXIS2_PLACEMENT_3D('',#53518,#43698,#43699);
#36221=AXIS2_PLACEMENT_3D('',#53519,#43700,#43701);
#36222=AXIS2_PLACEMENT_3D('',#53522,#43703,#43704);
#36223=AXIS2_PLACEMENT_3D('',#53524,#43705,#43706);
#36224=AXIS2_PLACEMENT_3D('',#53526,#43707,#43708);
#36225=AXIS2_PLACEMENT_3D('',#53528,#43709,#43710);
#36226=AXIS2_PLACEMENT_3D('',#53529,#43711,#43712);
#36227=AXIS2_PLACEMENT_3D('',#53531,#43713,#43714);
#36228=AXIS2_PLACEMENT_3D('',#53533,#43716,#43717);
#36229=AXIS2_PLACEMENT_3D('',#53536,#43719,#43720);
#36230=AXIS2_PLACEMENT_3D('',#53537,#43721,#43722);
#36231=AXIS2_PLACEMENT_3D('',#53539,#43723,#43724);
#36232=AXIS2_PLACEMENT_3D('',#53541,#43726,#43727);
#36233=AXIS2_PLACEMENT_3D('',#53544,#43729,#43730);
#36234=AXIS2_PLACEMENT_3D('',#53545,#43731,#43732);
#36235=AXIS2_PLACEMENT_3D('',#53547,#43733,#43734);
#36236=AXIS2_PLACEMENT_3D('',#53549,#43736,#43737);
#36237=AXIS2_PLACEMENT_3D('',#53552,#43739,#43740);
#36238=AXIS2_PLACEMENT_3D('',#53553,#43741,#43742);
#36239=AXIS2_PLACEMENT_3D('',#53555,#43743,#43744);
#36240=AXIS2_PLACEMENT_3D('',#53557,#43746,#43747);
#36241=AXIS2_PLACEMENT_3D('',#53559,#43748,#43749);
#36242=AXIS2_PLACEMENT_3D('',#53561,#43751,#43752);
#36243=AXIS2_PLACEMENT_3D('',#53564,#43754,#43755);
#36244=AXIS2_PLACEMENT_3D('',#53566,#43756,#43757);
#36245=AXIS2_PLACEMENT_3D('',#53568,#43758,#43759);
#36246=AXIS2_PLACEMENT_3D('',#53570,#43760,#43761);
#36247=AXIS2_PLACEMENT_3D('',#53571,#43762,#43763);
#36248=AXIS2_PLACEMENT_3D('',#53573,#43765,#43766);
#36249=AXIS2_PLACEMENT_3D('',#53575,#43768,#43769);
#36250=AXIS2_PLACEMENT_3D('',#53577,#43771,#43772);
#36251=AXIS2_PLACEMENT_3D('',#53579,#43774,#43775);
#36252=AXIS2_PLACEMENT_3D('',#53580,#43776,#43777);
#36253=AXIS2_PLACEMENT_3D('',#53581,#43778,#43779);
#36254=AXIS2_PLACEMENT_3D('',#53582,#43780,#43781);
#36255=AXIS2_PLACEMENT_3D('',#53583,#43782,#43783);
#36256=AXIS2_PLACEMENT_3D('',#53584,#43784,#43785);
#36257=AXIS2_PLACEMENT_3D('',#53587,#43786,#43787);
#36258=AXIS2_PLACEMENT_3D('',#53588,#43788,#43789);
#36259=AXIS2_PLACEMENT_3D('',#53592,#43791,#43792);
#36260=AXIS2_PLACEMENT_3D('',#53593,#43793,#43794);
#36261=AXIS2_PLACEMENT_3D('',#53594,#43795,#43796);
#36262=AXIS2_PLACEMENT_3D('',#53598,#43798,#43799);
#36263=AXIS2_PLACEMENT_3D('',#53599,#43800,#43801);
#36264=AXIS2_PLACEMENT_3D('',#53600,#43802,#43803);
#36265=AXIS2_PLACEMENT_3D('',#53602,#43805,#43806);
#36266=AXIS2_PLACEMENT_3D('',#53605,#43808,#43809);
#36267=AXIS2_PLACEMENT_3D('',#53606,#43810,#43811);
#36268=AXIS2_PLACEMENT_3D('',#57631,#43812,#43813);
#36269=AXIS2_PLACEMENT_3D('',#57644,#43814,#43815);
#36270=AXIS2_PLACEMENT_3D('',#57645,#43816,#43817);
#36271=AXIS2_PLACEMENT_3D('',#57646,#43818,#43819);
#36272=AXIS2_PLACEMENT_3D('',#57657,#43820,#43821);
#36273=AXIS2_PLACEMENT_3D('',#57666,#43822,#43823);
#36274=AXIS2_PLACEMENT_3D('',#57686,#43824,#43825);
#36275=AXIS2_PLACEMENT_3D('',#57688,#43826,#43827);
#36276=AXIS2_PLACEMENT_3D('',#57689,#43828,#43829);
#36277=AXIS2_PLACEMENT_3D('',#57690,#43830,#43831);
#36278=AXIS2_PLACEMENT_3D('',#57694,#43833,#43834);
#36279=AXIS2_PLACEMENT_3D('',#57696,#43835,#43836);
#36280=AXIS2_PLACEMENT_3D('',#57697,#43837,#43838);
#36281=AXIS2_PLACEMENT_3D('',#57784,#43839,#43840);
#36282=AXIS2_PLACEMENT_3D('',#57786,#43841,#43842);
#36283=AXIS2_PLACEMENT_3D('',#57788,#43844,#43845);
#36284=AXIS2_PLACEMENT_3D('',#57791,#43848,#43849);
#36285=AXIS2_PLACEMENT_3D('',#57794,#43852,#43853);
#36286=AXIS2_PLACEMENT_3D('',#57797,#43856,#43857);
#36287=AXIS2_PLACEMENT_3D('',#57800,#43860,#43861);
#36288=AXIS2_PLACEMENT_3D('',#57803,#43864,#43865);
#36289=AXIS2_PLACEMENT_3D('',#57806,#43868,#43869);
#36290=AXIS2_PLACEMENT_3D('',#57809,#43872,#43873);
#36291=AXIS2_PLACEMENT_3D('',#57812,#43876,#43877);
#36292=AXIS2_PLACEMENT_3D('',#57820,#43880,#43881);
#36293=AXIS2_PLACEMENT_3D('',#57821,#43882,#43883);
#36294=AXIS2_PLACEMENT_3D('',#57824,#43886,#43887);
#36295=AXIS2_PLACEMENT_3D('',#57825,#43888,#43889);
#36296=AXIS2_PLACEMENT_3D('',#57832,#43890,#43891);
#36297=AXIS2_PLACEMENT_3D('',#57833,#43892,#43893);
#36298=AXIS2_PLACEMENT_3D('',#57834,#43894,#43895);
#36299=AXIS2_PLACEMENT_3D('',#57835,#43896,#43897);
#36300=AXIS2_PLACEMENT_3D('',#57836,#43898,#43899);
#36301=AXIS2_PLACEMENT_3D('',#57837,#43900,#43901);
#36302=AXIS2_PLACEMENT_3D('',#57846,#43902,#43903);
#36303=AXIS2_PLACEMENT_3D('',#57847,#43904,#43905);
#36304=AXIS2_PLACEMENT_3D('',#57848,#43906,#43907);
#36305=AXIS2_PLACEMENT_3D('',#57849,#43908,#43909);
#36306=AXIS2_PLACEMENT_3D('',#57850,#43910,#43911);
#36307=AXIS2_PLACEMENT_3D('',#57851,#43912,#43913);
#36308=AXIS2_PLACEMENT_3D('',#57852,#43914,#43915);
#36309=AXIS2_PLACEMENT_3D('',#57853,#43916,#43917);
#36310=AXIS2_PLACEMENT_3D('',#57869,#43918,#43919);
#36311=AXIS2_PLACEMENT_3D('',#57878,#43920,#43921);
#36312=AXIS2_PLACEMENT_3D('',#57888,#43923,#43924);
#36313=AXIS2_PLACEMENT_3D('',#57890,#43925,#43926);
#36314=AXIS2_PLACEMENT_3D('',#57892,#43928,#43929);
#36315=AXIS2_PLACEMENT_3D('',#57894,#43930,#43931);
#36316=AXIS2_PLACEMENT_3D('',#57896,#43933,#43934);
#36317=AXIS2_PLACEMENT_3D('',#57898,#43935,#43936);
#36318=AXIS2_PLACEMENT_3D('',#57899,#43937,#43938);
#36319=AXIS2_PLACEMENT_3D('',#57901,#43939,#43940);
#36320=AXIS2_PLACEMENT_3D('',#57903,#43942,#43943);
#36321=AXIS2_PLACEMENT_3D('',#57905,#43944,#43945);
#36322=AXIS2_PLACEMENT_3D('',#57907,#43947,#43948);
#36323=AXIS2_PLACEMENT_3D('',#57909,#43949,#43950);
#36324=AXIS2_PLACEMENT_3D('',#57911,#43952,#43953);
#36325=AXIS2_PLACEMENT_3D('',#57913,#43954,#43955);
#36326=AXIS2_PLACEMENT_3D('',#57915,#43957,#43958);
#36327=AXIS2_PLACEMENT_3D('',#57918,#43959,#43960);
#36328=AXIS2_PLACEMENT_3D('',#57921,#43963,#43964);
#36329=AXIS2_PLACEMENT_3D('',#57925,#43967,#43968);
#36330=AXIS2_PLACEMENT_3D('',#57929,#43970,#43971);
#36331=AXIS2_PLACEMENT_3D('',#57931,#43973,#43974);
#36332=AXIS2_PLACEMENT_3D('',#57932,#43975,#43976);
#36333=AXIS2_PLACEMENT_3D('',#57934,#43978,#43979);
#36334=AXIS2_PLACEMENT_3D('',#57936,#43980,#43981);
#36335=AXIS2_PLACEMENT_3D('',#57937,#43982,#43983);
#36336=AXIS2_PLACEMENT_3D('',#57939,#43984,#43985);
#36337=AXIS2_PLACEMENT_3D('',#57941,#43987,#43988);
#36338=AXIS2_PLACEMENT_3D('',#57946,#43990,#43991);
#36339=AXIS2_PLACEMENT_3D('',#57948,#43993,#43994);
#36340=AXIS2_PLACEMENT_3D('',#57949,#43995,#43996);
#36341=AXIS2_PLACEMENT_3D('',#57950,#43997,#43998);
#36342=AXIS2_PLACEMENT_3D('',#57951,#43999,#44000);
#36343=AXIS2_PLACEMENT_3D('',#57954,#44001,#44002);
#36344=AXIS2_PLACEMENT_3D('',#57955,#44003,#44004);
#36345=AXIS2_PLACEMENT_3D('',#57958,#44006,#44007);
#36346=AXIS2_PLACEMENT_3D('',#57959,#44008,#44009);
#36347=AXIS2_PLACEMENT_3D('',#57961,#44010,#44011);
#36348=AXIS2_PLACEMENT_3D('',#57962,#44012,#44013);
#36349=AXIS2_PLACEMENT_3D('',#57965,#44015,#44016);
#36350=AXIS2_PLACEMENT_3D('',#57966,#44017,#44018);
#36351=AXIS2_PLACEMENT_3D('',#57968,#44019,#44020);
#36352=AXIS2_PLACEMENT_3D('',#57972,#44022,#44023);
#36353=AXIS2_PLACEMENT_3D('',#57973,#44024,#44025);
#36354=AXIS2_PLACEMENT_3D('',#57974,#44026,#44027);
#36355=AXIS2_PLACEMENT_3D('',#57976,#44028,#44029);
#36356=AXIS2_PLACEMENT_3D('',#57977,#44030,#44031);
#36357=AXIS2_PLACEMENT_3D('',#57979,#44032,#44033);
#36358=AXIS2_PLACEMENT_3D('',#57981,#44035,#44036);
#36359=AXIS2_PLACEMENT_3D('',#57983,#44037,#44038);
#36360=AXIS2_PLACEMENT_3D('',#57985,#44039,#44040);
#36361=AXIS2_PLACEMENT_3D('',#57986,#44041,#44042);
#36362=AXIS2_PLACEMENT_3D('',#57987,#44043,#44044);
#36363=AXIS2_PLACEMENT_3D('',#57989,#44045,#44046);
#36364=AXIS2_PLACEMENT_3D('',#57990,#44047,#44048);
#36365=AXIS2_PLACEMENT_3D('',#57992,#44049,#44050);
#36366=AXIS2_PLACEMENT_3D('',#57994,#44052,#44053);
#36367=AXIS2_PLACEMENT_3D('',#57996,#44054,#44055);
#36368=AXIS2_PLACEMENT_3D('',#57998,#44057,#44058);
#36369=AXIS2_PLACEMENT_3D('',#58000,#44060,#44061);
#36370=AXIS2_PLACEMENT_3D('',#58003,#44063,#44064);
#36371=AXIS2_PLACEMENT_3D('',#58004,#44065,#44066);
#36372=AXIS2_PLACEMENT_3D('',#58007,#44068,#44069);
#36373=AXIS2_PLACEMENT_3D('',#58008,#44070,#44071);
#36374=AXIS2_PLACEMENT_3D('',#58011,#44073,#44074);
#36375=AXIS2_PLACEMENT_3D('',#58012,#44075,#44076);
#36376=AXIS2_PLACEMENT_3D('',#58014,#44078,#44079);
#36377=AXIS2_PLACEMENT_3D('',#58015,#44080,#44081);
#36378=AXIS2_PLACEMENT_3D('',#58016,#44082,#44083);
#36379=AXIS2_PLACEMENT_3D('',#58018,#44084,#44085);
#36380=AXIS2_PLACEMENT_3D('',#58021,#44087,#44088);
#36381=AXIS2_PLACEMENT_3D('',#58022,#44089,#44090);
#36382=AXIS2_PLACEMENT_3D('',#58024,#44091,#44092);
#36383=AXIS2_PLACEMENT_3D('',#58026,#44094,#44095);
#36384=AXIS2_PLACEMENT_3D('',#58028,#44096,#44097);
#36385=AXIS2_PLACEMENT_3D('',#58030,#44099,#44100);
#36386=AXIS2_PLACEMENT_3D('',#58032,#44101,#44102);
#36387=AXIS2_PLACEMENT_3D('',#58033,#44103,#44104);
#36388=AXIS2_PLACEMENT_3D('',#58036,#44106,#44107);
#36389=AXIS2_PLACEMENT_3D('',#58037,#44108,#44109);
#36390=AXIS2_PLACEMENT_3D('',#58040,#44111,#44112);
#36391=AXIS2_PLACEMENT_3D('',#58041,#44113,#44114);
#36392=AXIS2_PLACEMENT_3D('',#58044,#44116,#44117);
#36393=AXIS2_PLACEMENT_3D('',#58045,#44118,#44119);
#36394=AXIS2_PLACEMENT_3D('',#58046,#44120,#44121);
#36395=AXIS2_PLACEMENT_3D('',#58047,#44122,#44123);
#36396=AXIS2_PLACEMENT_3D('',#58050,#44124,#44125);
#36397=AXIS2_PLACEMENT_3D('',#58051,#44126,#44127);
#36398=AXIS2_PLACEMENT_3D('',#58054,#44129,#44130);
#36399=AXIS2_PLACEMENT_3D('',#58055,#44131,#44132);
#36400=AXIS2_PLACEMENT_3D('',#58057,#44133,#44134);
#36401=AXIS2_PLACEMENT_3D('',#58058,#44135,#44136);
#36402=AXIS2_PLACEMENT_3D('',#58060,#44137,#44138);
#36403=AXIS2_PLACEMENT_3D('',#58062,#44140,#44141);
#36404=AXIS2_PLACEMENT_3D('',#58064,#44142,#44143);
#36405=AXIS2_PLACEMENT_3D('',#58068,#44145,#44146);
#36406=AXIS2_PLACEMENT_3D('',#58069,#44147,#44148);
#36407=AXIS2_PLACEMENT_3D('',#58070,#44149,#44150);
#36408=AXIS2_PLACEMENT_3D('',#58073,#44152,#44153);
#36409=AXIS2_PLACEMENT_3D('',#58074,#44154,#44155);
#36410=AXIS2_PLACEMENT_3D('',#58076,#44156,#44157);
#36411=AXIS2_PLACEMENT_3D('',#58077,#44158,#44159);
#36412=AXIS2_PLACEMENT_3D('',#58109,#44160,#44161);
#36413=AXIS2_PLACEMENT_3D('',#58111,#44162,#44163);
#36414=AXIS2_PLACEMENT_3D('',#58112,#44164,#44165);
#36415=AXIS2_PLACEMENT_3D('',#58113,#44166,#44167);
#36416=AXIS2_PLACEMENT_3D('',#58114,#44168,#44169);
#36417=AXIS2_PLACEMENT_3D('',#58121,#44170,#44171);
#36418=AXIS2_PLACEMENT_3D('',#58123,#44172,#44173);
#36419=AXIS2_PLACEMENT_3D('',#58128,#44174,#44175);
#36420=AXIS2_PLACEMENT_3D('',#58130,#44176,#44177);
#36421=AXIS2_PLACEMENT_3D('',#58131,#44178,#44179);
#36422=AXIS2_PLACEMENT_3D('',#58161,#44180,#44181);
#36423=AXIS2_PLACEMENT_3D('',#58162,#44182,#44183);
#36424=AXIS2_PLACEMENT_3D('',#58163,#44184,#44185);
#36425=AXIS2_PLACEMENT_3D('',#58199,#44186,#44187);
#36426=AXIS2_PLACEMENT_3D('',#58201,#44188,#44189);
#36427=AXIS2_PLACEMENT_3D('',#58202,#44190,#44191);
#36428=AXIS2_PLACEMENT_3D('',#58203,#44192,#44193);
#36429=AXIS2_PLACEMENT_3D('',#58204,#44194,#44195);
#36430=AXIS2_PLACEMENT_3D('',#58211,#44196,#44197);
#36431=AXIS2_PLACEMENT_3D('',#58213,#44198,#44199);
#36432=AXIS2_PLACEMENT_3D('',#58218,#44200,#44201);
#36433=AXIS2_PLACEMENT_3D('',#58220,#44202,#44203);
#36434=AXIS2_PLACEMENT_3D('',#58221,#44204,#44205);
#36435=AXIS2_PLACEMENT_3D('',#58255,#44206,#44207);
#36436=AXIS2_PLACEMENT_3D('',#58256,#44208,#44209);
#36437=AXIS2_PLACEMENT_3D('',#58257,#44210,#44211);
#36438=AXIS2_PLACEMENT_3D('',#58293,#44212,#44213);
#36439=AXIS2_PLACEMENT_3D('',#58295,#44214,#44215);
#36440=AXIS2_PLACEMENT_3D('',#58296,#44216,#44217);
#36441=AXIS2_PLACEMENT_3D('',#58297,#44218,#44219);
#36442=AXIS2_PLACEMENT_3D('',#58298,#44220,#44221);
#36443=AXIS2_PLACEMENT_3D('',#58305,#44222,#44223);
#36444=AXIS2_PLACEMENT_3D('',#58307,#44224,#44225);
#36445=AXIS2_PLACEMENT_3D('',#58312,#44226,#44227);
#36446=AXIS2_PLACEMENT_3D('',#58314,#44228,#44229);
#36447=AXIS2_PLACEMENT_3D('',#58315,#44230,#44231);
#36448=AXIS2_PLACEMENT_3D('',#58349,#44232,#44233);
#36449=AXIS2_PLACEMENT_3D('',#58350,#44234,#44235);
#36450=AXIS2_PLACEMENT_3D('',#58351,#44236,#44237);
#36451=AXIS2_PLACEMENT_3D('',#58387,#44238,#44239);
#36452=AXIS2_PLACEMENT_3D('',#58389,#44240,#44241);
#36453=AXIS2_PLACEMENT_3D('',#58390,#44242,#44243);
#36454=AXIS2_PLACEMENT_3D('',#58391,#44244,#44245);
#36455=AXIS2_PLACEMENT_3D('',#58392,#44246,#44247);
#36456=AXIS2_PLACEMENT_3D('',#58399,#44248,#44249);
#36457=AXIS2_PLACEMENT_3D('',#58401,#44250,#44251);
#36458=AXIS2_PLACEMENT_3D('',#58406,#44252,#44253);
#36459=AXIS2_PLACEMENT_3D('',#58408,#44254,#44255);
#36460=AXIS2_PLACEMENT_3D('',#58409,#44256,#44257);
#36461=AXIS2_PLACEMENT_3D('',#58439,#44258,#44259);
#36462=AXIS2_PLACEMENT_3D('',#58440,#44260,#44261);
#36463=AXIS2_PLACEMENT_3D('',#58441,#44262,#44263);
#36464=AXIS2_PLACEMENT_3D('',#58473,#44264,#44265);
#36465=AXIS2_PLACEMENT_3D('',#58475,#44266,#44267);
#36466=AXIS2_PLACEMENT_3D('',#58476,#44268,#44269);
#36467=AXIS2_PLACEMENT_3D('',#58477,#44270,#44271);
#36468=AXIS2_PLACEMENT_3D('',#58478,#44272,#44273);
#36469=AXIS2_PLACEMENT_3D('',#58485,#44274,#44275);
#36470=AXIS2_PLACEMENT_3D('',#58487,#44276,#44277);
#36471=AXIS2_PLACEMENT_3D('',#58492,#44278,#44279);
#36472=AXIS2_PLACEMENT_3D('',#58494,#44280,#44281);
#36473=AXIS2_PLACEMENT_3D('',#58495,#44282,#44283);
#36474=AXIS2_PLACEMENT_3D('',#58523,#44284,#44285);
#36475=AXIS2_PLACEMENT_3D('',#58524,#44286,#44287);
#36476=AXIS2_PLACEMENT_3D('',#58525,#44288,#44289);
#36477=AXIS2_PLACEMENT_3D('',#58557,#44290,#44291);
#36478=AXIS2_PLACEMENT_3D('',#58559,#44292,#44293);
#36479=AXIS2_PLACEMENT_3D('',#58560,#44294,#44295);
#36480=AXIS2_PLACEMENT_3D('',#58561,#44296,#44297);
#36481=AXIS2_PLACEMENT_3D('',#58562,#44298,#44299);
#36482=AXIS2_PLACEMENT_3D('',#58569,#44300,#44301);
#36483=AXIS2_PLACEMENT_3D('',#58571,#44302,#44303);
#36484=AXIS2_PLACEMENT_3D('',#58576,#44304,#44305);
#36485=AXIS2_PLACEMENT_3D('',#58578,#44306,#44307);
#36486=AXIS2_PLACEMENT_3D('',#58579,#44308,#44309);
#36487=AXIS2_PLACEMENT_3D('',#58607,#44310,#44311);
#36488=AXIS2_PLACEMENT_3D('',#58608,#44312,#44313);
#36489=AXIS2_PLACEMENT_3D('',#58609,#44314,#44315);
#36490=AXIS2_PLACEMENT_3D('',#58645,#44316,#44317);
#36491=AXIS2_PLACEMENT_3D('',#58647,#44318,#44319);
#36492=AXIS2_PLACEMENT_3D('',#58648,#44320,#44321);
#36493=AXIS2_PLACEMENT_3D('',#58649,#44322,#44323);
#36494=AXIS2_PLACEMENT_3D('',#58650,#44324,#44325);
#36495=AXIS2_PLACEMENT_3D('',#58657,#44326,#44327);
#36496=AXIS2_PLACEMENT_3D('',#58659,#44328,#44329);
#36497=AXIS2_PLACEMENT_3D('',#58664,#44330,#44331);
#36498=AXIS2_PLACEMENT_3D('',#58666,#44332,#44333);
#36499=AXIS2_PLACEMENT_3D('',#58667,#44334,#44335);
#36500=AXIS2_PLACEMENT_3D('',#58697,#44336,#44337);
#36501=AXIS2_PLACEMENT_3D('',#58698,#44338,#44339);
#36502=AXIS2_PLACEMENT_3D('',#58699,#44340,#44341);
#36503=AXIS2_PLACEMENT_3D('',#58735,#44342,#44343);
#36504=AXIS2_PLACEMENT_3D('',#58737,#44344,#44345);
#36505=AXIS2_PLACEMENT_3D('',#58738,#44346,#44347);
#36506=AXIS2_PLACEMENT_3D('',#58739,#44348,#44349);
#36507=AXIS2_PLACEMENT_3D('',#58740,#44350,#44351);
#36508=AXIS2_PLACEMENT_3D('',#58747,#44352,#44353);
#36509=AXIS2_PLACEMENT_3D('',#58749,#44354,#44355);
#36510=AXIS2_PLACEMENT_3D('',#58754,#44356,#44357);
#36511=AXIS2_PLACEMENT_3D('',#58756,#44358,#44359);
#36512=AXIS2_PLACEMENT_3D('',#58757,#44360,#44361);
#36513=AXIS2_PLACEMENT_3D('',#58791,#44362,#44363);
#36514=AXIS2_PLACEMENT_3D('',#58792,#44364,#44365);
#36515=AXIS2_PLACEMENT_3D('',#58793,#44366,#44367);
#36516=AXIS2_PLACEMENT_3D('',#58829,#44368,#44369);
#36517=AXIS2_PLACEMENT_3D('',#58831,#44370,#44371);
#36518=AXIS2_PLACEMENT_3D('',#58832,#44372,#44373);
#36519=AXIS2_PLACEMENT_3D('',#58833,#44374,#44375);
#36520=AXIS2_PLACEMENT_3D('',#58834,#44376,#44377);
#36521=AXIS2_PLACEMENT_3D('',#58841,#44378,#44379);
#36522=AXIS2_PLACEMENT_3D('',#58843,#44380,#44381);
#36523=AXIS2_PLACEMENT_3D('',#58848,#44382,#44383);
#36524=AXIS2_PLACEMENT_3D('',#58850,#44384,#44385);
#36525=AXIS2_PLACEMENT_3D('',#58851,#44386,#44387);
#36526=AXIS2_PLACEMENT_3D('',#58885,#44388,#44389);
#36527=AXIS2_PLACEMENT_3D('',#58886,#44390,#44391);
#36528=AXIS2_PLACEMENT_3D('',#58887,#44392,#44393);
#36529=AXIS2_PLACEMENT_3D('',#58919,#44394,#44395);
#36530=AXIS2_PLACEMENT_3D('',#58921,#44396,#44397);
#36531=AXIS2_PLACEMENT_3D('',#58922,#44398,#44399);
#36532=AXIS2_PLACEMENT_3D('',#58923,#44400,#44401);
#36533=AXIS2_PLACEMENT_3D('',#58924,#44402,#44403);
#36534=AXIS2_PLACEMENT_3D('',#58931,#44404,#44405);
#36535=AXIS2_PLACEMENT_3D('',#58933,#44406,#44407);
#36536=AXIS2_PLACEMENT_3D('',#58938,#44408,#44409);
#36537=AXIS2_PLACEMENT_3D('',#58940,#44410,#44411);
#36538=AXIS2_PLACEMENT_3D('',#58941,#44412,#44413);
#36539=AXIS2_PLACEMENT_3D('',#58971,#44414,#44415);
#36540=AXIS2_PLACEMENT_3D('',#58972,#44416,#44417);
#36541=AXIS2_PLACEMENT_3D('',#58973,#44418,#44419);
#36542=AXIS2_PLACEMENT_3D('',#58993,#44420,#44421);
#36543=AXIS2_PLACEMENT_3D('',#58995,#44422,#44423);
#36544=AXIS2_PLACEMENT_3D('',#58996,#44424,#44425);
#36545=AXIS2_PLACEMENT_3D('',#58998,#44426,#44427);
#36546=AXIS2_PLACEMENT_3D('',#59015,#44428,#44429);
#36547=AXIS2_PLACEMENT_3D('',#59022,#44430,#44431);
#36548=AXIS2_PLACEMENT_3D('',#59024,#44432,#44433);
#36549=AXIS2_PLACEMENT_3D('',#59029,#44434,#44435);
#36550=AXIS2_PLACEMENT_3D('',#59031,#44436,#44437);
#36551=AXIS2_PLACEMENT_3D('',#59032,#44438,#44439);
#36552=AXIS2_PLACEMENT_3D('',#59069,#44440,#44441);
#36553=AXIS2_PLACEMENT_3D('',#59070,#44442,#44443);
#36554=AXIS2_PLACEMENT_3D('',#59071,#44444,#44445);
#36555=AXIS2_PLACEMENT_3D('',#59103,#44446,#44447);
#36556=AXIS2_PLACEMENT_3D('',#59105,#44448,#44449);
#36557=AXIS2_PLACEMENT_3D('',#59106,#44450,#44451);
#36558=AXIS2_PLACEMENT_3D('',#59107,#44452,#44453);
#36559=AXIS2_PLACEMENT_3D('',#59108,#44454,#44455);
#36560=AXIS2_PLACEMENT_3D('',#59115,#44456,#44457);
#36561=AXIS2_PLACEMENT_3D('',#59117,#44458,#44459);
#36562=AXIS2_PLACEMENT_3D('',#59122,#44460,#44461);
#36563=AXIS2_PLACEMENT_3D('',#59124,#44462,#44463);
#36564=AXIS2_PLACEMENT_3D('',#59125,#44464,#44465);
#36565=AXIS2_PLACEMENT_3D('',#59155,#44466,#44467);
#36566=AXIS2_PLACEMENT_3D('',#59156,#44468,#44469);
#36567=AXIS2_PLACEMENT_3D('',#59157,#44470,#44471);
#36568=AXIS2_PLACEMENT_3D('',#59193,#44472,#44473);
#36569=AXIS2_PLACEMENT_3D('',#59195,#44474,#44475);
#36570=AXIS2_PLACEMENT_3D('',#59196,#44476,#44477);
#36571=AXIS2_PLACEMENT_3D('',#59197,#44478,#44479);
#36572=AXIS2_PLACEMENT_3D('',#59198,#44480,#44481);
#36573=AXIS2_PLACEMENT_3D('',#59205,#44482,#44483);
#36574=AXIS2_PLACEMENT_3D('',#59207,#44484,#44485);
#36575=AXIS2_PLACEMENT_3D('',#59212,#44486,#44487);
#36576=AXIS2_PLACEMENT_3D('',#59214,#44488,#44489);
#36577=AXIS2_PLACEMENT_3D('',#59215,#44490,#44491);
#36578=AXIS2_PLACEMENT_3D('',#59249,#44492,#44493);
#36579=AXIS2_PLACEMENT_3D('',#59250,#44494,#44495);
#36580=AXIS2_PLACEMENT_3D('',#59251,#44496,#44497);
#36581=AXIS2_PLACEMENT_3D('',#59287,#44498,#44499);
#36582=AXIS2_PLACEMENT_3D('',#59289,#44500,#44501);
#36583=AXIS2_PLACEMENT_3D('',#59290,#44502,#44503);
#36584=AXIS2_PLACEMENT_3D('',#59291,#44504,#44505);
#36585=AXIS2_PLACEMENT_3D('',#59292,#44506,#44507);
#36586=AXIS2_PLACEMENT_3D('',#59299,#44508,#44509);
#36587=AXIS2_PLACEMENT_3D('',#59301,#44510,#44511);
#36588=AXIS2_PLACEMENT_3D('',#59306,#44512,#44513);
#36589=AXIS2_PLACEMENT_3D('',#59308,#44514,#44515);
#36590=AXIS2_PLACEMENT_3D('',#59309,#44516,#44517);
#36591=AXIS2_PLACEMENT_3D('',#59343,#44518,#44519);
#36592=AXIS2_PLACEMENT_3D('',#59344,#44520,#44521);
#36593=AXIS2_PLACEMENT_3D('',#59345,#44522,#44523);
#36594=AXIS2_PLACEMENT_3D('',#59381,#44524,#44525);
#36595=AXIS2_PLACEMENT_3D('',#59383,#44526,#44527);
#36596=AXIS2_PLACEMENT_3D('',#59384,#44528,#44529);
#36597=AXIS2_PLACEMENT_3D('',#59385,#44530,#44531);
#36598=AXIS2_PLACEMENT_3D('',#59386,#44532,#44533);
#36599=AXIS2_PLACEMENT_3D('',#59393,#44534,#44535);
#36600=AXIS2_PLACEMENT_3D('',#59395,#44536,#44537);
#36601=AXIS2_PLACEMENT_3D('',#59400,#44538,#44539);
#36602=AXIS2_PLACEMENT_3D('',#59402,#44540,#44541);
#36603=AXIS2_PLACEMENT_3D('',#59403,#44542,#44543);
#36604=AXIS2_PLACEMENT_3D('',#59433,#44544,#44545);
#36605=AXIS2_PLACEMENT_3D('',#59434,#44546,#44547);
#36606=AXIS2_PLACEMENT_3D('',#59435,#44548,#44549);
#36607=AXIS2_PLACEMENT_3D('',#59467,#44550,#44551);
#36608=AXIS2_PLACEMENT_3D('',#59469,#44552,#44553);
#36609=AXIS2_PLACEMENT_3D('',#59470,#44554,#44555);
#36610=AXIS2_PLACEMENT_3D('',#59471,#44556,#44557);
#36611=AXIS2_PLACEMENT_3D('',#59472,#44558,#44559);
#36612=AXIS2_PLACEMENT_3D('',#59479,#44560,#44561);
#36613=AXIS2_PLACEMENT_3D('',#59481,#44562,#44563);
#36614=AXIS2_PLACEMENT_3D('',#59486,#44564,#44565);
#36615=AXIS2_PLACEMENT_3D('',#59488,#44566,#44567);
#36616=AXIS2_PLACEMENT_3D('',#59489,#44568,#44569);
#36617=AXIS2_PLACEMENT_3D('',#59517,#44570,#44571);
#36618=AXIS2_PLACEMENT_3D('',#59518,#44572,#44573);
#36619=AXIS2_PLACEMENT_3D('',#59519,#44574,#44575);
#36620=AXIS2_PLACEMENT_3D('',#59551,#44576,#44577);
#36621=AXIS2_PLACEMENT_3D('',#59553,#44578,#44579);
#36622=AXIS2_PLACEMENT_3D('',#59554,#44580,#44581);
#36623=AXIS2_PLACEMENT_3D('',#59555,#44582,#44583);
#36624=AXIS2_PLACEMENT_3D('',#59556,#44584,#44585);
#36625=AXIS2_PLACEMENT_3D('',#59563,#44586,#44587);
#36626=AXIS2_PLACEMENT_3D('',#59565,#44588,#44589);
#36627=AXIS2_PLACEMENT_3D('',#59570,#44590,#44591);
#36628=AXIS2_PLACEMENT_3D('',#59572,#44592,#44593);
#36629=AXIS2_PLACEMENT_3D('',#59573,#44594,#44595);
#36630=AXIS2_PLACEMENT_3D('',#59601,#44596,#44597);
#36631=AXIS2_PLACEMENT_3D('',#59602,#44598,#44599);
#36632=AXIS2_PLACEMENT_3D('',#59603,#44600,#44601);
#36633=AXIS2_PLACEMENT_3D('',#59639,#44602,#44603);
#36634=AXIS2_PLACEMENT_3D('',#59641,#44604,#44605);
#36635=AXIS2_PLACEMENT_3D('',#59642,#44606,#44607);
#36636=AXIS2_PLACEMENT_3D('',#59643,#44608,#44609);
#36637=AXIS2_PLACEMENT_3D('',#59644,#44610,#44611);
#36638=AXIS2_PLACEMENT_3D('',#59651,#44612,#44613);
#36639=AXIS2_PLACEMENT_3D('',#59653,#44614,#44615);
#36640=AXIS2_PLACEMENT_3D('',#59658,#44616,#44617);
#36641=AXIS2_PLACEMENT_3D('',#59660,#44618,#44619);
#36642=AXIS2_PLACEMENT_3D('',#59661,#44620,#44621);
#36643=AXIS2_PLACEMENT_3D('',#59691,#44622,#44623);
#36644=AXIS2_PLACEMENT_3D('',#59692,#44624,#44625);
#36645=AXIS2_PLACEMENT_3D('',#59693,#44626,#44627);
#36646=AXIS2_PLACEMENT_3D('',#59729,#44628,#44629);
#36647=AXIS2_PLACEMENT_3D('',#59731,#44630,#44631);
#36648=AXIS2_PLACEMENT_3D('',#59732,#44632,#44633);
#36649=AXIS2_PLACEMENT_3D('',#59733,#44634,#44635);
#36650=AXIS2_PLACEMENT_3D('',#59734,#44636,#44637);
#36651=AXIS2_PLACEMENT_3D('',#59741,#44638,#44639);
#36652=AXIS2_PLACEMENT_3D('',#59743,#44640,#44641);
#36653=AXIS2_PLACEMENT_3D('',#59748,#44642,#44643);
#36654=AXIS2_PLACEMENT_3D('',#59750,#44644,#44645);
#36655=AXIS2_PLACEMENT_3D('',#59751,#44646,#44647);
#36656=AXIS2_PLACEMENT_3D('',#59785,#44648,#44649);
#36657=AXIS2_PLACEMENT_3D('',#59786,#44650,#44651);
#36658=AXIS2_PLACEMENT_3D('',#59787,#44652,#44653);
#36659=AXIS2_PLACEMENT_3D('',#59823,#44654,#44655);
#36660=AXIS2_PLACEMENT_3D('',#59825,#44656,#44657);
#36661=AXIS2_PLACEMENT_3D('',#59826,#44658,#44659);
#36662=AXIS2_PLACEMENT_3D('',#59827,#44660,#44661);
#36663=AXIS2_PLACEMENT_3D('',#59828,#44662,#44663);
#36664=AXIS2_PLACEMENT_3D('',#59835,#44664,#44665);
#36665=AXIS2_PLACEMENT_3D('',#59837,#44666,#44667);
#36666=AXIS2_PLACEMENT_3D('',#59842,#44668,#44669);
#36667=AXIS2_PLACEMENT_3D('',#59844,#44670,#44671);
#36668=AXIS2_PLACEMENT_3D('',#59845,#44672,#44673);
#36669=AXIS2_PLACEMENT_3D('',#59879,#44674,#44675);
#36670=AXIS2_PLACEMENT_3D('',#59880,#44676,#44677);
#36671=AXIS2_PLACEMENT_3D('',#59881,#44678,#44679);
#36672=AXIS2_PLACEMENT_3D('',#59913,#44680,#44681);
#36673=AXIS2_PLACEMENT_3D('',#59915,#44682,#44683);
#36674=AXIS2_PLACEMENT_3D('',#59916,#44684,#44685);
#36675=AXIS2_PLACEMENT_3D('',#59917,#44686,#44687);
#36676=AXIS2_PLACEMENT_3D('',#59918,#44688,#44689);
#36677=AXIS2_PLACEMENT_3D('',#59925,#44690,#44691);
#36678=AXIS2_PLACEMENT_3D('',#59927,#44692,#44693);
#36679=AXIS2_PLACEMENT_3D('',#59932,#44694,#44695);
#36680=AXIS2_PLACEMENT_3D('',#59934,#44696,#44697);
#36681=AXIS2_PLACEMENT_3D('',#59935,#44698,#44699);
#36682=AXIS2_PLACEMENT_3D('',#59965,#44700,#44701);
#36683=AXIS2_PLACEMENT_3D('',#59966,#44702,#44703);
#36684=AXIS2_PLACEMENT_3D('',#59967,#44704,#44705);
#36685=AXIS2_PLACEMENT_3D('',#59999,#44706,#44707);
#36686=AXIS2_PLACEMENT_3D('',#60001,#44708,#44709);
#36687=AXIS2_PLACEMENT_3D('',#60002,#44710,#44711);
#36688=AXIS2_PLACEMENT_3D('',#60003,#44712,#44713);
#36689=AXIS2_PLACEMENT_3D('',#60004,#44714,#44715);
#36690=AXIS2_PLACEMENT_3D('',#60011,#44716,#44717);
#36691=AXIS2_PLACEMENT_3D('',#60013,#44718,#44719);
#36692=AXIS2_PLACEMENT_3D('',#60018,#44720,#44721);
#36693=AXIS2_PLACEMENT_3D('',#60020,#44722,#44723);
#36694=AXIS2_PLACEMENT_3D('',#60021,#44724,#44725);
#36695=AXIS2_PLACEMENT_3D('',#60053,#44726,#44727);
#36696=AXIS2_PLACEMENT_3D('',#60054,#44728,#44729);
#36697=AXIS2_PLACEMENT_3D('',#60055,#44730,#44731);
#36698=AXIS2_PLACEMENT_3D('',#60058,#44733,#44734);
#36699=AXIS2_PLACEMENT_3D('',#60059,#44735,#44736);
#36700=AXIS2_PLACEMENT_3D('',#60062,#44739,#44740);
#36701=AXIS2_PLACEMENT_3D('',#60064,#44741,#44742);
#36702=AXIS2_PLACEMENT_3D('',#60066,#44744,#44745);
#36703=AXIS2_PLACEMENT_3D('',#60068,#44746,#44747);
#36704=AXIS2_PLACEMENT_3D('',#60069,#44748,#44749);
#36705=AXIS2_PLACEMENT_3D('',#60072,#44751,#44752);
#36706=AXIS2_PLACEMENT_3D('',#60073,#44753,#44754);
#36707=AXIS2_PLACEMENT_3D('',#60076,#44756,#44757);
#36708=AXIS2_PLACEMENT_3D('',#60077,#44758,#44759);
#36709=AXIS2_PLACEMENT_3D('',#60080,#44761,#44762);
#36710=AXIS2_PLACEMENT_3D('',#60081,#44763,#44764);
#36711=AXIS2_PLACEMENT_3D('',#60082,#44765,#44766);
#36712=AXIS2_PLACEMENT_3D('',#60083,#44767,#44768);
#36713=AXIS2_PLACEMENT_3D('',#60085,#44769,#44770);
#36714=AXIS2_PLACEMENT_3D('',#60088,#44772,#44773);
#36715=AXIS2_PLACEMENT_3D('',#60089,#44774,#44775);
#36716=AXIS2_PLACEMENT_3D('',#60091,#44776,#44777);
#36717=AXIS2_PLACEMENT_3D('',#60093,#44779,#44780);
#36718=AXIS2_PLACEMENT_3D('',#60095,#44781,#44782);
#36719=AXIS2_PLACEMENT_3D('',#60097,#44784,#44785);
#36720=AXIS2_PLACEMENT_3D('',#60099,#44786,#44787);
#36721=AXIS2_PLACEMENT_3D('',#60100,#44788,#44789);
#36722=AXIS2_PLACEMENT_3D('',#60103,#44791,#44792);
#36723=AXIS2_PLACEMENT_3D('',#60104,#44793,#44794);
#36724=AXIS2_PLACEMENT_3D('',#60107,#44796,#44797);
#36725=AXIS2_PLACEMENT_3D('',#60108,#44798,#44799);
#36726=AXIS2_PLACEMENT_3D('',#60111,#44801,#44802);
#36727=AXIS2_PLACEMENT_3D('',#60112,#44803,#44804);
#36728=AXIS2_PLACEMENT_3D('',#60113,#44805,#44806);
#36729=AXIS2_PLACEMENT_3D('',#60114,#44807,#44808);
#36730=AXIS2_PLACEMENT_3D('',#60117,#44809,#44810);
#36731=AXIS2_PLACEMENT_3D('',#60118,#44811,#44812);
#36732=AXIS2_PLACEMENT_3D('',#60121,#44814,#44815);
#36733=AXIS2_PLACEMENT_3D('',#60122,#44816,#44817);
#36734=AXIS2_PLACEMENT_3D('',#60124,#44818,#44819);
#36735=AXIS2_PLACEMENT_3D('',#60125,#44820,#44821);
#36736=AXIS2_PLACEMENT_3D('',#60127,#44822,#44823);
#36737=AXIS2_PLACEMENT_3D('',#60129,#44825,#44826);
#36738=AXIS2_PLACEMENT_3D('',#60131,#44827,#44828);
#36739=AXIS2_PLACEMENT_3D('',#60135,#44830,#44831);
#36740=AXIS2_PLACEMENT_3D('',#60136,#44832,#44833);
#36741=AXIS2_PLACEMENT_3D('',#60137,#44834,#44835);
#36742=AXIS2_PLACEMENT_3D('',#60140,#44837,#44838);
#36743=AXIS2_PLACEMENT_3D('',#60141,#44839,#44840);
#36744=AXIS2_PLACEMENT_3D('',#60143,#44841,#44842);
#36745=AXIS2_PLACEMENT_3D('',#60144,#44843,#44844);
#36746=AXIS2_PLACEMENT_3D('',#60176,#44845,#44846);
#36747=AXIS2_PLACEMENT_3D('',#60178,#44847,#44848);
#36748=AXIS2_PLACEMENT_3D('',#60179,#44849,#44850);
#36749=AXIS2_PLACEMENT_3D('',#60180,#44851,#44852);
#36750=AXIS2_PLACEMENT_3D('',#60181,#44853,#44854);
#36751=AXIS2_PLACEMENT_3D('',#60188,#44855,#44856);
#36752=AXIS2_PLACEMENT_3D('',#60190,#44857,#44858);
#36753=AXIS2_PLACEMENT_3D('',#60195,#44859,#44860);
#36754=AXIS2_PLACEMENT_3D('',#60197,#44861,#44862);
#36755=AXIS2_PLACEMENT_3D('',#60198,#44863,#44864);
#36756=AXIS2_PLACEMENT_3D('',#60226,#44865,#44866);
#36757=AXIS2_PLACEMENT_3D('',#60227,#44867,#44868);
#36758=AXIS2_PLACEMENT_3D('',#60228,#44869,#44870);
#36759=AXIS2_PLACEMENT_3D('',#60262,#44871,#44872);
#36760=AXIS2_PLACEMENT_3D('',#60264,#44873,#44874);
#36761=AXIS2_PLACEMENT_3D('',#60265,#44875,#44876);
#36762=AXIS2_PLACEMENT_3D('',#60266,#44877,#44878);
#36763=AXIS2_PLACEMENT_3D('',#60267,#44879,#44880);
#36764=AXIS2_PLACEMENT_3D('',#60274,#44881,#44882);
#36765=AXIS2_PLACEMENT_3D('',#60276,#44883,#44884);
#36766=AXIS2_PLACEMENT_3D('',#60281,#44885,#44886);
#36767=AXIS2_PLACEMENT_3D('',#60283,#44887,#44888);
#36768=AXIS2_PLACEMENT_3D('',#60284,#44889,#44890);
#36769=AXIS2_PLACEMENT_3D('',#60316,#44891,#44892);
#36770=AXIS2_PLACEMENT_3D('',#60317,#44893,#44894);
#36771=AXIS2_PLACEMENT_3D('',#60318,#44895,#44896);
#36772=AXIS2_PLACEMENT_3D('',#60352,#44897,#44898);
#36773=AXIS2_PLACEMENT_3D('',#60354,#44899,#44900);
#36774=AXIS2_PLACEMENT_3D('',#60355,#44901,#44902);
#36775=AXIS2_PLACEMENT_3D('',#60356,#44903,#44904);
#36776=AXIS2_PLACEMENT_3D('',#60357,#44905,#44906);
#36777=AXIS2_PLACEMENT_3D('',#60364,#44907,#44908);
#36778=AXIS2_PLACEMENT_3D('',#60366,#44909,#44910);
#36779=AXIS2_PLACEMENT_3D('',#60371,#44911,#44912);
#36780=AXIS2_PLACEMENT_3D('',#60373,#44913,#44914);
#36781=AXIS2_PLACEMENT_3D('',#60374,#44915,#44916);
#36782=AXIS2_PLACEMENT_3D('',#60406,#44917,#44918);
#36783=AXIS2_PLACEMENT_3D('',#60407,#44919,#44920);
#36784=AXIS2_PLACEMENT_3D('',#60408,#44921,#44922);
#36785=AXIS2_PLACEMENT_3D('',#60440,#44923,#44924);
#36786=AXIS2_PLACEMENT_3D('',#60442,#44925,#44926);
#36787=AXIS2_PLACEMENT_3D('',#60443,#44927,#44928);
#36788=AXIS2_PLACEMENT_3D('',#60444,#44929,#44930);
#36789=AXIS2_PLACEMENT_3D('',#60445,#44931,#44932);
#36790=AXIS2_PLACEMENT_3D('',#60452,#44933,#44934);
#36791=AXIS2_PLACEMENT_3D('',#60454,#44935,#44936);
#36792=AXIS2_PLACEMENT_3D('',#60459,#44937,#44938);
#36793=AXIS2_PLACEMENT_3D('',#60461,#44939,#44940);
#36794=AXIS2_PLACEMENT_3D('',#60462,#44941,#44942);
#36795=AXIS2_PLACEMENT_3D('',#60490,#44943,#44944);
#36796=AXIS2_PLACEMENT_3D('',#60491,#44945,#44946);
#36797=AXIS2_PLACEMENT_3D('',#60492,#44947,#44948);
#36798=AXIS2_PLACEMENT_3D('',#60524,#44949,#44950);
#36799=AXIS2_PLACEMENT_3D('',#60526,#44951,#44952);
#36800=AXIS2_PLACEMENT_3D('',#60527,#44953,#44954);
#36801=AXIS2_PLACEMENT_3D('',#60528,#44955,#44956);
#36802=AXIS2_PLACEMENT_3D('',#60529,#44957,#44958);
#36803=AXIS2_PLACEMENT_3D('',#60536,#44959,#44960);
#36804=AXIS2_PLACEMENT_3D('',#60538,#44961,#44962);
#36805=AXIS2_PLACEMENT_3D('',#60543,#44963,#44964);
#36806=AXIS2_PLACEMENT_3D('',#60545,#44965,#44966);
#36807=AXIS2_PLACEMENT_3D('',#60546,#44967,#44968);
#36808=AXIS2_PLACEMENT_3D('',#60578,#44969,#44970);
#36809=AXIS2_PLACEMENT_3D('',#60579,#44971,#44972);
#36810=AXIS2_PLACEMENT_3D('',#60580,#44973,#44974);
#36811=AXIS2_PLACEMENT_3D('',#60612,#44975,#44976);
#36812=AXIS2_PLACEMENT_3D('',#60614,#44977,#44978);
#36813=AXIS2_PLACEMENT_3D('',#60615,#44979,#44980);
#36814=AXIS2_PLACEMENT_3D('',#60616,#44981,#44982);
#36815=AXIS2_PLACEMENT_3D('',#60617,#44983,#44984);
#36816=AXIS2_PLACEMENT_3D('',#60624,#44985,#44986);
#36817=AXIS2_PLACEMENT_3D('',#60626,#44987,#44988);
#36818=AXIS2_PLACEMENT_3D('',#60631,#44989,#44990);
#36819=AXIS2_PLACEMENT_3D('',#60633,#44991,#44992);
#36820=AXIS2_PLACEMENT_3D('',#60634,#44993,#44994);
#36821=AXIS2_PLACEMENT_3D('',#60662,#44995,#44996);
#36822=AXIS2_PLACEMENT_3D('',#60663,#44997,#44998);
#36823=AXIS2_PLACEMENT_3D('',#60664,#44999,#45000);
#36824=AXIS2_PLACEMENT_3D('',#60698,#45001,#45002);
#36825=AXIS2_PLACEMENT_3D('',#60700,#45003,#45004);
#36826=AXIS2_PLACEMENT_3D('',#60701,#45005,#45006);
#36827=AXIS2_PLACEMENT_3D('',#60702,#45007,#45008);
#36828=AXIS2_PLACEMENT_3D('',#60703,#45009,#45010);
#36829=AXIS2_PLACEMENT_3D('',#60710,#45011,#45012);
#36830=AXIS2_PLACEMENT_3D('',#60712,#45013,#45014);
#36831=AXIS2_PLACEMENT_3D('',#60717,#45015,#45016);
#36832=AXIS2_PLACEMENT_3D('',#60719,#45017,#45018);
#36833=AXIS2_PLACEMENT_3D('',#60720,#45019,#45020);
#36834=AXIS2_PLACEMENT_3D('',#60752,#45021,#45022);
#36835=AXIS2_PLACEMENT_3D('',#60753,#45023,#45024);
#36836=AXIS2_PLACEMENT_3D('',#60754,#45025,#45026);
#36837=AXIS2_PLACEMENT_3D('',#60788,#45027,#45028);
#36838=AXIS2_PLACEMENT_3D('',#60790,#45029,#45030);
#36839=AXIS2_PLACEMENT_3D('',#60791,#45031,#45032);
#36840=AXIS2_PLACEMENT_3D('',#60792,#45033,#45034);
#36841=AXIS2_PLACEMENT_3D('',#60793,#45035,#45036);
#36842=AXIS2_PLACEMENT_3D('',#60800,#45037,#45038);
#36843=AXIS2_PLACEMENT_3D('',#60802,#45039,#45040);
#36844=AXIS2_PLACEMENT_3D('',#60807,#45041,#45042);
#36845=AXIS2_PLACEMENT_3D('',#60809,#45043,#45044);
#36846=AXIS2_PLACEMENT_3D('',#60810,#45045,#45046);
#36847=AXIS2_PLACEMENT_3D('',#60842,#45047,#45048);
#36848=AXIS2_PLACEMENT_3D('',#60843,#45049,#45050);
#36849=AXIS2_PLACEMENT_3D('',#60844,#45051,#45052);
#36850=AXIS2_PLACEMENT_3D('',#60876,#45053,#45054);
#36851=AXIS2_PLACEMENT_3D('',#60878,#45055,#45056);
#36852=AXIS2_PLACEMENT_3D('',#60879,#45057,#45058);
#36853=AXIS2_PLACEMENT_3D('',#60880,#45059,#45060);
#36854=AXIS2_PLACEMENT_3D('',#60881,#45061,#45062);
#36855=AXIS2_PLACEMENT_3D('',#60888,#45063,#45064);
#36856=AXIS2_PLACEMENT_3D('',#60890,#45065,#45066);
#36857=AXIS2_PLACEMENT_3D('',#60895,#45067,#45068);
#36858=AXIS2_PLACEMENT_3D('',#60897,#45069,#45070);
#36859=AXIS2_PLACEMENT_3D('',#60898,#45071,#45072);
#36860=AXIS2_PLACEMENT_3D('',#60926,#45073,#45074);
#36861=AXIS2_PLACEMENT_3D('',#60927,#45075,#45076);
#36862=AXIS2_PLACEMENT_3D('',#60928,#45077,#45078);
#36863=AXIS2_PLACEMENT_3D('',#60948,#45079,#45080);
#36864=AXIS2_PLACEMENT_3D('',#60950,#45081,#45082);
#36865=AXIS2_PLACEMENT_3D('',#60951,#45083,#45084);
#36866=AXIS2_PLACEMENT_3D('',#60953,#45085,#45086);
#36867=AXIS2_PLACEMENT_3D('',#60970,#45087,#45088);
#36868=AXIS2_PLACEMENT_3D('',#60977,#45089,#45090);
#36869=AXIS2_PLACEMENT_3D('',#60979,#45091,#45092);
#36870=AXIS2_PLACEMENT_3D('',#60984,#45093,#45094);
#36871=AXIS2_PLACEMENT_3D('',#60986,#45095,#45096);
#36872=AXIS2_PLACEMENT_3D('',#60987,#45097,#45098);
#36873=AXIS2_PLACEMENT_3D('',#61024,#45099,#45100);
#36874=AXIS2_PLACEMENT_3D('',#61025,#45101,#45102);
#36875=AXIS2_PLACEMENT_3D('',#61026,#45103,#45104);
#36876=AXIS2_PLACEMENT_3D('',#61058,#45105,#45106);
#36877=AXIS2_PLACEMENT_3D('',#61060,#45107,#45108);
#36878=AXIS2_PLACEMENT_3D('',#61061,#45109,#45110);
#36879=AXIS2_PLACEMENT_3D('',#61062,#45111,#45112);
#36880=AXIS2_PLACEMENT_3D('',#61063,#45113,#45114);
#36881=AXIS2_PLACEMENT_3D('',#61070,#45115,#45116);
#36882=AXIS2_PLACEMENT_3D('',#61072,#45117,#45118);
#36883=AXIS2_PLACEMENT_3D('',#61077,#45119,#45120);
#36884=AXIS2_PLACEMENT_3D('',#61079,#45121,#45122);
#36885=AXIS2_PLACEMENT_3D('',#61080,#45123,#45124);
#36886=AXIS2_PLACEMENT_3D('',#61108,#45125,#45126);
#36887=AXIS2_PLACEMENT_3D('',#61109,#45127,#45128);
#36888=AXIS2_PLACEMENT_3D('',#61110,#45129,#45130);
#36889=AXIS2_PLACEMENT_3D('',#61144,#45131,#45132);
#36890=AXIS2_PLACEMENT_3D('',#61146,#45133,#45134);
#36891=AXIS2_PLACEMENT_3D('',#61147,#45135,#45136);
#36892=AXIS2_PLACEMENT_3D('',#61148,#45137,#45138);
#36893=AXIS2_PLACEMENT_3D('',#61149,#45139,#45140);
#36894=AXIS2_PLACEMENT_3D('',#61156,#45141,#45142);
#36895=AXIS2_PLACEMENT_3D('',#61158,#45143,#45144);
#36896=AXIS2_PLACEMENT_3D('',#61163,#45145,#45146);
#36897=AXIS2_PLACEMENT_3D('',#61165,#45147,#45148);
#36898=AXIS2_PLACEMENT_3D('',#61166,#45149,#45150);
#36899=AXIS2_PLACEMENT_3D('',#61198,#45151,#45152);
#36900=AXIS2_PLACEMENT_3D('',#61199,#45153,#45154);
#36901=AXIS2_PLACEMENT_3D('',#61200,#45155,#45156);
#36902=AXIS2_PLACEMENT_3D('',#61234,#45157,#45158);
#36903=AXIS2_PLACEMENT_3D('',#61236,#45159,#45160);
#36904=AXIS2_PLACEMENT_3D('',#61237,#45161,#45162);
#36905=AXIS2_PLACEMENT_3D('',#61238,#45163,#45164);
#36906=AXIS2_PLACEMENT_3D('',#61239,#45165,#45166);
#36907=AXIS2_PLACEMENT_3D('',#61246,#45167,#45168);
#36908=AXIS2_PLACEMENT_3D('',#61248,#45169,#45170);
#36909=AXIS2_PLACEMENT_3D('',#61253,#45171,#45172);
#36910=AXIS2_PLACEMENT_3D('',#61255,#45173,#45174);
#36911=AXIS2_PLACEMENT_3D('',#61256,#45175,#45176);
#36912=AXIS2_PLACEMENT_3D('',#61288,#45177,#45178);
#36913=AXIS2_PLACEMENT_3D('',#61289,#45179,#45180);
#36914=AXIS2_PLACEMENT_3D('',#61290,#45181,#45182);
#36915=AXIS2_PLACEMENT_3D('',#61322,#45183,#45184);
#36916=AXIS2_PLACEMENT_3D('',#61324,#45185,#45186);
#36917=AXIS2_PLACEMENT_3D('',#61325,#45187,#45188);
#36918=AXIS2_PLACEMENT_3D('',#61326,#45189,#45190);
#36919=AXIS2_PLACEMENT_3D('',#61327,#45191,#45192);
#36920=AXIS2_PLACEMENT_3D('',#61334,#45193,#45194);
#36921=AXIS2_PLACEMENT_3D('',#61336,#45195,#45196);
#36922=AXIS2_PLACEMENT_3D('',#61341,#45197,#45198);
#36923=AXIS2_PLACEMENT_3D('',#61343,#45199,#45200);
#36924=AXIS2_PLACEMENT_3D('',#61344,#45201,#45202);
#36925=AXIS2_PLACEMENT_3D('',#61372,#45203,#45204);
#36926=AXIS2_PLACEMENT_3D('',#61373,#45205,#45206);
#36927=AXIS2_PLACEMENT_3D('',#61374,#45207,#45208);
#36928=AXIS2_PLACEMENT_3D('',#61406,#45209,#45210);
#36929=AXIS2_PLACEMENT_3D('',#61408,#45211,#45212);
#36930=AXIS2_PLACEMENT_3D('',#61409,#45213,#45214);
#36931=AXIS2_PLACEMENT_3D('',#61410,#45215,#45216);
#36932=AXIS2_PLACEMENT_3D('',#61411,#45217,#45218);
#36933=AXIS2_PLACEMENT_3D('',#61418,#45219,#45220);
#36934=AXIS2_PLACEMENT_3D('',#61420,#45221,#45222);
#36935=AXIS2_PLACEMENT_3D('',#61425,#45223,#45224);
#36936=AXIS2_PLACEMENT_3D('',#61427,#45225,#45226);
#36937=AXIS2_PLACEMENT_3D('',#61428,#45227,#45228);
#36938=AXIS2_PLACEMENT_3D('',#61460,#45229,#45230);
#36939=AXIS2_PLACEMENT_3D('',#61461,#45231,#45232);
#36940=AXIS2_PLACEMENT_3D('',#61462,#45233,#45234);
#36941=AXIS2_PLACEMENT_3D('',#61494,#45235,#45236);
#36942=AXIS2_PLACEMENT_3D('',#61496,#45237,#45238);
#36943=AXIS2_PLACEMENT_3D('',#61497,#45239,#45240);
#36944=AXIS2_PLACEMENT_3D('',#61498,#45241,#45242);
#36945=AXIS2_PLACEMENT_3D('',#61499,#45243,#45244);
#36946=AXIS2_PLACEMENT_3D('',#61506,#45245,#45246);
#36947=AXIS2_PLACEMENT_3D('',#61508,#45247,#45248);
#36948=AXIS2_PLACEMENT_3D('',#61513,#45249,#45250);
#36949=AXIS2_PLACEMENT_3D('',#61515,#45251,#45252);
#36950=AXIS2_PLACEMENT_3D('',#61516,#45253,#45254);
#36951=AXIS2_PLACEMENT_3D('',#61544,#45255,#45256);
#36952=AXIS2_PLACEMENT_3D('',#61545,#45257,#45258);
#36953=AXIS2_PLACEMENT_3D('',#61546,#45259,#45260);
#36954=AXIS2_PLACEMENT_3D('',#61580,#45261,#45262);
#36955=AXIS2_PLACEMENT_3D('',#61582,#45263,#45264);
#36956=AXIS2_PLACEMENT_3D('',#61583,#45265,#45266);
#36957=AXIS2_PLACEMENT_3D('',#61584,#45267,#45268);
#36958=AXIS2_PLACEMENT_3D('',#61585,#45269,#45270);
#36959=AXIS2_PLACEMENT_3D('',#61592,#45271,#45272);
#36960=AXIS2_PLACEMENT_3D('',#61594,#45273,#45274);
#36961=AXIS2_PLACEMENT_3D('',#61599,#45275,#45276);
#36962=AXIS2_PLACEMENT_3D('',#61601,#45277,#45278);
#36963=AXIS2_PLACEMENT_3D('',#61602,#45279,#45280);
#36964=AXIS2_PLACEMENT_3D('',#61634,#45281,#45282);
#36965=AXIS2_PLACEMENT_3D('',#61635,#45283,#45284);
#36966=AXIS2_PLACEMENT_3D('',#61636,#45285,#45286);
#36967=AXIS2_PLACEMENT_3D('',#61670,#45287,#45288);
#36968=AXIS2_PLACEMENT_3D('',#61672,#45289,#45290);
#36969=AXIS2_PLACEMENT_3D('',#61673,#45291,#45292);
#36970=AXIS2_PLACEMENT_3D('',#61674,#45293,#45294);
#36971=AXIS2_PLACEMENT_3D('',#61675,#45295,#45296);
#36972=AXIS2_PLACEMENT_3D('',#61682,#45297,#45298);
#36973=AXIS2_PLACEMENT_3D('',#61684,#45299,#45300);
#36974=AXIS2_PLACEMENT_3D('',#61689,#45301,#45302);
#36975=AXIS2_PLACEMENT_3D('',#61691,#45303,#45304);
#36976=AXIS2_PLACEMENT_3D('',#61692,#45305,#45306);
#36977=AXIS2_PLACEMENT_3D('',#61724,#45307,#45308);
#36978=AXIS2_PLACEMENT_3D('',#61725,#45309,#45310);
#36979=AXIS2_PLACEMENT_3D('',#61726,#45311,#45312);
#36980=AXIS2_PLACEMENT_3D('',#61758,#45313,#45314);
#36981=AXIS2_PLACEMENT_3D('',#61760,#45315,#45316);
#36982=AXIS2_PLACEMENT_3D('',#61761,#45317,#45318);
#36983=AXIS2_PLACEMENT_3D('',#61762,#45319,#45320);
#36984=AXIS2_PLACEMENT_3D('',#61763,#45321,#45322);
#36985=AXIS2_PLACEMENT_3D('',#61770,#45323,#45324);
#36986=AXIS2_PLACEMENT_3D('',#61772,#45325,#45326);
#36987=AXIS2_PLACEMENT_3D('',#61777,#45327,#45328);
#36988=AXIS2_PLACEMENT_3D('',#61779,#45329,#45330);
#36989=AXIS2_PLACEMENT_3D('',#61780,#45331,#45332);
#36990=AXIS2_PLACEMENT_3D('',#61808,#45333,#45334);
#36991=AXIS2_PLACEMENT_3D('',#61809,#45335,#45336);
#36992=AXIS2_PLACEMENT_3D('',#61810,#45337,#45338);
#36993=AXIS2_PLACEMENT_3D('',#61842,#45339,#45340);
#36994=AXIS2_PLACEMENT_3D('',#61844,#45341,#45342);
#36995=AXIS2_PLACEMENT_3D('',#61845,#45343,#45344);
#36996=AXIS2_PLACEMENT_3D('',#61846,#45345,#45346);
#36997=AXIS2_PLACEMENT_3D('',#61847,#45347,#45348);
#36998=AXIS2_PLACEMENT_3D('',#61854,#45349,#45350);
#36999=AXIS2_PLACEMENT_3D('',#61856,#45351,#45352);
#37000=AXIS2_PLACEMENT_3D('',#61861,#45353,#45354);
#37001=AXIS2_PLACEMENT_3D('',#61863,#45355,#45356);
#37002=AXIS2_PLACEMENT_3D('',#61864,#45357,#45358);
#37003=AXIS2_PLACEMENT_3D('',#61896,#45359,#45360);
#37004=AXIS2_PLACEMENT_3D('',#61897,#45361,#45362);
#37005=AXIS2_PLACEMENT_3D('',#61898,#45363,#45364);
#37006=AXIS2_PLACEMENT_3D('',#61901,#45366,#45367);
#37007=AXIS2_PLACEMENT_3D('',#61902,#45368,#45369);
#37008=AXIS2_PLACEMENT_3D('',#61905,#45372,#45373);
#37009=AXIS2_PLACEMENT_3D('',#61907,#45374,#45375);
#37010=AXIS2_PLACEMENT_3D('',#61909,#45377,#45378);
#37011=AXIS2_PLACEMENT_3D('',#61911,#45379,#45380);
#37012=AXIS2_PLACEMENT_3D('',#61912,#45381,#45382);
#37013=AXIS2_PLACEMENT_3D('',#61915,#45384,#45385);
#37014=AXIS2_PLACEMENT_3D('',#61916,#45386,#45387);
#37015=AXIS2_PLACEMENT_3D('',#61919,#45389,#45390);
#37016=AXIS2_PLACEMENT_3D('',#61920,#45391,#45392);
#37017=AXIS2_PLACEMENT_3D('',#61923,#45394,#45395);
#37018=AXIS2_PLACEMENT_3D('',#61924,#45396,#45397);
#37019=AXIS2_PLACEMENT_3D('',#61925,#45398,#45399);
#37020=AXIS2_PLACEMENT_3D('',#61926,#45400,#45401);
#37021=AXIS2_PLACEMENT_3D('',#61935,#45406,#45407);
#37022=AXIS2_PLACEMENT_3D('',#61945,#45413,#45414);
#37023=AXIS2_PLACEMENT_3D('',#61949,#45417,#45418);
#37024=AXIS2_PLACEMENT_3D('',#61953,#45421,#45422);
#37025=AXIS2_PLACEMENT_3D('',#61959,#45426,#45427);
#37026=AXIS2_PLACEMENT_3D('',#61961,#45428,#45429);
#37027=AXIS2_PLACEMENT_3D('',#61962,#45430,#45431);
#37028=AXIS2_PLACEMENT_3D('',#61963,#45432,#45433);
#37029=AXIS2_PLACEMENT_3D('',#61964,#45434,#45435);
#37030=AXIS2_PLACEMENT_3D('',#61965,#45436,#45437);
#37031=AXIS2_PLACEMENT_3D('',#61967,#45438,#45439);
#37032=AXIS2_PLACEMENT_3D('',#61968,#45440,#45441);
#37033=AXIS2_PLACEMENT_3D('',#61970,#45442,#45443);
#37034=AXIS2_PLACEMENT_3D('',#61972,#45445,#45446);
#37035=AXIS2_PLACEMENT_3D('',#61974,#45447,#45448);
#37036=AXIS2_PLACEMENT_3D('',#61976,#45450,#45451);
#37037=AXIS2_PLACEMENT_3D('',#61978,#45453,#45454);
#37038=AXIS2_PLACEMENT_3D('',#61979,#45455,#45456);
#37039=AXIS2_PLACEMENT_3D('',#61994,#45460,#45461);
#37040=AXIS2_PLACEMENT_3D('',#61996,#45462,#45463);
#37041=AXIS2_PLACEMENT_3D('',#61999,#45465,#45466);
#37042=AXIS2_PLACEMENT_3D('',#62000,#45467,#45468);
#37043=AXIS2_PLACEMENT_3D('',#62024,#45469,#45470);
#37044=AXIS2_PLACEMENT_3D('',#62036,#45475,#45476);
#37045=AXIS2_PLACEMENT_3D('',#62040,#45479,#45480);
#37046=AXIS2_PLACEMENT_3D('',#62046,#45484,#45485);
#37047=AXIS2_PLACEMENT_3D('',#62056,#45491,#45492);
#37048=AXIS2_PLACEMENT_3D('',#62066,#45496,#45497);
#37049=AXIS2_PLACEMENT_3D('',#62071,#45500,#45501);
#37050=AXIS2_PLACEMENT_3D('',#62072,#45502,#45503);
#37051=AXIS2_PLACEMENT_3D('',#62080,#45508,#45509);
#37052=AXIS2_PLACEMENT_3D('',#62086,#45511,#45512);
#37053=AXIS2_PLACEMENT_3D('',#62093,#45513,#45514);
#37054=AXIS2_PLACEMENT_3D('',#62098,#45515,#45516);
#37055=AXIS2_PLACEMENT_3D('',#62111,#45521,#45522);
#37056=AXIS2_PLACEMENT_3D('',#62129,#45528,#45529);
#37057=AXIS2_PLACEMENT_3D('',#62137,#45534,#45535);
#37058=AXIS2_PLACEMENT_3D('',#62140,#45538,#45539);
#37059=AXIS2_PLACEMENT_3D('',#62155,#45543,#45544);
#37060=AXIS2_PLACEMENT_3D('',#62157,#45545,#45546);
#37061=AXIS2_PLACEMENT_3D('',#62168,#45547,#45548);
#37062=AXIS2_PLACEMENT_3D('',#62173,#45549,#45550);
#37063=AXIS2_PLACEMENT_3D('',#62175,#45551,#45552);
#37064=AXIS2_PLACEMENT_3D('',#62177,#45554,#45555);
#37065=AXIS2_PLACEMENT_3D('',#62201,#45556,#45557);
#37066=AXIS2_PLACEMENT_3D('',#62204,#45560,#45561);
#37067=AXIS2_PLACEMENT_3D('',#62212,#45564,#45565);
#37068=AXIS2_PLACEMENT_3D('',#62222,#45569,#45570);
#37069=AXIS2_PLACEMENT_3D('',#62224,#45571,#45572);
#37070=AXIS2_PLACEMENT_3D('',#62260,#45574,#45575);
#37071=AXIS2_PLACEMENT_3D('',#62275,#45579,#45580);
#37072=AXIS2_PLACEMENT_3D('',#62277,#45581,#45582);
#37073=AXIS2_PLACEMENT_3D('',#62280,#45584,#45585);
#37074=AXIS2_PLACEMENT_3D('',#62281,#45586,#45587);
#37075=AXIS2_PLACEMENT_3D('',#62305,#45588,#45589);
#37076=AXIS2_PLACEMENT_3D('',#62317,#45594,#45595);
#37077=AXIS2_PLACEMENT_3D('',#62321,#45598,#45599);
#37078=AXIS2_PLACEMENT_3D('',#62327,#45603,#45604);
#37079=AXIS2_PLACEMENT_3D('',#62330,#45607,#45608);
#37080=AXIS2_PLACEMENT_3D('',#62334,#45611,#45612);
#37081=AXIS2_PLACEMENT_3D('',#62338,#45615,#45616);
#37082=AXIS2_PLACEMENT_3D('',#62340,#45618,#45619);
#37083=AXIS2_PLACEMENT_3D('',#62346,#45623,#45624);
#37084=AXIS2_PLACEMENT_3D('',#62350,#45627,#45628);
#37085=AXIS2_PLACEMENT_3D('',#62354,#45631,#45632);
#37086=AXIS2_PLACEMENT_3D('',#62362,#45637,#45638);
#37087=AXIS2_PLACEMENT_3D('',#62372,#45642,#45643);
#37088=AXIS2_PLACEMENT_3D('',#62377,#45646,#45647);
#37089=AXIS2_PLACEMENT_3D('',#62378,#45648,#45649);
#37090=AXIS2_PLACEMENT_3D('',#62386,#45654,#45655);
#37091=AXIS2_PLACEMENT_3D('',#62392,#45657,#45658);
#37092=AXIS2_PLACEMENT_3D('',#62399,#45659,#45660);
#37093=AXIS2_PLACEMENT_3D('',#62404,#45661,#45662);
#37094=AXIS2_PLACEMENT_3D('',#62414,#45668,#45669);
#37095=AXIS2_PLACEMENT_3D('',#62418,#45672,#45673);
#37096=AXIS2_PLACEMENT_3D('',#62424,#45675,#45676);
#37097=AXIS2_PLACEMENT_3D('',#62434,#45677,#45678);
#37098=AXIS2_PLACEMENT_3D('',#62446,#45679,#45680);
#37099=AXIS2_PLACEMENT_3D('',#62456,#45684,#45685);
#37100=AXIS2_PLACEMENT_3D('',#62457,#45686,#45687);
#37101=AXIS2_PLACEMENT_3D('',#62458,#45688,#45689);
#37102=AXIS2_PLACEMENT_3D('',#62472,#45695,#45696);
#37103=AXIS2_PLACEMENT_3D('',#62478,#45700,#45701);
#37104=AXIS2_PLACEMENT_3D('',#62484,#45703,#45704);
#37105=AXIS2_PLACEMENT_3D('',#62498,#45708,#45709);
#37106=AXIS2_PLACEMENT_3D('',#62500,#45711,#45712);
#37107=AXIS2_PLACEMENT_3D('',#62510,#45716,#45717);
#37108=AXIS2_PLACEMENT_3D('',#62518,#45720,#45721);
#37109=AXIS2_PLACEMENT_3D('',#62520,#45722,#45723);
#37110=AXIS2_PLACEMENT_3D('',#62526,#45724,#45725);
#37111=AXIS2_PLACEMENT_3D('',#62530,#45726,#45727);
#37112=AXIS2_PLACEMENT_3D('',#62532,#45729,#45730);
#37113=AXIS2_PLACEMENT_3D('',#62535,#45733,#45734);
#37114=AXIS2_PLACEMENT_3D('',#62536,#45735,#45736);
#37115=AXIS2_PLACEMENT_3D('',#62543,#45738,#45739);
#37116=AXIS2_PLACEMENT_3D('',#62550,#45741,#45742);
#37117=AXIS2_PLACEMENT_3D('',#62557,#45744,#45745);
#37118=AXIS2_PLACEMENT_3D('',#62566,#45748,#45749);
#37119=AXIS2_PLACEMENT_3D('',#62573,#45751,#45752);
#37120=AXIS2_PLACEMENT_3D('',#62580,#45754,#45755);
#37121=AXIS2_PLACEMENT_3D('',#62596,#45759,#45760);
#37122=AXIS2_PLACEMENT_3D('',#62600,#45761,#45762);
#37123=AXIS2_PLACEMENT_3D('',#62601,#45763,#45764);
#37124=AXIS2_PLACEMENT_3D('',#62603,#45765,#45766);
#37125=AXIS2_PLACEMENT_3D('',#62604,#45767,#45768);
#37126=AXIS2_PLACEMENT_3D('',#62608,#45769,#45770);
#37127=AXIS2_PLACEMENT_3D('',#62617,#45773,#45774);
#37128=AXIS2_PLACEMENT_3D('',#62621,#45775,#45776);
#37129=AXIS2_PLACEMENT_3D('',#62622,#45777,#45778);
#37130=AXIS2_PLACEMENT_3D('',#62623,#45779,#45780);
#37131=AXIS2_PLACEMENT_3D('',#62624,#45781,#45782);
#37132=AXIS2_PLACEMENT_3D('',#62631,#45784,#45785);
#37133=AXIS2_PLACEMENT_3D('',#62633,#45786,#45787);
#37134=AXIS2_PLACEMENT_3D('',#62637,#45789,#45790);
#37135=AXIS2_PLACEMENT_3D('',#62641,#45792,#45793);
#37136=AXIS2_PLACEMENT_3D('',#62645,#45795,#45796);
#37137=AXIS2_PLACEMENT_3D('',#62649,#45798,#45799);
#37138=AXIS2_PLACEMENT_3D('',#62650,#45800,#45801);
#37139=AXIS2_PLACEMENT_3D('',#62651,#45802,#45803);
#37140=AXIS2_PLACEMENT_3D('',#62652,#45804,#45805);
#37141=AXIS2_PLACEMENT_3D('',#62659,#45806,#45807);
#37142=AXIS2_PLACEMENT_3D('',#62663,#45808,#45809);
#37143=AXIS2_PLACEMENT_3D('',#62671,#45812,#45813);
#37144=AXIS2_PLACEMENT_3D('',#62679,#45816,#45817);
#37145=AXIS2_PLACEMENT_3D('',#62681,#45819,#45820);
#37146=AXIS2_PLACEMENT_3D('',#62698,#45821,#45822);
#37147=AXIS2_PLACEMENT_3D('',#62702,#45823,#45824);
#37148=AXIS2_PLACEMENT_3D('',#62708,#45828,#45829);
#37149=AXIS2_PLACEMENT_3D('',#62715,#45832,#45833);
#37150=AXIS2_PLACEMENT_3D('',#62723,#45836,#45837);
#37151=AXIS2_PLACEMENT_3D('',#62730,#45839,#45840);
#37152=AXIS2_PLACEMENT_3D('',#62734,#45843,#45844);
#37153=AXIS2_PLACEMENT_3D('',#62737,#45847,#45848);
#37154=AXIS2_PLACEMENT_3D('',#62744,#45850,#45851);
#37155=AXIS2_PLACEMENT_3D('',#62750,#45852,#45853);
#37156=AXIS2_PLACEMENT_3D('',#62754,#45854,#45855);
#37157=AXIS2_PLACEMENT_3D('',#62762,#45858,#45859);
#37158=AXIS2_PLACEMENT_3D('',#62763,#45860,#45861);
#37159=AXIS2_PLACEMENT_3D('',#62764,#45862,#45863);
#37160=AXIS2_PLACEMENT_3D('',#62770,#45865,#45866);
#37161=AXIS2_PLACEMENT_3D('',#62775,#45867,#45868);
#37162=AXIS2_PLACEMENT_3D('',#62776,#45869,#45870);
#37163=AXIS2_PLACEMENT_3D('',#62777,#45871,#45872);
#37164=AXIS2_PLACEMENT_3D('',#62778,#45873,#45874);
#37165=AXIS2_PLACEMENT_3D('',#62779,#45875,#45876);
#37166=AXIS2_PLACEMENT_3D('',#62787,#45879,#45880);
#37167=AXIS2_PLACEMENT_3D('',#62792,#45884,#45885);
#37168=AXIS2_PLACEMENT_3D('',#62796,#45888,#45889);
#37169=AXIS2_PLACEMENT_3D('',#62800,#45892,#45893);
#37170=AXIS2_PLACEMENT_3D('',#62804,#45896,#45897);
#37171=AXIS2_PLACEMENT_3D('',#62805,#45898,#45899);
#37172=AXIS2_PLACEMENT_3D('',#62806,#45900,#45901);
#37173=AXIS2_PLACEMENT_3D('',#62810,#45902,#45903);
#37174=AXIS2_PLACEMENT_3D('',#62812,#45904,#45905);
#37175=AXIS2_PLACEMENT_3D('',#62814,#45907,#45908);
#37176=AXIS2_PLACEMENT_3D('',#62816,#45910,#45911);
#37177=AXIS2_PLACEMENT_3D('',#62818,#45913,#45914);
#37178=AXIS2_PLACEMENT_3D('',#62819,#45915,#45916);
#37179=AXIS2_PLACEMENT_3D('',#62820,#45917,#45918);
#37180=AXIS2_PLACEMENT_3D('',#62821,#45919,#45920);
#37181=AXIS2_PLACEMENT_3D('',#62823,#45922,#45923);
#37182=AXIS2_PLACEMENT_3D('',#62824,#45924,#45925);
#37183=AXIS2_PLACEMENT_3D('',#62825,#45926,#45927);
#37184=AXIS2_PLACEMENT_3D('',#62826,#45928,#45929);
#37185=AXIS2_PLACEMENT_3D('',#62827,#45930,#45931);
#37186=AXIS2_PLACEMENT_3D('',#62828,#45932,#45933);
#37187=AXIS2_PLACEMENT_3D('',#62838,#45934,#45935);
#37188=AXIS2_PLACEMENT_3D('',#62840,#45936,#45937);
#37189=AXIS2_PLACEMENT_3D('',#62848,#45938,#45939);
#37190=AXIS2_PLACEMENT_3D('',#62849,#45940,#45941);
#37191=AXIS2_PLACEMENT_3D('',#62869,#45943,#45944);
#37192=AXIS2_PLACEMENT_3D('',#62873,#45946,#45947);
#37193=AXIS2_PLACEMENT_3D('',#62877,#45949,#45950);
#37194=AXIS2_PLACEMENT_3D('',#62881,#45952,#45953);
#37195=AXIS2_PLACEMENT_3D('',#62884,#45955,#45956);
#37196=AXIS2_PLACEMENT_3D('',#62885,#45957,#45958);
#37197=AXIS2_PLACEMENT_3D('',#62895,#45962,#45963);
#37198=AXIS2_PLACEMENT_3D('',#62902,#45964,#45965);
#37199=AXIS2_PLACEMENT_3D('',#62911,#45966,#45967);
#37200=AXIS2_PLACEMENT_3D('',#62916,#45971,#45972);
#37201=AXIS2_PLACEMENT_3D('',#62920,#45975,#45976);
#37202=AXIS2_PLACEMENT_3D('',#62930,#45980,#45981);
#37203=AXIS2_PLACEMENT_3D('',#62936,#45985,#45986);
#37204=AXIS2_PLACEMENT_3D('',#62950,#45989,#45990);
#37205=AXIS2_PLACEMENT_3D('',#62955,#45992,#45993);
#37206=AXIS2_PLACEMENT_3D('',#62957,#45995,#45996);
#37207=AXIS2_PLACEMENT_3D('',#62958,#45997,#45998);
#37208=AXIS2_PLACEMENT_3D('',#62959,#45999,#46000);
#37209=AXIS2_PLACEMENT_3D('',#62960,#46001,#46002);
#37210=AXIS2_PLACEMENT_3D('',#62961,#46003,#46004);
#37211=AXIS2_PLACEMENT_3D('',#62962,#46005,#46006);
#37212=AXIS2_PLACEMENT_3D('',#62964,#46007,#46008);
#37213=AXIS2_PLACEMENT_3D('',#62965,#46009,#46010);
#37214=AXIS2_PLACEMENT_3D('',#62989,#46011,#46012);
#37215=AXIS2_PLACEMENT_3D('',#62990,#46013,#46014);
#37216=AXIS2_PLACEMENT_3D('',#62991,#46015,#46016);
#37217=AXIS2_PLACEMENT_3D('',#62994,#46017,#46018);
#37218=AXIS2_PLACEMENT_3D('',#62995,#46019,#46020);
#37219=AXIS2_PLACEMENT_3D('',#62999,#46022,#46023);
#37220=AXIS2_PLACEMENT_3D('',#63000,#46024,#46025);
#37221=AXIS2_PLACEMENT_3D('',#63001,#46026,#46027);
#37222=AXIS2_PLACEMENT_3D('',#63005,#46029,#46030);
#37223=AXIS2_PLACEMENT_3D('',#63006,#46031,#46032);
#37224=AXIS2_PLACEMENT_3D('',#63007,#46033,#46034);
#37225=AXIS2_PLACEMENT_3D('',#63009,#46035,#46036);
#37226=AXIS2_PLACEMENT_3D('',#63011,#46038,#46039);
#37227=AXIS2_PLACEMENT_3D('',#63015,#46041,#46042);
#37228=AXIS2_PLACEMENT_3D('',#63016,#46043,#46044);
#37229=AXIS2_PLACEMENT_3D('',#63017,#46045,#46046);
#37230=AXIS2_PLACEMENT_3D('',#63021,#46048,#46049);
#37231=AXIS2_PLACEMENT_3D('',#63022,#46050,#46051);
#37232=AXIS2_PLACEMENT_3D('',#63023,#46052,#46053);
#37233=AXIS2_PLACEMENT_3D('',#63027,#46055,#46056);
#37234=AXIS2_PLACEMENT_3D('',#63028,#46057,#46058);
#37235=AXIS2_PLACEMENT_3D('',#63029,#46059,#46060);
#37236=AXIS2_PLACEMENT_3D('',#63033,#46062,#46063);
#37237=AXIS2_PLACEMENT_3D('',#63034,#46064,#46065);
#37238=AXIS2_PLACEMENT_3D('',#63035,#46066,#46067);
#37239=AXIS2_PLACEMENT_3D('',#63039,#46069,#46070);
#37240=AXIS2_PLACEMENT_3D('',#63040,#46071,#46072);
#37241=AXIS2_PLACEMENT_3D('',#63041,#46073,#46074);
#37242=AXIS2_PLACEMENT_3D('',#63044,#46076,#46077);
#37243=AXIS2_PLACEMENT_3D('',#63045,#46078,#46079);
#37244=AXIS2_PLACEMENT_3D('',#63047,#46080,#46081);
#37245=AXIS2_PLACEMENT_3D('',#63049,#46082,#46083);
#37246=AXIS2_PLACEMENT_3D('',#63050,#46084,#46085);
#37247=AXIS2_PLACEMENT_3D('',#63052,#46086,#46087);
#37248=AXIS2_PLACEMENT_3D('',#63054,#46089,#46090);
#37249=AXIS2_PLACEMENT_3D('',#63056,#46091,#46092);
#37250=AXIS2_PLACEMENT_3D('',#63058,#46094,#46095);
#37251=AXIS2_PLACEMENT_3D('',#63060,#46096,#46097);
#37252=AXIS2_PLACEMENT_3D('',#63061,#46098,#46099);
#37253=AXIS2_PLACEMENT_3D('',#63063,#46100,#46101);
#37254=AXIS2_PLACEMENT_3D('',#63065,#46103,#46104);
#37255=AXIS2_PLACEMENT_3D('',#63067,#46106,#46107);
#37256=AXIS2_PLACEMENT_3D('',#63068,#46108,#46109);
#37257=AXIS2_PLACEMENT_3D('',#63070,#46110,#46111);
#37258=AXIS2_PLACEMENT_3D('',#63071,#46112,#46113);
#37259=AXIS2_PLACEMENT_3D('',#63074,#46115,#46116);
#37260=AXIS2_PLACEMENT_3D('',#63075,#46117,#46118);
#37261=AXIS2_PLACEMENT_3D('',#63078,#46120,#46121);
#37262=AXIS2_PLACEMENT_3D('',#63079,#46122,#46123);
#37263=AXIS2_PLACEMENT_3D('',#63082,#46125,#46126);
#37264=AXIS2_PLACEMENT_3D('',#63083,#46127,#46128);
#37265=AXIS2_PLACEMENT_3D('',#63086,#46130,#46131);
#37266=AXIS2_PLACEMENT_3D('',#63087,#46132,#46133);
#37267=AXIS2_PLACEMENT_3D('',#63090,#46135,#46136);
#37268=AXIS2_PLACEMENT_3D('',#63091,#46137,#46138);
#37269=AXIS2_PLACEMENT_3D('',#63093,#46140,#46141);
#37270=AXIS2_PLACEMENT_3D('',#63094,#46142,#46143);
#37271=AXIS2_PLACEMENT_3D('',#63116,#46145,#46146);
#37272=AXIS2_PLACEMENT_3D('',#63127,#46147,#46148);
#37273=AXIS2_PLACEMENT_3D('',#63211,#46150,#46151);
#37274=AXIS2_PLACEMENT_3D('',#63301,#46153,#46154);
#37275=AXIS2_PLACEMENT_3D('',#63391,#46156,#46157);
#37276=AXIS2_PLACEMENT_3D('',#63475,#46159,#46160);
#37277=AXIS2_PLACEMENT_3D('',#63565,#46162,#46163);
#37278=AXIS2_PLACEMENT_3D('',#63649,#46165,#46166);
#37279=AXIS2_PLACEMENT_3D('',#63736,#46168,#46169);
#37280=AXIS2_PLACEMENT_3D('',#63826,#46171,#46172);
#37281=AXIS2_PLACEMENT_3D('',#63910,#46174,#46175);
#37282=AXIS2_PLACEMENT_3D('',#64000,#46177,#46178);
#37283=AXIS2_PLACEMENT_3D('',#64090,#46180,#46181);
#37284=AXIS2_PLACEMENT_3D('',#64174,#46183,#46184);
#37285=AXIS2_PLACEMENT_3D('',#64264,#46186,#46187);
#37286=AXIS2_PLACEMENT_3D('',#64351,#46189,#46190);
#37287=AXIS2_PLACEMENT_3D('',#64438,#46192,#46193);
#37288=AXIS2_PLACEMENT_3D('',#64528,#46195,#46196);
#37289=AXIS2_PLACEMENT_3D('',#64612,#46198,#46199);
#37290=AXIS2_PLACEMENT_3D('',#64702,#46201,#46202);
#37291=AXIS2_PLACEMENT_3D('',#64792,#46204,#46205);
#37292=AXIS2_PLACEMENT_3D('',#64876,#46207,#46208);
#37293=AXIS2_PLACEMENT_3D('',#64966,#46210,#46211);
#37294=AXIS2_PLACEMENT_3D('',#65053,#46213,#46214);
#37295=AXIS2_PLACEMENT_3D('',#65140,#46216,#46217);
#37296=AXIS2_PLACEMENT_3D('',#65230,#46219,#46220);
#37297=AXIS2_PLACEMENT_3D('',#65314,#46222,#46223);
#37298=AXIS2_PLACEMENT_3D('',#65404,#46225,#46226);
#37299=AXIS2_PLACEMENT_3D('',#65494,#46228,#46229);
#37300=AXIS2_PLACEMENT_3D('',#65578,#46231,#46232);
#37301=AXIS2_PLACEMENT_3D('',#65587,#46234,#46235);
#37302=AXIS2_PLACEMENT_3D('',#65588,#46236,#46237);
#37303=AXIS2_PLACEMENT_3D('',#65609,#46239,#46240);
#37304=AXIS2_PLACEMENT_3D('',#65624,#46241,#46242);
#37305=AXIS2_PLACEMENT_3D('',#65661,#46244,#46245);
#37306=AXIS2_PLACEMENT_3D('',#65699,#46247,#46248);
#37307=AXIS2_PLACEMENT_3D('',#65736,#46250,#46251);
#37308=AXIS2_PLACEMENT_3D('',#65773,#46253,#46254);
#37309=AXIS2_PLACEMENT_3D('',#65811,#46256,#46257);
#37310=AXIS2_PLACEMENT_3D('',#65847,#46259,#46260);
#37311=AXIS2_PLACEMENT_3D('',#65885,#46262,#46263);
#37312=AXIS2_PLACEMENT_3D('',#65922,#46265,#46266);
#37313=AXIS2_PLACEMENT_3D('',#65959,#46268,#46269);
#37314=AXIS2_PLACEMENT_3D('',#65997,#46271,#46272);
#37315=AXIS2_PLACEMENT_3D('',#66034,#46274,#46275);
#37316=AXIS2_PLACEMENT_3D('',#66071,#46277,#46278);
#37317=AXIS2_PLACEMENT_3D('',#66109,#46280,#46281);
#37318=AXIS2_PLACEMENT_3D('',#66145,#46283,#46284);
#37319=AXIS2_PLACEMENT_3D('',#66183,#46286,#46287);
#37320=AXIS2_PLACEMENT_3D('',#66220,#46289,#46290);
#37321=AXIS2_PLACEMENT_3D('',#66257,#46292,#46293);
#37322=AXIS2_PLACEMENT_3D('',#66295,#46295,#46296);
#37323=AXIS2_PLACEMENT_3D('',#66332,#46298,#46299);
#37324=AXIS2_PLACEMENT_3D('',#66369,#46301,#46302);
#37325=AXIS2_PLACEMENT_3D('',#66407,#46304,#46305);
#37326=AXIS2_PLACEMENT_3D('',#66444,#46307,#46308);
#37327=AXIS2_PLACEMENT_3D('',#66481,#46310,#46311);
#37328=AXIS2_PLACEMENT_3D('',#66518,#46313,#46314);
#37329=AXIS2_PLACEMENT_3D('',#66555,#46316,#46317);
#37330=AXIS2_PLACEMENT_3D('',#66593,#46319,#46320);
#37331=AXIS2_PLACEMENT_3D('',#66630,#46322,#46323);
#37332=AXIS2_PLACEMENT_3D('',#66632,#46324,#46325);
#37333=AXIS2_PLACEMENT_3D('',#66636,#46327,#46328);
#37334=AXIS2_PLACEMENT_3D('',#66637,#46329,#46330);
#37335=AXIS2_PLACEMENT_3D('',#66638,#46331,#46332);
#37336=AXIS2_PLACEMENT_3D('',#66642,#46334,#46335);
#37337=AXIS2_PLACEMENT_3D('',#66644,#46336,#46337);
#37338=AXIS2_PLACEMENT_3D('',#66645,#46338,#46339);
#37339=AXIS2_PLACEMENT_3D('',#66646,#46340,#46341);
#37340=AXIS2_PLACEMENT_3D('',#66647,#46342,#46343);
#37341=AXIS2_PLACEMENT_3D('',#66664,#46348,#46349);
#37342=AXIS2_PLACEMENT_3D('',#66665,#46350,#46351);
#37343=AXIS2_PLACEMENT_3D('',#66667,#46352,#46353);
#37344=AXIS2_PLACEMENT_3D('',#66668,#46354,#46355);
#37345=AXIS2_PLACEMENT_3D('',#66682,#46359,#46360);
#37346=AXIS2_PLACEMENT_3D('',#66684,#46361,#46362);
#37347=AXIS2_PLACEMENT_3D('',#66687,#46364,#46365);
#37348=AXIS2_PLACEMENT_3D('',#66688,#46366,#46367);
#37349=AXIS2_PLACEMENT_3D('',#66694,#46368,#46369);
#37350=AXIS2_PLACEMENT_3D('',#66702,#46370,#46371);
#37351=AXIS2_PLACEMENT_3D('',#66707,#46375,#46376);
#37352=AXIS2_PLACEMENT_3D('',#66709,#46378,#46379);
#37353=AXIS2_PLACEMENT_3D('',#66710,#46380,#46381);
#37354=AXIS2_PLACEMENT_3D('',#66714,#46382,#46383);
#37355=AXIS2_PLACEMENT_3D('',#66715,#46384,#46385);
#37356=AXIS2_PLACEMENT_3D('',#68559,#46386,#46387);
#37357=AXIS2_PLACEMENT_3D('',#68561,#46388,#46389);
#37358=AXIS2_PLACEMENT_3D('',#68562,#46390,#46391);
#37359=AXIS2_PLACEMENT_3D('',#68676,#46392,#46393);
#37360=AXIS2_PLACEMENT_3D('',#68677,#46394,#46395);
#37361=AXIS2_PLACEMENT_3D('',#70182,#46396,#46397);
#37362=AXIS2_PLACEMENT_3D('',#70183,#46398,#46399);
#37363=AXIS2_PLACEMENT_3D('',#70192,#46404,#46405);
#37364=AXIS2_PLACEMENT_3D('',#70194,#46406,#46407);
#37365=AXIS2_PLACEMENT_3D('',#70196,#46409,#46410);
#37366=AXIS2_PLACEMENT_3D('',#70200,#46413,#46414);
#37367=AXIS2_PLACEMENT_3D('',#70201,#46415,#46416);
#37368=AXIS2_PLACEMENT_3D('',#70202,#46417,#46418);
#37369=AXIS2_PLACEMENT_3D('',#70211,#46423,#46424);
#37370=AXIS2_PLACEMENT_3D('',#70213,#46425,#46426);
#37371=AXIS2_PLACEMENT_3D('',#70215,#46428,#46429);
#37372=AXIS2_PLACEMENT_3D('',#70219,#46432,#46433);
#37373=AXIS2_PLACEMENT_3D('',#70220,#46434,#46435);
#37374=AXIS2_PLACEMENT_3D('',#70221,#46436,#46437);
#37375=AXIS2_PLACEMENT_3D('',#70230,#46442,#46443);
#37376=AXIS2_PLACEMENT_3D('',#70232,#46444,#46445);
#37377=AXIS2_PLACEMENT_3D('',#70234,#46447,#46448);
#37378=AXIS2_PLACEMENT_3D('',#70238,#46451,#46452);
#37379=AXIS2_PLACEMENT_3D('',#70239,#46453,#46454);
#37380=AXIS2_PLACEMENT_3D('',#70240,#46455,#46456);
#37381=AXIS2_PLACEMENT_3D('',#70249,#46461,#46462);
#37382=AXIS2_PLACEMENT_3D('',#70251,#46463,#46464);
#37383=AXIS2_PLACEMENT_3D('',#70253,#46466,#46467);
#37384=AXIS2_PLACEMENT_3D('',#70257,#46470,#46471);
#37385=AXIS2_PLACEMENT_3D('',#70258,#46472,#46473);
#37386=AXIS2_PLACEMENT_3D('',#70259,#46474,#46475);
#37387=AXIS2_PLACEMENT_3D('',#70268,#46480,#46481);
#37388=AXIS2_PLACEMENT_3D('',#70270,#46482,#46483);
#37389=AXIS2_PLACEMENT_3D('',#70272,#46485,#46486);
#37390=AXIS2_PLACEMENT_3D('',#70276,#46489,#46490);
#37391=AXIS2_PLACEMENT_3D('',#70277,#46491,#46492);
#37392=AXIS2_PLACEMENT_3D('',#70278,#46493,#46494);
#37393=AXIS2_PLACEMENT_3D('',#70287,#46499,#46500);
#37394=AXIS2_PLACEMENT_3D('',#70289,#46501,#46502);
#37395=AXIS2_PLACEMENT_3D('',#70291,#46504,#46505);
#37396=AXIS2_PLACEMENT_3D('',#70295,#46508,#46509);
#37397=AXIS2_PLACEMENT_3D('',#70296,#46510,#46511);
#37398=AXIS2_PLACEMENT_3D('',#70297,#46512,#46513);
#37399=AXIS2_PLACEMENT_3D('',#70306,#46518,#46519);
#37400=AXIS2_PLACEMENT_3D('',#70308,#46520,#46521);
#37401=AXIS2_PLACEMENT_3D('',#70310,#46523,#46524);
#37402=AXIS2_PLACEMENT_3D('',#70314,#46527,#46528);
#37403=AXIS2_PLACEMENT_3D('',#70315,#46529,#46530);
#37404=AXIS2_PLACEMENT_3D('',#70316,#46531,#46532);
#37405=AXIS2_PLACEMENT_3D('',#70325,#46537,#46538);
#37406=AXIS2_PLACEMENT_3D('',#70327,#46539,#46540);
#37407=AXIS2_PLACEMENT_3D('',#70329,#46542,#46543);
#37408=AXIS2_PLACEMENT_3D('',#70333,#46546,#46547);
#37409=AXIS2_PLACEMENT_3D('',#70334,#46548,#46549);
#37410=AXIS2_PLACEMENT_3D('',#70335,#46550,#46551);
#37411=AXIS2_PLACEMENT_3D('',#70344,#46556,#46557);
#37412=AXIS2_PLACEMENT_3D('',#70346,#46558,#46559);
#37413=AXIS2_PLACEMENT_3D('',#70348,#46561,#46562);
#37414=AXIS2_PLACEMENT_3D('',#70352,#46565,#46566);
#37415=AXIS2_PLACEMENT_3D('',#70353,#46567,#46568);
#37416=AXIS2_PLACEMENT_3D('',#70354,#46569,#46570);
#37417=AXIS2_PLACEMENT_3D('',#70363,#46575,#46576);
#37418=AXIS2_PLACEMENT_3D('',#70365,#46577,#46578);
#37419=AXIS2_PLACEMENT_3D('',#70367,#46580,#46581);
#37420=AXIS2_PLACEMENT_3D('',#70371,#46584,#46585);
#37421=AXIS2_PLACEMENT_3D('',#70372,#46586,#46587);
#37422=AXIS2_PLACEMENT_3D('',#70373,#46588,#46589);
#37423=AXIS2_PLACEMENT_3D('',#70382,#46594,#46595);
#37424=AXIS2_PLACEMENT_3D('',#70384,#46596,#46597);
#37425=AXIS2_PLACEMENT_3D('',#70386,#46599,#46600);
#37426=AXIS2_PLACEMENT_3D('',#70390,#46603,#46604);
#37427=AXIS2_PLACEMENT_3D('',#70391,#46605,#46606);
#37428=AXIS2_PLACEMENT_3D('',#70392,#46607,#46608);
#37429=AXIS2_PLACEMENT_3D('',#70401,#46613,#46614);
#37430=AXIS2_PLACEMENT_3D('',#70403,#46615,#46616);
#37431=AXIS2_PLACEMENT_3D('',#70405,#46618,#46619);
#37432=AXIS2_PLACEMENT_3D('',#70409,#46622,#46623);
#37433=AXIS2_PLACEMENT_3D('',#70410,#46624,#46625);
#37434=AXIS2_PLACEMENT_3D('',#70411,#46626,#46627);
#37435=AXIS2_PLACEMENT_3D('',#70420,#46632,#46633);
#37436=AXIS2_PLACEMENT_3D('',#70422,#46634,#46635);
#37437=AXIS2_PLACEMENT_3D('',#70424,#46637,#46638);
#37438=AXIS2_PLACEMENT_3D('',#70428,#46641,#46642);
#37439=AXIS2_PLACEMENT_3D('',#70429,#46643,#46644);
#37440=AXIS2_PLACEMENT_3D('',#70430,#46645,#46646);
#37441=AXIS2_PLACEMENT_3D('',#70439,#46651,#46652);
#37442=AXIS2_PLACEMENT_3D('',#70441,#46653,#46654);
#37443=AXIS2_PLACEMENT_3D('',#70443,#46656,#46657);
#37444=AXIS2_PLACEMENT_3D('',#70447,#46660,#46661);
#37445=AXIS2_PLACEMENT_3D('',#70448,#46662,#46663);
#37446=AXIS2_PLACEMENT_3D('',#70449,#46664,#46665);
#37447=AXIS2_PLACEMENT_3D('',#70458,#46670,#46671);
#37448=AXIS2_PLACEMENT_3D('',#70460,#46672,#46673);
#37449=AXIS2_PLACEMENT_3D('',#70462,#46675,#46676);
#37450=AXIS2_PLACEMENT_3D('',#70466,#46679,#46680);
#37451=AXIS2_PLACEMENT_3D('',#70467,#46681,#46682);
#37452=AXIS2_PLACEMENT_3D('',#70468,#46683,#46684);
#37453=AXIS2_PLACEMENT_3D('',#70477,#46689,#46690);
#37454=AXIS2_PLACEMENT_3D('',#70479,#46691,#46692);
#37455=AXIS2_PLACEMENT_3D('',#70481,#46694,#46695);
#37456=AXIS2_PLACEMENT_3D('',#70485,#46698,#46699);
#37457=AXIS2_PLACEMENT_3D('',#70486,#46700,#46701);
#37458=AXIS2_PLACEMENT_3D('',#70487,#46702,#46703);
#37459=AXIS2_PLACEMENT_3D('',#70496,#46708,#46709);
#37460=AXIS2_PLACEMENT_3D('',#70498,#46710,#46711);
#37461=AXIS2_PLACEMENT_3D('',#70500,#46713,#46714);
#37462=AXIS2_PLACEMENT_3D('',#70504,#46717,#46718);
#37463=AXIS2_PLACEMENT_3D('',#70505,#46719,#46720);
#37464=AXIS2_PLACEMENT_3D('',#70506,#46721,#46722);
#37465=AXIS2_PLACEMENT_3D('',#70515,#46727,#46728);
#37466=AXIS2_PLACEMENT_3D('',#70517,#46729,#46730);
#37467=AXIS2_PLACEMENT_3D('',#70520,#46732,#46733);
#37468=AXIS2_PLACEMENT_3D('',#70521,#46734,#46735);
#37469=AXIS2_PLACEMENT_3D('',#70525,#46738,#46739);
#37470=AXIS2_PLACEMENT_3D('',#70527,#46740,#46741);
#37471=AXIS2_PLACEMENT_3D('',#70528,#46742,#46743);
#37472=AXIS2_PLACEMENT_3D('',#70529,#46744,#46745);
#37473=AXIS2_PLACEMENT_3D('',#70538,#46750,#46751);
#37474=AXIS2_PLACEMENT_3D('',#70540,#46752,#46753);
#37475=AXIS2_PLACEMENT_3D('',#70542,#46755,#46756);
#37476=AXIS2_PLACEMENT_3D('',#70546,#46759,#46760);
#37477=AXIS2_PLACEMENT_3D('',#70547,#46761,#46762);
#37478=AXIS2_PLACEMENT_3D('',#70548,#46763,#46764);
#37479=AXIS2_PLACEMENT_3D('',#70557,#46769,#46770);
#37480=AXIS2_PLACEMENT_3D('',#70559,#46771,#46772);
#37481=AXIS2_PLACEMENT_3D('',#70561,#46774,#46775);
#37482=AXIS2_PLACEMENT_3D('',#70565,#46778,#46779);
#37483=AXIS2_PLACEMENT_3D('',#70566,#46780,#46781);
#37484=AXIS2_PLACEMENT_3D('',#70567,#46782,#46783);
#37485=AXIS2_PLACEMENT_3D('',#70576,#46788,#46789);
#37486=AXIS2_PLACEMENT_3D('',#70578,#46790,#46791);
#37487=AXIS2_PLACEMENT_3D('',#70580,#46793,#46794);
#37488=AXIS2_PLACEMENT_3D('',#70584,#46797,#46798);
#37489=AXIS2_PLACEMENT_3D('',#70585,#46799,#46800);
#37490=AXIS2_PLACEMENT_3D('',#70586,#46801,#46802);
#37491=AXIS2_PLACEMENT_3D('',#70595,#46807,#46808);
#37492=AXIS2_PLACEMENT_3D('',#70597,#46809,#46810);
#37493=AXIS2_PLACEMENT_3D('',#70599,#46812,#46813);
#37494=AXIS2_PLACEMENT_3D('',#70603,#46816,#46817);
#37495=AXIS2_PLACEMENT_3D('',#70604,#46818,#46819);
#37496=AXIS2_PLACEMENT_3D('',#70605,#46820,#46821);
#37497=AXIS2_PLACEMENT_3D('',#70614,#46826,#46827);
#37498=AXIS2_PLACEMENT_3D('',#70616,#46828,#46829);
#37499=AXIS2_PLACEMENT_3D('',#70618,#46831,#46832);
#37500=AXIS2_PLACEMENT_3D('',#70622,#46835,#46836);
#37501=AXIS2_PLACEMENT_3D('',#70623,#46837,#46838);
#37502=AXIS2_PLACEMENT_3D('',#70624,#46839,#46840);
#37503=AXIS2_PLACEMENT_3D('',#70633,#46845,#46846);
#37504=AXIS2_PLACEMENT_3D('',#70635,#46847,#46848);
#37505=AXIS2_PLACEMENT_3D('',#70637,#46850,#46851);
#37506=AXIS2_PLACEMENT_3D('',#70641,#46854,#46855);
#37507=AXIS2_PLACEMENT_3D('',#70642,#46856,#46857);
#37508=AXIS2_PLACEMENT_3D('',#70643,#46858,#46859);
#37509=AXIS2_PLACEMENT_3D('',#70652,#46864,#46865);
#37510=AXIS2_PLACEMENT_3D('',#70654,#46866,#46867);
#37511=AXIS2_PLACEMENT_3D('',#70656,#46869,#46870);
#37512=AXIS2_PLACEMENT_3D('',#70660,#46873,#46874);
#37513=AXIS2_PLACEMENT_3D('',#70661,#46875,#46876);
#37514=AXIS2_PLACEMENT_3D('',#70662,#46877,#46878);
#37515=AXIS2_PLACEMENT_3D('',#70671,#46883,#46884);
#37516=AXIS2_PLACEMENT_3D('',#70673,#46885,#46886);
#37517=AXIS2_PLACEMENT_3D('',#70675,#46888,#46889);
#37518=AXIS2_PLACEMENT_3D('',#70679,#46892,#46893);
#37519=AXIS2_PLACEMENT_3D('',#70680,#46894,#46895);
#37520=AXIS2_PLACEMENT_3D('',#70681,#46896,#46897);
#37521=AXIS2_PLACEMENT_3D('',#70690,#46902,#46903);
#37522=AXIS2_PLACEMENT_3D('',#70692,#46904,#46905);
#37523=AXIS2_PLACEMENT_3D('',#70694,#46907,#46908);
#37524=AXIS2_PLACEMENT_3D('',#70698,#46911,#46912);
#37525=AXIS2_PLACEMENT_3D('',#70699,#46913,#46914);
#37526=AXIS2_PLACEMENT_3D('',#70700,#46915,#46916);
#37527=AXIS2_PLACEMENT_3D('',#70709,#46921,#46922);
#37528=AXIS2_PLACEMENT_3D('',#70711,#46923,#46924);
#37529=AXIS2_PLACEMENT_3D('',#70713,#46926,#46927);
#37530=AXIS2_PLACEMENT_3D('',#70717,#46930,#46931);
#37531=AXIS2_PLACEMENT_3D('',#70718,#46932,#46933);
#37532=AXIS2_PLACEMENT_3D('',#70719,#46934,#46935);
#37533=AXIS2_PLACEMENT_3D('',#70728,#46940,#46941);
#37534=AXIS2_PLACEMENT_3D('',#70730,#46942,#46943);
#37535=AXIS2_PLACEMENT_3D('',#70732,#46945,#46946);
#37536=AXIS2_PLACEMENT_3D('',#70736,#46949,#46950);
#37537=AXIS2_PLACEMENT_3D('',#70737,#46951,#46952);
#37538=AXIS2_PLACEMENT_3D('',#70738,#46953,#46954);
#37539=AXIS2_PLACEMENT_3D('',#70747,#46959,#46960);
#37540=AXIS2_PLACEMENT_3D('',#70749,#46961,#46962);
#37541=AXIS2_PLACEMENT_3D('',#70751,#46964,#46965);
#37542=AXIS2_PLACEMENT_3D('',#70755,#46968,#46969);
#37543=AXIS2_PLACEMENT_3D('',#70756,#46970,#46971);
#37544=AXIS2_PLACEMENT_3D('',#70757,#46972,#46973);
#37545=AXIS2_PLACEMENT_3D('',#70766,#46978,#46979);
#37546=AXIS2_PLACEMENT_3D('',#70768,#46980,#46981);
#37547=AXIS2_PLACEMENT_3D('',#70770,#46983,#46984);
#37548=AXIS2_PLACEMENT_3D('',#70774,#46987,#46988);
#37549=AXIS2_PLACEMENT_3D('',#70775,#46989,#46990);
#37550=AXIS2_PLACEMENT_3D('',#70776,#46991,#46992);
#37551=AXIS2_PLACEMENT_3D('',#70785,#46997,#46998);
#37552=AXIS2_PLACEMENT_3D('',#70787,#46999,#47000);
#37553=AXIS2_PLACEMENT_3D('',#70789,#47002,#47003);
#37554=AXIS2_PLACEMENT_3D('',#70793,#47006,#47007);
#37555=AXIS2_PLACEMENT_3D('',#70794,#47008,#47009);
#37556=AXIS2_PLACEMENT_3D('',#70795,#47010,#47011);
#37557=AXIS2_PLACEMENT_3D('',#70804,#47016,#47017);
#37558=AXIS2_PLACEMENT_3D('',#70806,#47018,#47019);
#37559=AXIS2_PLACEMENT_3D('',#70808,#47021,#47022);
#37560=AXIS2_PLACEMENT_3D('',#70812,#47025,#47026);
#37561=AXIS2_PLACEMENT_3D('',#70813,#47027,#47028);
#37562=AXIS2_PLACEMENT_3D('',#70814,#47029,#47030);
#37563=AXIS2_PLACEMENT_3D('',#70823,#47035,#47036);
#37564=AXIS2_PLACEMENT_3D('',#70825,#47037,#47038);
#37565=AXIS2_PLACEMENT_3D('',#70827,#47040,#47041);
#37566=AXIS2_PLACEMENT_3D('',#70831,#47044,#47045);
#37567=AXIS2_PLACEMENT_3D('',#70832,#47046,#47047);
#37568=AXIS2_PLACEMENT_3D('',#70833,#47048,#47049);
#37569=AXIS2_PLACEMENT_3D('',#70842,#47054,#47055);
#37570=AXIS2_PLACEMENT_3D('',#70844,#47056,#47057);
#37571=AXIS2_PLACEMENT_3D('',#70846,#47059,#47060);
#37572=AXIS2_PLACEMENT_3D('',#70850,#47063,#47064);
#37573=AXIS2_PLACEMENT_3D('',#70851,#47065,#47066);
#37574=AXIS2_PLACEMENT_3D('',#70852,#47067,#47068);
#37575=AXIS2_PLACEMENT_3D('',#70861,#47073,#47074);
#37576=AXIS2_PLACEMENT_3D('',#70863,#47075,#47076);
#37577=AXIS2_PLACEMENT_3D('',#70865,#47078,#47079);
#37578=AXIS2_PLACEMENT_3D('',#70869,#47082,#47083);
#37579=AXIS2_PLACEMENT_3D('',#70870,#47084,#47085);
#37580=AXIS2_PLACEMENT_3D('',#70871,#47086,#47087);
#37581=AXIS2_PLACEMENT_3D('',#70873,#47088,#47089);
#37582=AXIS2_PLACEMENT_3D('',#70876,#47092,#47093);
#37583=AXIS2_PLACEMENT_3D('',#70878,#47095,#47096);
#37584=AXIS2_PLACEMENT_3D('',#70879,#47097,#47098);
#37585=AXIS2_PLACEMENT_3D('',#70881,#47099,#47100);
#37586=AXIS2_PLACEMENT_3D('',#70905,#47102,#47103);
#37587=AXIS2_PLACEMENT_3D('',#70945,#47104,#47105);
#37588=AXIS2_PLACEMENT_3D('',#70991,#47106,#47107);
#37589=AXIS2_PLACEMENT_3D('',#71031,#47108,#47109);
#37590=AXIS2_PLACEMENT_3D('',#71071,#47110,#47111);
#37591=AXIS2_PLACEMENT_3D('',#71117,#47112,#47113);
#37592=AXIS2_PLACEMENT_3D('',#71244,#47114,#47115);
#37593=AXIS2_PLACEMENT_3D('',#71245,#47116,#47117);
#37594=AXIS2_PLACEMENT_3D('',#71250,#47118,#47119);
#37595=AXIS2_PLACEMENT_3D('',#71260,#47120,#47121);
#37596=AXIS2_PLACEMENT_3D('',#71270,#47122,#47123);
#37597=AXIS2_PLACEMENT_3D('',#71280,#47124,#47125);
#37598=AXIS2_PLACEMENT_3D('',#71329,#47126,#47127);
#37599=AXIS2_PLACEMENT_3D('',#71331,#47128,#47129);
#37600=AXIS2_PLACEMENT_3D('',#71332,#47130,#47131);
#37601=AXIS2_PLACEMENT_3D('',#71339,#47135,#47136);
#37602=AXIS2_PLACEMENT_3D('',#71346,#47140,#47141);
#37603=AXIS2_PLACEMENT_3D('',#71353,#47145,#47146);
#37604=AXIS2_PLACEMENT_3D('',#71356,#47149,#47150);
#37605=AXIS2_PLACEMENT_3D('',#71358,#47152,#47153);
#37606=AXIS2_PLACEMENT_3D('',#71365,#47157,#47158);
#37607=AXIS2_PLACEMENT_3D('',#71374,#47160,#47161);
#37608=AXIS2_PLACEMENT_3D('',#71381,#47165,#47166);
#37609=AXIS2_PLACEMENT_3D('',#71384,#47169,#47170);
#37610=AXIS2_PLACEMENT_3D('',#71386,#47172,#47173);
#37611=AXIS2_PLACEMENT_3D('',#71393,#47177,#47178);
#37612=AXIS2_PLACEMENT_3D('',#71396,#47181,#47182);
#37613=AXIS2_PLACEMENT_3D('',#71412,#47184,#47185);
#37614=AXIS2_PLACEMENT_3D('',#71421,#47187,#47188);
#37615=AXIS2_PLACEMENT_3D('',#71467,#47190,#47191);
#37616=AXIS2_PLACEMENT_3D('',#71500,#47194,#47195);
#37617=AXIS2_PLACEMENT_3D('',#71503,#47198,#47199);
#37618=AXIS2_PLACEMENT_3D('',#71536,#47202,#47203);
#37619=AXIS2_PLACEMENT_3D('',#71539,#47206,#47207);
#37620=AXIS2_PLACEMENT_3D('',#71542,#47210,#47211);
#37621=AXIS2_PLACEMENT_3D('',#71545,#47214,#47215);
#37622=AXIS2_PLACEMENT_3D('',#71548,#47218,#47219);
#37623=AXIS2_PLACEMENT_3D('',#71551,#47222,#47223);
#37624=AXIS2_PLACEMENT_3D('',#71554,#47226,#47227);
#37625=AXIS2_PLACEMENT_3D('',#71555,#47228,#47229);
#37626=AXIS2_PLACEMENT_3D('',#71557,#47230,#47231);
#37627=AXIS2_PLACEMENT_3D('',#71558,#47232,#47233);
#37628=AXIS2_PLACEMENT_3D('',#71559,#47234,#47235);
#37629=AXIS2_PLACEMENT_3D('',#71560,#47236,#47237);
#37630=AXIS2_PLACEMENT_3D('',#71561,#47238,#47239);
#37631=AXIS2_PLACEMENT_3D('',#71562,#47240,#47241);
#37632=AXIS2_PLACEMENT_3D('',#71563,#47242,#47243);
#37633=AXIS2_PLACEMENT_3D('',#71566,#47244,#47245);
#37634=AXIS2_PLACEMENT_3D('',#71568,#47247,#47248);
#37635=AXIS2_PLACEMENT_3D('',#71569,#47249,#47250);
#37636=AXIS2_PLACEMENT_3D('',#71572,#47252,#47253);
#37637=AXIS2_PLACEMENT_3D('',#71573,#47254,#47255);
#37638=AXIS2_PLACEMENT_3D('',#71575,#47256,#47257);
#37639=AXIS2_PLACEMENT_3D('',#71576,#47258,#47259);
#37640=AXIS2_PLACEMENT_3D('',#71578,#47261,#47262);
#37641=AXIS2_PLACEMENT_3D('',#71579,#47263,#47264);
#37642=AXIS2_PLACEMENT_3D('',#71580,#47265,#47266);
#37643=AXIS2_PLACEMENT_3D('',#71581,#47267,#47268);
#37644=AXIS2_PLACEMENT_3D('',#71582,#47269,#47270);
#37645=AXIS2_PLACEMENT_3D('',#71583,#47271,#47272);
#37646=AXIS2_PLACEMENT_3D('',#71584,#47273,#47274);
#37647=AXIS2_PLACEMENT_3D('',#71585,#47275,#47276);
#37648=AXIS2_PLACEMENT_3D('',#71586,#47277,#47278);
#37649=AXIS2_PLACEMENT_3D('',#71587,#47279,#47280);
#37650=AXIS2_PLACEMENT_3D('',#71588,#47281,#47282);
#37651=AXIS2_PLACEMENT_3D('',#71589,#47283,#47284);
#37652=AXIS2_PLACEMENT_3D('',#71590,#47285,#47286);
#37653=AXIS2_PLACEMENT_3D('',#71591,#47287,#47288);
#37654=AXIS2_PLACEMENT_3D('',#71592,#47289,#47290);
#37655=AXIS2_PLACEMENT_3D('',#71593,#47291,#47292);
#37656=AXIS2_PLACEMENT_3D('',#71594,#47293,#47294);
#37657=AXIS2_PLACEMENT_3D('',#71595,#47295,#47296);
#37658=AXIS2_PLACEMENT_3D('',#71596,#47297,#47298);
#37659=AXIS2_PLACEMENT_3D('',#71597,#47299,#47300);
#37660=AXIS2_PLACEMENT_3D('',#71598,#47301,#47302);
#37661=DIRECTION('axis',(0.,0.,1.));
#37662=DIRECTION('refdir',(1.,0.,0.));
#37663=DIRECTION('axis',(0.,0.,1.));
#37664=DIRECTION('refdir',(1.,0.,0.));
#37665=DIRECTION('center_axis',(1.,0.,3.3469968371114E-15));
#37666=DIRECTION('ref_axis',(0.,-1.,-3.0444058251673E-17));
#37667=DIRECTION('center_axis',(-1.,0.,0.));
#37668=DIRECTION('ref_axis',(0.,-1.,0.));
#37669=DIRECTION('center_axis',(-1.,0.,0.));
#37670=DIRECTION('ref_axis',(0.,-1.,0.));
#37671=DIRECTION('',(-0.85065080835204,-0.525731112119134,-2.92751444600949E-15));
#37672=DIRECTION('center_axis',(1.,0.,0.));
#37673=DIRECTION('ref_axis',(0.,-1.,-6.12323399573677E-17));
#37674=DIRECTION('center_axis',(1.,0.,0.));
#37675=DIRECTION('ref_axis',(0.,-1.,-6.12323399573677E-17));
#37676=DIRECTION('center_axis',(1.,0.,0.));
#37677=DIRECTION('ref_axis',(0.,1.,0.));
#37678=DIRECTION('',(-0.447213595499958,0.894427190999916,1.09535739652841E-16));
#37679=DIRECTION('center_axis',(-1.,0.,0.));
#37680=DIRECTION('ref_axis',(0.,-1.,-6.12323399573676E-17));
#37681=DIRECTION('center_axis',(-1.,0.,0.));
#37682=DIRECTION('ref_axis',(0.,-1.,-6.12323399573676E-17));
#37683=DIRECTION('center_axis',(1.,0.,0.));
#37684=DIRECTION('ref_axis',(0.,1.,0.));
#37685=DIRECTION('center_axis',(1.,0.,0.));
#37686=DIRECTION('ref_axis',(0.,0.,-1.));
#37687=DIRECTION('',(-1.,0.,0.));
#37688=DIRECTION('center_axis',(1.,0.,-1.02545205978024E-14));
#37689=DIRECTION('ref_axis',(0.,-1.,-3.10083423275242E-17));
#37690=DIRECTION('',(-0.229752920547362,-0.97324898946773,2.20663859235035E-15));
#37691=DIRECTION('center_axis',(1.,0.,0.));
#37692=DIRECTION('ref_axis',(0.,-1.,0.));
#37693=DIRECTION('center_axis',(-1.,0.,0.));
#37694=DIRECTION('ref_axis',(0.,0.,1.));
#37695=DIRECTION('center_axis',(1.,0.,0.));
#37696=DIRECTION('ref_axis',(0.,0.,-1.));
#37697=DIRECTION('center_axis',(-1.,0.,0.));
#37698=DIRECTION('ref_axis',(0.,-1.,0.));
#37699=DIRECTION('center_axis',(-1.,0.,0.));
#37700=DIRECTION('ref_axis',(0.,-1.,0.));
#37701=DIRECTION('',(0.707106781186548,-0.707106781186548,8.65956056235493E-17));
#37702=DIRECTION('center_axis',(1.,0.,0.));
#37703=DIRECTION('ref_axis',(0.,-1.,0.));
#37704=DIRECTION('center_axis',(1.,0.,0.));
#37705=DIRECTION('ref_axis',(0.,-1.,0.));
#37706=DIRECTION('center_axis',(1.,0.,0.));
#37707=DIRECTION('ref_axis',(0.,1.,0.));
#37708=DIRECTION('center_axis',(1.,0.,0.));
#37709=DIRECTION('ref_axis',(0.,0.,-1.));
#37710=DIRECTION('',(-1.,0.,0.));
#37711=DIRECTION('center_axis',(-1.,0.,0.));
#37712=DIRECTION('ref_axis',(0.,0.,1.));
#37713=DIRECTION('center_axis',(1.,0.,0.));
#37714=DIRECTION('ref_axis',(0.,0.,-1.));
#37715=DIRECTION('center_axis',(-1.,0.,-5.60335109986454E-15));
#37716=DIRECTION('ref_axis',(0.,-1.,-3.10254273231018E-17));
#37717=DIRECTION('center_axis',(-1.,0.,0.));
#37718=DIRECTION('ref_axis',(0.,-1.,0.));
#37719=DIRECTION('',(-0.38268343236509,0.923879532511287,-2.00250326312286E-15));
#37720=DIRECTION('center_axis',(1.,0.,0.));
#37721=DIRECTION('ref_axis',(0.,-1.,-6.12323399573677E-17));
#37722=DIRECTION('center_axis',(1.,0.,0.));
#37723=DIRECTION('ref_axis',(0.,-1.,-6.12323399573677E-17));
#37724=DIRECTION('center_axis',(-1.,0.,0.));
#37725=DIRECTION('ref_axis',(0.,1.,0.));
#37726=DIRECTION('',(-0.707106781186547,-0.707106781186548,-8.65956056235494E-17));
#37727=DIRECTION('center_axis',(-1.,0.,0.));
#37728=DIRECTION('ref_axis',(0.,-1.,-6.12323399573677E-17));
#37729=DIRECTION('center_axis',(-1.,0.,0.));
#37730=DIRECTION('ref_axis',(0.,-1.,-6.12323399573677E-17));
#37731=DIRECTION('center_axis',(1.,0.,0.));
#37732=DIRECTION('ref_axis',(0.,0.,-1.));
#37733=DIRECTION('center_axis',(1.,0.,0.));
#37734=DIRECTION('ref_axis',(0.,0.,-1.));
#37735=DIRECTION('center_axis',(-1.,0.,-2.93398870229358E-17));
#37736=DIRECTION('ref_axis',(0.,-1.,-6.12323399573676E-17));
#37737=DIRECTION('',(-0.901819525133682,0.43211288350113,5.29185659649989E-17));
#37738=DIRECTION('center_axis',(1.,0.,0.));
#37739=DIRECTION('ref_axis',(0.,-1.,-6.12323399573677E-17));
#37740=DIRECTION('center_axis',(1.,0.,0.));
#37741=DIRECTION('ref_axis',(0.,-1.,-6.12323399573677E-17));
#37742=DIRECTION('center_axis',(-1.,0.,0.));
#37743=DIRECTION('ref_axis',(0.,1.,0.));
#37744=DIRECTION('',(-0.994144463069456,-0.108059180768419,-1.3233432984653E-17));
#37745=DIRECTION('center_axis',(1.,0.,0.));
#37746=DIRECTION('ref_axis',(0.,0.,-1.));
#37747=DIRECTION('center_axis',(-1.,0.,-1.54843166437498E-16));
#37748=DIRECTION('ref_axis',(0.,-1.,-6.12323399573677E-17));
#37749=DIRECTION('center_axis',(-1.,0.,0.));
#37750=DIRECTION('ref_axis',(0.,-1.,-6.12323399573677E-17));
#37751=DIRECTION('center_axis',(-1.,0.,0.));
#37752=DIRECTION('ref_axis',(0.,-1.,-6.12323399573677E-17));
#37753=DIRECTION('',(-0.367738219294597,0.929929353268322,1.1388350059132E-16));
#37754=DIRECTION('center_axis',(1.,0.,0.));
#37755=DIRECTION('ref_axis',(0.,-1.,-6.12323399573677E-17));
#37756=DIRECTION('center_axis',(1.,0.,0.));
#37757=DIRECTION('ref_axis',(0.,-1.,-6.12323399573677E-17));
#37758=DIRECTION('center_axis',(-1.,0.,0.));
#37759=DIRECTION('ref_axis',(0.,1.,0.));
#37760=DIRECTION('',(-0.554700196225228,-0.832050294337845,-1.01896772969045E-16));
#37761=DIRECTION('center_axis',(-1.,0.,0.));
#37762=DIRECTION('ref_axis',(0.,-1.,-6.12323399573677E-17));
#37763=DIRECTION('center_axis',(-1.,0.,0.));
#37764=DIRECTION('ref_axis',(0.,-1.,-6.12323399573677E-17));
#37765=DIRECTION('center_axis',(-1.,0.,0.));
#37766=DIRECTION('ref_axis',(0.,1.,0.));
#37767=DIRECTION('center_axis',(1.,0.,0.));
#37768=DIRECTION('ref_axis',(0.,0.,-1.));
#37769=DIRECTION('',(-0.164398987305358,-0.986393923832144,-1.20798416151943E-16));
#37770=DIRECTION('center_axis',(-1.,0.,-6.47285581734468E-17));
#37771=DIRECTION('ref_axis',(0.,-1.,-6.12323399573677E-17));
#37772=DIRECTION('',(-0.687215388498205,0.726453721727173,8.89649225041859E-17));
#37773=DIRECTION('center_axis',(1.,0.,0.));
#37774=DIRECTION('ref_axis',(0.,-1.,-6.12323399573677E-17));
#37775=DIRECTION('center_axis',(1.,0.,0.));
#37776=DIRECTION('ref_axis',(0.,-1.,-6.12323399573677E-17));
#37777=DIRECTION('center_axis',(-1.,0.,0.));
#37778=DIRECTION('ref_axis',(0.,1.,0.));
#37779=DIRECTION('',(-0.800000000000001,-0.599999999999999,-7.34788079488411E-17));
#37780=DIRECTION('center_axis',(-1.,0.,0.));
#37781=DIRECTION('ref_axis',(0.,-1.,-6.12323399573677E-17));
#37782=DIRECTION('center_axis',(-1.,0.,0.));
#37783=DIRECTION('ref_axis',(0.,-1.,-6.12323399573677E-17));
#37784=DIRECTION('center_axis',(-1.,0.,-3.35417469620003E-17));
#37785=DIRECTION('ref_axis',(0.,-1.,-6.12323399573677E-17));
#37786=DIRECTION('',(-0.877037421408632,0.480422065947118,5.8834734530191E-17));
#37787=DIRECTION('center_axis',(1.,0.,0.));
#37788=DIRECTION('ref_axis',(0.,-1.,-6.12323399573677E-17));
#37789=DIRECTION('center_axis',(1.,0.,0.));
#37790=DIRECTION('ref_axis',(0.,-1.,-6.12323399573677E-17));
#37791=DIRECTION('center_axis',(-1.,0.,0.));
#37792=DIRECTION('ref_axis',(0.,1.,0.));
#37793=DIRECTION('',(-0.936329177569044,-0.351123441588392,-4.30002198846827E-17));
#37794=DIRECTION('center_axis',(-1.,0.,0.));
#37795=DIRECTION('ref_axis',(0.,-1.,-6.12323399573676E-17));
#37796=DIRECTION('center_axis',(-1.,0.,0.));
#37797=DIRECTION('ref_axis',(0.,-1.,-6.12323399573676E-17));
#37798=DIRECTION('center_axis',(-1.,0.,8.59032469848147E-15));
#37799=DIRECTION('ref_axis',(0.,-1.,-3.0596396085212E-17));
#37800=DIRECTION('',(-0.983953550115309,0.17842480549374,8.47979037642802E-15));
#37801=DIRECTION('center_axis',(1.,0.,0.));
#37802=DIRECTION('ref_axis',(0.,-1.,0.));
#37803=DIRECTION('center_axis',(1.,0.,0.));
#37804=DIRECTION('ref_axis',(0.,-1.,0.));
#37805=DIRECTION('center_axis',(1.,0.,0.));
#37806=DIRECTION('ref_axis',(0.,1.,0.));
#37807=DIRECTION('',(-1.,0.,0.));
#37808=DIRECTION('center_axis',(1.,0.,0.));
#37809=DIRECTION('ref_axis',(0.,1.,0.));
#37810=DIRECTION('center_axis',(0.707106781186548,-0.070359754473029,-0.703597544730291));
#37811=DIRECTION('ref_axis',(0.707106781186547,0.0703597544730292,0.703597544730293));
#37812=DIRECTION('',(-1.,0.,0.));
#37813=DIRECTION('center_axis',(-0.707106781186548,-0.0703597544730291,
-0.703597544730292));
#37814=DIRECTION('ref_axis',(-0.707106781186547,0.0703597544730291,0.703597544730292));
#37815=DIRECTION('center_axis',(-1.,0.,0.));
#37816=DIRECTION('ref_axis',(0.,1.,0.));
#37817=DIRECTION('',(-1.,0.,0.));
#37818=DIRECTION('center_axis',(1.,0.,0.));
#37819=DIRECTION('ref_axis',(0.,0.,-1.));
#37820=DIRECTION('center_axis',(-1.,0.,0.));
#37821=DIRECTION('ref_axis',(0.,1.,0.));
#37822=DIRECTION('center_axis',(-0.707106781186547,-0.0703597544730291,
0.703597544730292));
#37823=DIRECTION('ref_axis',(-0.707106781186548,0.0703597544730291,-0.703597544730291));
#37824=DIRECTION('',(1.,0.,0.));
#37825=DIRECTION('center_axis',(0.707106781186548,-0.070359754473029,0.703597544730291));
#37826=DIRECTION('ref_axis',(0.707106781186547,0.0703597544730292,-0.703597544730293));
#37827=DIRECTION('center_axis',(1.,0.,0.));
#37828=DIRECTION('ref_axis',(0.,1.,0.));
#37829=DIRECTION('',(-1.,0.,0.));
#37830=DIRECTION('center_axis',(-0.707106781186548,-0.703597544730292,0.0703597544730291));
#37831=DIRECTION('ref_axis',(-0.707106781186547,0.703597544730292,-0.0703597544730291));
#37832=DIRECTION('center_axis',(-1.,0.,0.));
#37833=DIRECTION('ref_axis',(0.,1.,0.));
#37834=DIRECTION('center_axis',(-0.707106781186547,0.703597544730292,0.0703597544730291));
#37835=DIRECTION('ref_axis',(0.707106781186548,0.703597544730291,0.070359754473029));
#37836=DIRECTION('',(1.,0.,0.));
#37837=DIRECTION('center_axis',(0.707106781186548,0.703597544730291,0.070359754473029));
#37838=DIRECTION('ref_axis',(-0.707106781186547,0.703597544730293,0.0703597544730292));
#37839=DIRECTION('center_axis',(1.,0.,0.));
#37840=DIRECTION('ref_axis',(0.,1.,0.));
#37841=DIRECTION('center_axis',(0.707106781186548,-0.703597544730291,0.070359754473029));
#37842=DIRECTION('ref_axis',(0.707106781186547,0.703597544730293,-0.0703597544730292));
#37843=DIRECTION('',(-1.,0.,0.));
#37844=DIRECTION('center_axis',(-0.707106781186548,-0.707052400311326,0.00876944775867132));
#37845=DIRECTION('ref_axis',(-0.707106781186547,0.707052400311326,-0.00876944775867133));
#37846=DIRECTION('center_axis',(-1.,0.,0.));
#37847=DIRECTION('ref_axis',(0.,1.,0.));
#37848=DIRECTION('center_axis',(-0.707106781186548,0.694787886990046,0.131414580971466));
#37849=DIRECTION('ref_axis',(0.707106781186547,0.694787886990047,0.131414580971466));
#37850=DIRECTION('',(1.,0.,0.));
#37851=DIRECTION('center_axis',(0.707106781186549,0.694787886990045,0.131414580971465));
#37852=DIRECTION('ref_axis',(-0.707106781186546,0.694787886990049,0.131414580971466));
#37853=DIRECTION('center_axis',(1.,0.,0.));
#37854=DIRECTION('ref_axis',(0.,1.,0.));
#37855=DIRECTION('center_axis',(0.707106781186549,-0.707052400311325,0.00876944775867131));
#37856=DIRECTION('ref_axis',(0.707106781186546,0.707052400311328,-0.00876944775867135));
#37857=DIRECTION('',(-1.,0.,0.));
#37858=DIRECTION('center_axis',(-0.707106781186545,-0.705126160196082,-0.0528875997482674));
#37859=DIRECTION('ref_axis',(-0.70710678118655,0.705126160196077,0.052887599748267));
#37860=DIRECTION('center_axis',(-1.,0.,0.));
#37861=DIRECTION('ref_axis',(0.,1.,0.));
#37862=DIRECTION('center_axis',(-0.707106781186538,0.68069047390542,0.191469263158419));
#37863=DIRECTION('ref_axis',(0.707106781186557,0.680690473905402,0.191469263158414));
#37864=DIRECTION('',(1.,0.,0.));
#37865=DIRECTION('center_axis',(0.707106781186543,0.680690473905416,0.191469263158417));
#37866=DIRECTION('ref_axis',(-0.707106781186552,0.680690473905407,0.191469263158415));
#37867=DIRECTION('center_axis',(1.,0.,0.));
#37868=DIRECTION('ref_axis',(0.,1.,0.));
#37869=DIRECTION('center_axis',(0.70710678118655,-0.705126160196078,-0.0528875997482671));
#37870=DIRECTION('ref_axis',(0.707106781186546,0.705126160196081,0.0528875997482674));
#37871=DIRECTION('',(-1.,0.,0.));
#37872=DIRECTION('center_axis',(-0.70710678118655,-0.697833484234922,-0.114142140686715));
#37873=DIRECTION('ref_axis',(-0.707106781186545,0.697833484234926,0.114142140686716));
#37874=DIRECTION('center_axis',(-1.,0.,0.));
#37875=DIRECTION('ref_axis',(0.,1.,0.));
#37876=DIRECTION('center_axis',(-0.707106781186541,0.661412595302216,0.250066748640431));
#37877=DIRECTION('ref_axis',(0.707106781186554,0.661412595302203,0.250066748640426));
#37878=DIRECTION('',(1.,0.,0.));
#37879=DIRECTION('center_axis',(0.707106781186545,0.661412595302212,0.25006674864043));
#37880=DIRECTION('ref_axis',(-0.70710678118655,0.661412595302208,0.250066748640428));
#37881=DIRECTION('center_axis',(1.,0.,0.));
#37882=DIRECTION('ref_axis',(0.,1.,0.));
#37883=DIRECTION('center_axis',(0.707106781186551,-0.697833484234921,-0.114142140686715));
#37884=DIRECTION('ref_axis',(0.707106781186544,0.697833484234928,0.114142140686716));
#37885=DIRECTION('',(-1.,0.,0.));
#37886=DIRECTION('center_axis',(-0.707106781186539,-0.685229874095371,-0.174527991013631));
#37887=DIRECTION('ref_axis',(-0.707106781186556,0.685229874095354,0.174527991013627));
#37888=DIRECTION('center_axis',(-1.,0.,0.));
#37889=DIRECTION('ref_axis',(0.,1.,0.));
#37890=DIRECTION('center_axis',(-0.707106781186553,0.637100967476909,0.306761075170854));
#37891=DIRECTION('ref_axis',(0.707106781186542,0.637100967476919,0.306761075170859));
#37892=DIRECTION('',(1.,0.,0.));
#37893=DIRECTION('center_axis',(0.707106781186549,0.637100967476913,0.306761075170856));
#37894=DIRECTION('ref_axis',(-0.707106781186546,0.637100967476915,0.306761075170857));
#37895=DIRECTION('center_axis',(1.,0.,0.));
#37896=DIRECTION('ref_axis',(0.,1.,0.));
#37897=DIRECTION('center_axis',(0.707106781186534,-0.685229874095376,-0.174527991013633));
#37898=DIRECTION('ref_axis',(0.707106781186561,0.68522987409535,0.174527991013626));
#37899=DIRECTION('',(-1.,0.,0.));
#37900=DIRECTION('center_axis',(-0.707106781186562,-0.667411250860812,-0.233585577946042));
#37901=DIRECTION('ref_axis',(-0.707106781186534,0.667411250860838,0.233585577946052));
#37902=DIRECTION('center_axis',(-1.,0.,0.));
#37903=DIRECTION('ref_axis',(0.,1.,0.));
#37904=DIRECTION('center_axis',(-0.707106781186546,0.607940616597039,0.361120764691834));
#37905=DIRECTION('ref_axis',(0.707106781186549,0.607940616597036,0.361120764691832));
#37906=DIRECTION('',(1.,0.,0.));
#37907=DIRECTION('center_axis',(0.707106781186553,0.607940616597033,0.36112076469183));
#37908=DIRECTION('ref_axis',(-0.707106781186542,0.607940616597042,0.361120764691836));
#37909=DIRECTION('center_axis',(1.,0.,0.));
#37910=DIRECTION('ref_axis',(0.,1.,0.));
#37911=DIRECTION('center_axis',(0.707106781186557,-0.667411250860816,-0.233585577946044));
#37912=DIRECTION('ref_axis',(0.707106781186538,0.667411250860834,0.23358557794605));
#37913=DIRECTION('',(-1.,0.,0.));
#37914=DIRECTION('center_axis',(-0.707106781186555,-0.644513225013298,-0.290865437587464));
#37915=DIRECTION('ref_axis',(-0.70710678118654,0.644513225013312,0.29086543758747));
#37916=DIRECTION('center_axis',(-1.,0.,0.));
#37917=DIRECTION('ref_axis',(0.,1.,0.));
#37918=DIRECTION('center_axis',(-0.707106781186541,0.574153470540282,0.412732107142829));
#37919=DIRECTION('ref_axis',(0.707106781186554,0.574153470540271,0.412732107142821));
#37920=DIRECTION('',(1.,0.,0.));
#37921=DIRECTION('center_axis',(0.707106781186542,0.57415347054028,0.412732107142828));
#37922=DIRECTION('ref_axis',(-0.707106781186553,0.574153470540272,0.412732107142822));
#37923=DIRECTION('center_axis',(1.,0.,0.));
#37924=DIRECTION('ref_axis',(0.,1.,0.));
#37925=DIRECTION('center_axis',(0.707106781186557,-0.644513225013297,-0.290865437587463));
#37926=DIRECTION('ref_axis',(0.707106781186538,0.644513225013314,0.290865437587471));
#37927=DIRECTION('',(-1.,0.,0.));
#37928=DIRECTION('center_axis',(-0.707106781186539,-0.616710064355716,-0.345931635619497));
#37929=DIRECTION('ref_axis',(-0.707106781186556,0.616710064355701,0.345931635619489));
#37930=DIRECTION('center_axis',(-1.,0.,0.));
#37931=DIRECTION('ref_axis',(0.,1.,0.));
#37932=DIRECTION('center_axis',(-0.707106781186546,0.535996669889361,0.461202309044001));
#37933=DIRECTION('ref_axis',(0.707106781186549,0.535996669889358,0.461202309043999));
#37934=DIRECTION('',(1.,0.,0.));
#37935=DIRECTION('center_axis',(0.707106781186547,0.53599666988936,0.461202309044));
#37936=DIRECTION('ref_axis',(-0.707106781186548,0.535996669889359,0.461202309044));
#37937=DIRECTION('center_axis',(1.,0.,0.));
#37938=DIRECTION('ref_axis',(0.,1.,0.));
#37939=DIRECTION('center_axis',(0.707106781186546,-0.61671006435571,-0.345931635619494));
#37940=DIRECTION('ref_axis',(0.707106781186549,0.616710064355707,0.345931635619493));
#37941=DIRECTION('',(-1.,0.,0.));
#37942=DIRECTION('center_axis',(-0.70710678118654,-0.584213367728653,-0.398365085025227));
#37943=DIRECTION('ref_axis',(-0.707106781186555,0.584213367728641,0.398365085025218));
#37944=DIRECTION('center_axis',(-1.,0.,0.));
#37945=DIRECTION('ref_axis',(0.,1.,0.));
#37946=DIRECTION('center_axis',(-0.70710678118654,0.493760610936952,0.506162482891787));
#37947=DIRECTION('ref_axis',(0.707106781186555,0.493760610936941,0.506162482891777));
#37948=DIRECTION('',(1.,0.,0.));
#37949=DIRECTION('center_axis',(0.707106781186551,0.493760610936944,0.50616248289178));
#37950=DIRECTION('ref_axis',(-0.707106781186545,0.493760610936949,0.506162482891784));
#37951=DIRECTION('center_axis',(1.,0.,0.));
#37952=DIRECTION('ref_axis',(0.,1.,0.));
#37953=DIRECTION('center_axis',(0.707106781186542,-0.584213367728652,-0.398365085025226));
#37954=DIRECTION('ref_axis',(0.707106781186553,0.584213367728642,0.398365085025219));
#37955=DIRECTION('',(-1.,0.,0.));
#37956=DIRECTION('center_axis',(-0.70710678118655,-0.547270454615492,-0.447766735594494));
#37957=DIRECTION('ref_axis',(-0.707106781186545,0.547270454615496,0.447766735594497));
#37958=DIRECTION('center_axis',(-1.,0.,0.));
#37959=DIRECTION('ref_axis',(0.,1.,0.));
#37960=DIRECTION('center_axis',(-0.70710678118655,0.447766735594494,0.547270454615492));
#37961=DIRECTION('ref_axis',(0.707106781186545,0.447766735594497,0.547270454615496));
#37962=DIRECTION('',(1.,0.,0.));
#37963=DIRECTION('center_axis',(0.707106781186552,0.447766735594493,0.547270454615491));
#37964=DIRECTION('ref_axis',(-0.707106781186544,0.447766735594498,0.547270454615497));
#37965=DIRECTION('center_axis',(1.,0.,0.));
#37966=DIRECTION('ref_axis',(0.,1.,0.));
#37967=DIRECTION('center_axis',(0.707106781186552,-0.547270454615491,-0.447766735594493));
#37968=DIRECTION('ref_axis',(0.707106781186544,0.547270454615497,0.447766735594498));
#37969=DIRECTION('',(-1.,0.,0.));
#37970=DIRECTION('center_axis',(-0.707106781186558,-0.506162482891774,-0.493760610936939));
#37971=DIRECTION('ref_axis',(-0.707106781186537,0.506162482891789,0.493760610936954));
#37972=DIRECTION('center_axis',(-1.,0.,0.));
#37973=DIRECTION('ref_axis',(0.,1.,0.));
#37974=DIRECTION('center_axis',(-0.707106781186547,0.398365085025223,0.584213367728647));
#37975=DIRECTION('ref_axis',(0.707106781186548,0.398365085025222,0.584213367728647));
#37976=DIRECTION('',(1.,0.,0.));
#37977=DIRECTION('center_axis',(0.707106781186549,0.398365085025222,0.584213367728646));
#37978=DIRECTION('ref_axis',(-0.707106781186546,0.398365085025223,0.584213367728648));
#37979=DIRECTION('center_axis',(1.,0.,0.));
#37980=DIRECTION('ref_axis',(0.,1.,0.));
#37981=DIRECTION('center_axis',(0.707106781186551,-0.50616248289178,-0.493760610936944));
#37982=DIRECTION('ref_axis',(0.707106781186544,0.506162482891784,0.493760610936949));
#37983=DIRECTION('',(-1.,0.,0.));
#37984=DIRECTION('center_axis',(-0.707106781186551,-0.461202309043998,-0.535996669889357));
#37985=DIRECTION('ref_axis',(-0.707106781186545,0.461202309044002,0.535996669889362));
#37986=DIRECTION('center_axis',(-1.,0.,0.));
#37987=DIRECTION('ref_axis',(0.,1.,0.));
#37988=DIRECTION('center_axis',(-0.707106781186545,0.345931635619495,0.616710064355711));
#37989=DIRECTION('ref_axis',(0.70710678118655,0.345931635619492,0.616710064355706));
#37990=DIRECTION('',(1.,0.,0.));
#37991=DIRECTION('center_axis',(0.707106781186546,0.345931635619494,0.61671006435571));
#37992=DIRECTION('ref_axis',(-0.707106781186549,0.345931635619493,0.616710064355707));
#37993=DIRECTION('center_axis',(1.,0.,0.));
#37994=DIRECTION('ref_axis',(0.,1.,0.));
#37995=DIRECTION('center_axis',(0.707106781186552,-0.461202309043997,-0.535996669889356));
#37996=DIRECTION('ref_axis',(0.707106781186543,0.461202309044003,0.535996669889363));
#37997=DIRECTION('',(-1.,0.,0.));
#37998=DIRECTION('center_axis',(-0.707106781186541,-0.412732107142829,-0.574153470540282));
#37999=DIRECTION('ref_axis',(-0.707106781186554,0.412732107142821,0.57415347054027));
#38000=DIRECTION('center_axis',(-1.,0.,0.));
#38001=DIRECTION('ref_axis',(0.,1.,0.));
#38002=DIRECTION('center_axis',(-0.707106781186549,0.290865437587466,0.644513225013304));
#38003=DIRECTION('ref_axis',(0.707106781186546,0.290865437587468,0.644513225013307));
#38004=DIRECTION('',(1.,0.,0.));
#38005=DIRECTION('center_axis',(0.707106781186551,0.290865437587466,0.644513225013302));
#38006=DIRECTION('ref_axis',(-0.707106781186544,0.290865437587468,0.644513225013308));
#38007=DIRECTION('center_axis',(1.,0.,0.));
#38008=DIRECTION('ref_axis',(0.,1.,0.));
#38009=DIRECTION('center_axis',(0.707106781186555,-0.412732107142821,-0.57415347054027));
#38010=DIRECTION('ref_axis',(0.70710678118654,0.412732107142829,0.574153470540282));
#38011=DIRECTION('',(-1.,0.,0.));
#38012=DIRECTION('center_axis',(-0.707106781186551,-0.361120764691831,-0.607940616597034));
#38013=DIRECTION('ref_axis',(-0.707106781186544,0.361120764691835,0.60794061659704));
#38014=DIRECTION('center_axis',(-1.,0.,0.));
#38015=DIRECTION('ref_axis',(0.,1.,0.));
#38016=DIRECTION('center_axis',(-0.70710678118655,0.233585577946046,0.667411250860823));
#38017=DIRECTION('ref_axis',(0.707106781186545,0.233585577946048,0.667411250860827));
#38018=DIRECTION('',(1.,0.,0.));
#38019=DIRECTION('center_axis',(0.707106781186551,0.233585577946046,0.667411250860822));
#38020=DIRECTION('ref_axis',(-0.707106781186544,0.233585577946048,0.667411250860829));
#38021=DIRECTION('center_axis',(1.,0.,0.));
#38022=DIRECTION('ref_axis',(0.,1.,0.));
#38023=DIRECTION('center_axis',(0.707106781186553,-0.36112076469183,-0.607940616597033));
#38024=DIRECTION('ref_axis',(0.707106781186542,0.361120764691836,0.607940616597042));
#38025=DIRECTION('',(-1.,0.,0.));
#38026=DIRECTION('center_axis',(-0.707106781186547,-0.306761075170857,-0.637100967476915));
#38027=DIRECTION('ref_axis',(-0.707106781186548,0.306761075170857,0.637100967476914));
#38028=DIRECTION('center_axis',(-1.,0.,0.));
#38029=DIRECTION('ref_axis',(0.,1.,0.));
#38030=DIRECTION('center_axis',(-0.707106781186539,0.174527991013632,0.685229874095371));
#38031=DIRECTION('ref_axis',(0.707106781186556,0.174527991013627,0.685229874095354));
#38032=DIRECTION('',(1.,0.,0.));
#38033=DIRECTION('center_axis',(0.70710678118654,0.174527991013631,0.68522987409537));
#38034=DIRECTION('ref_axis',(-0.707106781186555,0.174527991013628,0.685229874095355));
#38035=DIRECTION('center_axis',(1.,0.,0.));
#38036=DIRECTION('ref_axis',(0.,1.,0.));
#38037=DIRECTION('center_axis',(0.707106781186549,-0.306761075170856,-0.637100967476913));
#38038=DIRECTION('ref_axis',(0.707106781186547,0.306761075170857,0.637100967476915));
#38039=DIRECTION('',(-1.,0.,0.));
#38040=DIRECTION('center_axis',(-0.707106781186544,-0.25006674864043,-0.661412595302213));
#38041=DIRECTION('ref_axis',(-0.707106781186551,0.250066748640427,0.661412595302206));
#38042=DIRECTION('center_axis',(-1.,0.,0.));
#38043=DIRECTION('ref_axis',(0.,1.,0.));
#38044=DIRECTION('center_axis',(-0.707106781186546,0.114142140686716,0.697833484234925));
#38045=DIRECTION('ref_axis',(0.707106781186548,0.114142140686716,0.697833484234923));
#38046=DIRECTION('',(1.,0.,0.));
#38047=DIRECTION('center_axis',(0.707106781186548,0.114142140686716,0.697833484234924));
#38048=DIRECTION('ref_axis',(-0.707106781186547,0.114142140686716,0.697833484234925));
#38049=DIRECTION('center_axis',(1.,0.,0.));
#38050=DIRECTION('ref_axis',(0.,1.,0.));
#38051=DIRECTION('center_axis',(0.707106781186545,-0.25006674864043,-0.661412595302212));
#38052=DIRECTION('ref_axis',(0.70710678118655,0.250066748640428,0.661412595302208));
#38053=DIRECTION('',(-1.,0.,0.));
#38054=DIRECTION('center_axis',(-0.707106781186544,-0.191469263158417,-0.680690473905414));
#38055=DIRECTION('ref_axis',(-0.707106781186551,0.191469263158415,0.680690473905408));
#38056=DIRECTION('center_axis',(-1.,0.,0.));
#38057=DIRECTION('ref_axis',(0.,1.,0.));
#38058=DIRECTION('center_axis',(-0.707106781186545,0.0528875997482675,0.705126160196082));
#38059=DIRECTION('ref_axis',(0.70710678118655,0.0528875997482671,0.705126160196077));
#38060=DIRECTION('',(1.,0.,0.));
#38061=DIRECTION('center_axis',(0.707106781186546,0.0528875997482674,0.705126160196081));
#38062=DIRECTION('ref_axis',(-0.707106781186549,0.0528875997482673,0.705126160196078));
#38063=DIRECTION('center_axis',(1.,0.,0.));
#38064=DIRECTION('ref_axis',(0.,1.,0.));
#38065=DIRECTION('center_axis',(0.707106781186546,-0.191469263158417,-0.680690473905413));
#38066=DIRECTION('ref_axis',(0.707106781186549,0.191469263158416,0.68069047390541));
#38067=DIRECTION('',(-1.,0.,0.));
#38068=DIRECTION('center_axis',(-0.707106781186545,-0.131414580971466,-0.694787886990049));
#38069=DIRECTION('ref_axis',(-0.70710678118655,0.131414580971465,0.694787886990044));
#38070=DIRECTION('center_axis',(-1.,0.,0.));
#38071=DIRECTION('ref_axis',(0.,1.,0.));
#38072=DIRECTION('center_axis',(-0.707106781186548,-0.00876944775867119,
0.707052400311326));
#38073=DIRECTION('ref_axis',(-0.707106781186547,0.00876944775867126,-0.707052400311326));
#38074=DIRECTION('',(1.,0.,0.));
#38075=DIRECTION('center_axis',(0.707106781186549,-0.00876944775867117,
0.707052400311324));
#38076=DIRECTION('ref_axis',(0.707106781186546,0.00876944775867128,-0.707052400311328));
#38077=DIRECTION('center_axis',(1.,0.,0.));
#38078=DIRECTION('ref_axis',(0.,1.,0.));
#38079=DIRECTION('center_axis',(0.707106781186545,-0.131414580971466,-0.694787886990049));
#38080=DIRECTION('ref_axis',(0.70710678118655,0.131414580971465,0.694787886990044));
#38081=DIRECTION('',(-1.,0.,0.));
#38082=DIRECTION('center_axis',(-0.707106781186548,-0.00876944775867143,
-0.707052400311326));
#38083=DIRECTION('ref_axis',(-0.707106781186547,0.00876944775867142,0.707052400311326));
#38084=DIRECTION('center_axis',(-1.,0.,0.));
#38085=DIRECTION('ref_axis',(0.,1.,0.));
#38086=DIRECTION('center_axis',(-0.707106781186548,-0.131414580971466,0.694787886990046));
#38087=DIRECTION('ref_axis',(-0.707106781186547,0.131414580971466,-0.694787886990047));
#38088=DIRECTION('',(1.,0.,0.));
#38089=DIRECTION('center_axis',(0.707106781186549,-0.131414580971465,0.694787886990045));
#38090=DIRECTION('ref_axis',(0.707106781186546,0.131414580971466,-0.694787886990049));
#38091=DIRECTION('center_axis',(1.,0.,0.));
#38092=DIRECTION('ref_axis',(0.,1.,0.));
#38093=DIRECTION('center_axis',(0.707106781186549,-0.00876944775867141,
-0.707052400311324));
#38094=DIRECTION('ref_axis',(0.707106781186546,0.00876944775867144,0.707052400311328));
#38095=DIRECTION('',(-1.,0.,0.));
#38096=DIRECTION('center_axis',(-0.707106781186548,0.0528875997482672,-0.705126160196079));
#38097=DIRECTION('ref_axis',(0.707106781186547,0.0528875997482672,-0.70512616019608));
#38098=DIRECTION('center_axis',(-1.,0.,0.));
#38099=DIRECTION('ref_axis',(0.,1.,0.));
#38100=DIRECTION('center_axis',(-0.707106781186538,-0.191469263158419,0.68069047390542));
#38101=DIRECTION('ref_axis',(-0.707106781186557,0.191469263158414,-0.680690473905402));
#38102=DIRECTION('',(1.,0.,0.));
#38103=DIRECTION('center_axis',(0.707106781186546,-0.191469263158417,0.680690473905413));
#38104=DIRECTION('ref_axis',(0.707106781186549,0.191469263158416,-0.68069047390541));
#38105=DIRECTION('center_axis',(1.,0.,0.));
#38106=DIRECTION('ref_axis',(0.,1.,0.));
#38107=DIRECTION('center_axis',(0.707106781186549,0.0528875997482671,-0.705126160196077));
#38108=DIRECTION('ref_axis',(-0.707106781186546,0.0528875997482673,-0.705126160196081));
#38109=DIRECTION('',(-1.,0.,0.));
#38110=DIRECTION('center_axis',(-0.70710678118655,0.114142140686715,-0.697833484234922));
#38111=DIRECTION('ref_axis',(0.707106781186545,0.114142140686716,-0.697833484234926));
#38112=DIRECTION('center_axis',(-1.,0.,0.));
#38113=DIRECTION('ref_axis',(0.,1.,0.));
#38114=DIRECTION('center_axis',(-0.707106781186544,-0.25006674864043,0.661412595302213));
#38115=DIRECTION('ref_axis',(-0.707106781186551,0.250066748640427,-0.661412595302206));
#38116=DIRECTION('',(1.,0.,0.));
#38117=DIRECTION('center_axis',(0.707106781186545,-0.25006674864043,0.661412595302212));
#38118=DIRECTION('ref_axis',(0.70710678118655,0.250066748640428,-0.661412595302208));
#38119=DIRECTION('center_axis',(1.,0.,0.));
#38120=DIRECTION('ref_axis',(0.,1.,0.));
#38121=DIRECTION('center_axis',(0.707106781186545,0.114142140686716,-0.697833484234927));
#38122=DIRECTION('ref_axis',(-0.70710678118655,0.114142140686715,-0.697833484234922));
#38123=DIRECTION('',(-1.,0.,0.));
#38124=DIRECTION('center_axis',(-0.707106781186539,0.174527991013631,-0.685229874095371));
#38125=DIRECTION('ref_axis',(0.707106781186556,0.174527991013627,-0.685229874095354));
#38126=DIRECTION('center_axis',(-1.,0.,0.));
#38127=DIRECTION('ref_axis',(0.,1.,0.));
#38128=DIRECTION('center_axis',(-0.707106781186553,-0.306761075170854,0.637100967476909));
#38129=DIRECTION('ref_axis',(-0.707106781186542,0.306761075170859,-0.637100967476919));
#38130=DIRECTION('',(1.,0.,0.));
#38131=DIRECTION('center_axis',(0.707106781186549,-0.306761075170856,0.637100967476913));
#38132=DIRECTION('ref_axis',(0.707106781186546,0.306761075170857,-0.637100967476915));
#38133=DIRECTION('center_axis',(1.,0.,0.));
#38134=DIRECTION('ref_axis',(0.,1.,0.));
#38135=DIRECTION('center_axis',(0.707106781186534,0.174527991013633,-0.685229874095376));
#38136=DIRECTION('ref_axis',(-0.707106781186561,0.174527991013626,-0.68522987409535));
#38137=DIRECTION('',(-1.,0.,0.));
#38138=DIRECTION('center_axis',(-0.70710678118655,0.233585577946046,-0.667411250860823));
#38139=DIRECTION('ref_axis',(0.707106781186545,0.233585577946048,-0.667411250860827));
#38140=DIRECTION('center_axis',(-1.,0.,0.));
#38141=DIRECTION('ref_axis',(0.,1.,0.));
#38142=DIRECTION('center_axis',(-0.70710678118654,-0.361120764691837,0.607940616597043));
#38143=DIRECTION('ref_axis',(-0.707106781186555,0.361120764691829,-0.607940616597031));
#38144=DIRECTION('',(1.,0.,0.));
#38145=DIRECTION('center_axis',(0.707106781186547,-0.361120764691833,0.607940616597037));
#38146=DIRECTION('ref_axis',(0.707106781186548,0.361120764691833,-0.607940616597037));
#38147=DIRECTION('center_axis',(1.,0.,0.));
#38148=DIRECTION('ref_axis',(0.,1.,0.));
#38149=DIRECTION('center_axis',(0.707106781186551,0.233585577946046,-0.667411250860822));
#38150=DIRECTION('ref_axis',(-0.707106781186544,0.233585577946048,-0.667411250860829));
#38151=DIRECTION('',(-1.,0.,0.));
#38152=DIRECTION('center_axis',(-0.707106781186549,0.290865437587466,-0.644513225013304));
#38153=DIRECTION('ref_axis',(0.707106781186546,0.290865437587468,-0.644513225013307));
#38154=DIRECTION('center_axis',(-1.,0.,0.));
#38155=DIRECTION('ref_axis',(0.,1.,0.));
#38156=DIRECTION('center_axis',(-0.707106781186541,-0.412732107142829,0.574153470540282));
#38157=DIRECTION('ref_axis',(-0.707106781186554,0.412732107142821,-0.57415347054027));
#38158=DIRECTION('',(1.,0.,0.));
#38159=DIRECTION('center_axis',(0.707106781186542,-0.412732107142828,0.57415347054028));
#38160=DIRECTION('ref_axis',(0.707106781186553,0.412732107142822,-0.574153470540272));
#38161=DIRECTION('center_axis',(1.,0.,0.));
#38162=DIRECTION('ref_axis',(0.,1.,0.));
#38163=DIRECTION('center_axis',(0.707106781186551,0.290865437587465,-0.644513225013302));
#38164=DIRECTION('ref_axis',(-0.707106781186544,0.290865437587468,-0.644513225013308));
#38165=DIRECTION('',(-1.,0.,0.));
#38166=DIRECTION('center_axis',(-0.707106781186545,0.345931635619494,-0.616710064355711));
#38167=DIRECTION('ref_axis',(0.70710678118655,0.345931635619492,-0.616710064355706));
#38168=DIRECTION('center_axis',(-1.,0.,0.));
#38169=DIRECTION('ref_axis',(0.,1.,0.));
#38170=DIRECTION('center_axis',(-0.707106781186546,-0.461202309044001,0.535996669889361));
#38171=DIRECTION('ref_axis',(-0.707106781186549,0.461202309043999,-0.535996669889358));
#38172=DIRECTION('',(1.,0.,0.));
#38173=DIRECTION('center_axis',(0.707106781186547,-0.461202309044,0.53599666988936));
#38174=DIRECTION('ref_axis',(0.707106781186548,0.461202309044,-0.535996669889359));
#38175=DIRECTION('center_axis',(1.,0.,0.));
#38176=DIRECTION('ref_axis',(0.,1.,0.));
#38177=DIRECTION('center_axis',(0.707106781186546,0.345931635619494,-0.61671006435571));
#38178=DIRECTION('ref_axis',(-0.707106781186549,0.345931635619492,-0.616710064355708));
#38179=DIRECTION('',(-1.,0.,0.));
#38180=DIRECTION('center_axis',(-0.70710678118654,0.398365085025227,-0.584213367728653));
#38181=DIRECTION('ref_axis',(0.707106781186555,0.398365085025218,-0.584213367728641));
#38182=DIRECTION('center_axis',(-1.,0.,0.));
#38183=DIRECTION('ref_axis',(0.,1.,0.));
#38184=DIRECTION('center_axis',(-0.707106781186549,-0.506162482891781,0.493760610936946));
#38185=DIRECTION('ref_axis',(-0.707106781186546,0.506162482891783,-0.493760610936947));
#38186=DIRECTION('',(1.,0.,0.));
#38187=DIRECTION('center_axis',(0.707106781186551,-0.50616248289178,0.493760610936944));
#38188=DIRECTION('ref_axis',(0.707106781186544,0.506162482891784,-0.493760610936949));
#38189=DIRECTION('center_axis',(1.,0.,0.));
#38190=DIRECTION('ref_axis',(0.,1.,0.));
#38191=DIRECTION('center_axis',(0.707106781186542,0.398365085025226,-0.584213367728652));
#38192=DIRECTION('ref_axis',(-0.707106781186554,0.398365085025219,-0.584213367728642));
#38193=DIRECTION('',(-1.,0.,0.));
#38194=DIRECTION('center_axis',(-0.70710678118655,0.447766735594494,-0.547270454615492));
#38195=DIRECTION('ref_axis',(0.707106781186545,0.447766735594497,-0.547270454615496));
#38196=DIRECTION('center_axis',(-1.,0.,0.));
#38197=DIRECTION('ref_axis',(0.,1.,0.));
#38198=DIRECTION('center_axis',(-0.70710678118655,-0.547270454615492,0.447766735594494));
#38199=DIRECTION('ref_axis',(-0.707106781186545,0.547270454615496,-0.447766735594497));
#38200=DIRECTION('',(1.,0.,0.));
#38201=DIRECTION('center_axis',(0.707106781186552,-0.547270454615491,0.447766735594493));
#38202=DIRECTION('ref_axis',(0.707106781186544,0.547270454615497,-0.447766735594498));
#38203=DIRECTION('center_axis',(1.,0.,0.));
#38204=DIRECTION('ref_axis',(0.,1.,0.));
#38205=DIRECTION('center_axis',(0.707106781186551,0.447766735594493,-0.547270454615491));
#38206=DIRECTION('ref_axis',(-0.707106781186544,0.447766735594498,-0.547270454615497));
#38207=DIRECTION('',(-1.,0.,0.));
#38208=DIRECTION('center_axis',(-0.707106781186558,0.493760610936939,-0.506162482891774));
#38209=DIRECTION('ref_axis',(0.707106781186537,0.493760610936954,-0.50616248289179));
#38210=DIRECTION('center_axis',(-1.,0.,0.));
#38211=DIRECTION('ref_axis',(0.,1.,0.));
#38212=DIRECTION('center_axis',(-0.707106781186547,-0.584213367728647,0.398365085025223));
#38213=DIRECTION('ref_axis',(-0.707106781186548,0.584213367728646,-0.398365085025223));
#38214=DIRECTION('',(1.,0.,0.));
#38215=DIRECTION('center_axis',(0.707106781186549,-0.584213367728646,0.398365085025222));
#38216=DIRECTION('ref_axis',(0.707106781186546,0.584213367728648,-0.398365085025223));
#38217=DIRECTION('center_axis',(1.,0.,0.));
#38218=DIRECTION('ref_axis',(0.,1.,0.));
#38219=DIRECTION('center_axis',(0.70710678118656,0.493760610936938,-0.506162482891773));
#38220=DIRECTION('ref_axis',(-0.707106781186535,0.493760610936955,-0.506162482891791));
#38221=DIRECTION('',(-1.,0.,0.));
#38222=DIRECTION('center_axis',(-0.707106781186541,0.535996669889364,-0.461202309044004));
#38223=DIRECTION('ref_axis',(0.707106781186554,0.535996669889354,-0.461202309043996));
#38224=DIRECTION('center_axis',(-1.,0.,0.));
#38225=DIRECTION('ref_axis',(0.,1.,0.));
#38226=DIRECTION('center_axis',(-0.707106781186545,-0.616710064355711,0.345931635619495));
#38227=DIRECTION('ref_axis',(-0.70710678118655,0.616710064355706,-0.345931635619492));
#38228=DIRECTION('',(1.,0.,0.));
#38229=DIRECTION('center_axis',(0.707106781186546,-0.61671006435571,0.345931635619494));
#38230=DIRECTION('ref_axis',(0.707106781186549,0.616710064355707,-0.345931635619493));
#38231=DIRECTION('center_axis',(1.,0.,0.));
#38232=DIRECTION('ref_axis',(0.,1.,0.));
#38233=DIRECTION('center_axis',(0.707106781186552,0.535996669889356,-0.461202309043997));
#38234=DIRECTION('ref_axis',(-0.707106781186543,0.535996669889363,-0.461202309044003));
#38235=DIRECTION('',(-1.,0.,0.));
#38236=DIRECTION('center_axis',(-0.707106781186546,0.574153470540278,-0.412732107142826));
#38237=DIRECTION('ref_axis',(0.707106781186549,0.574153470540275,-0.412732107142824));
#38238=DIRECTION('center_axis',(-1.,0.,0.));
#38239=DIRECTION('ref_axis',(0.,1.,0.));
#38240=DIRECTION('center_axis',(-0.707106781186555,-0.644513225013298,0.290865437587464));
#38241=DIRECTION('ref_axis',(-0.70710678118654,0.644513225013312,-0.29086543758747));
#38242=DIRECTION('',(1.,0.,0.));
#38243=DIRECTION('center_axis',(0.707106781186551,-0.644513225013302,0.290865437587466));
#38244=DIRECTION('ref_axis',(0.707106781186544,0.644513225013308,-0.290865437587468));
#38245=DIRECTION('center_axis',(1.,0.,0.));
#38246=DIRECTION('ref_axis',(0.,1.,0.));
#38247=DIRECTION('center_axis',(0.707106781186547,0.574153470540276,-0.412732107142825));
#38248=DIRECTION('ref_axis',(-0.707106781186548,0.574153470540276,-0.412732107142825));
#38249=DIRECTION('',(-1.,0.,0.));
#38250=DIRECTION('center_axis',(-0.707106781186546,0.607940616597039,-0.361120764691834));
#38251=DIRECTION('ref_axis',(0.707106781186549,0.607940616597036,-0.361120764691832));
#38252=DIRECTION('center_axis',(-1.,0.,0.));
#38253=DIRECTION('ref_axis',(0.,1.,0.));
#38254=DIRECTION('center_axis',(-0.707106781186556,-0.667411250860817,0.233585577946044));
#38255=DIRECTION('ref_axis',(-0.707106781186539,0.667411250860833,-0.23358557794605));
#38256=DIRECTION('',(1.,0.,0.));
#38257=DIRECTION('center_axis',(0.707106781186557,-0.667411250860816,0.233585577946044));
#38258=DIRECTION('ref_axis',(0.707106781186538,0.667411250860834,-0.23358557794605));
#38259=DIRECTION('center_axis',(1.,0.,0.));
#38260=DIRECTION('ref_axis',(0.,1.,0.));
#38261=DIRECTION('center_axis',(0.707106781186547,0.607940616597037,-0.361120764691833));
#38262=DIRECTION('ref_axis',(-0.707106781186548,0.607940616597037,-0.361120764691833));
#38263=DIRECTION('',(-1.,0.,0.));
#38264=DIRECTION('center_axis',(-0.707106781186541,0.63710096747692,-0.30676107517086));
#38265=DIRECTION('ref_axis',(0.707106781186554,0.637100967476909,-0.306761075170854));
#38266=DIRECTION('center_axis',(-1.,0.,0.));
#38267=DIRECTION('ref_axis',(0.,1.,0.));
#38268=DIRECTION('center_axis',(-0.707106781186539,-0.685229874095371,0.174527991013632));
#38269=DIRECTION('ref_axis',(-0.707106781186556,0.685229874095354,-0.174527991013627));
#38270=DIRECTION('',(1.,0.,0.));
#38271=DIRECTION('center_axis',(0.70710678118654,-0.68522987409537,0.174527991013631));
#38272=DIRECTION('ref_axis',(0.707106781186555,0.685229874095355,-0.174527991013628));
#38273=DIRECTION('center_axis',(1.,0.,0.));
#38274=DIRECTION('ref_axis',(0.,1.,0.));
#38275=DIRECTION('center_axis',(0.707106781186549,0.637100967476913,-0.306761075170856));
#38276=DIRECTION('ref_axis',(-0.707106781186547,0.637100967476915,-0.306761075170857));
#38277=DIRECTION('',(-1.,0.,0.));
#38278=DIRECTION('center_axis',(-0.707106781186547,0.66141259530221,-0.250066748640429));
#38279=DIRECTION('ref_axis',(0.707106781186548,0.661412595302209,-0.250066748640429));
#38280=DIRECTION('center_axis',(-1.,0.,0.));
#38281=DIRECTION('ref_axis',(0.,1.,0.));
#38282=DIRECTION('center_axis',(-0.707106781186546,-0.697833484234925,0.114142140686716));
#38283=DIRECTION('ref_axis',(-0.707106781186549,0.697833484234923,-0.114142140686716));
#38284=DIRECTION('',(1.,0.,0.));
#38285=DIRECTION('center_axis',(0.707106781186548,-0.697833484234924,0.114142140686716));
#38286=DIRECTION('ref_axis',(0.707106781186547,0.697833484234924,-0.114142140686716));
#38287=DIRECTION('center_axis',(1.,0.,0.));
#38288=DIRECTION('ref_axis',(0.,1.,0.));
#38289=DIRECTION('center_axis',(0.707106781186545,0.661412595302212,-0.25006674864043));
#38290=DIRECTION('ref_axis',(-0.70710678118655,0.661412595302207,-0.250066748640428));
#38291=DIRECTION('',(-1.,0.,0.));
#38292=DIRECTION('center_axis',(-0.707106781186541,0.680690473905417,-0.191469263158418));
#38293=DIRECTION('ref_axis',(0.707106781186554,0.680690473905405,-0.191469263158415));
#38294=DIRECTION('center_axis',(-1.,0.,0.));
#38295=DIRECTION('ref_axis',(0.,1.,0.));
#38296=DIRECTION('center_axis',(-0.707106781186551,-0.705126160196076,0.0528875997482672));
#38297=DIRECTION('ref_axis',(-0.707106781186544,0.705126160196083,-0.0528875997482678));
#38298=DIRECTION('',(1.,0.,0.));
#38299=DIRECTION('center_axis',(0.707106781186553,-0.705126160196074,0.0528875997482671));
#38300=DIRECTION('ref_axis',(0.707106781186542,0.705126160196085,-0.0528875997482679));
#38301=DIRECTION('center_axis',(1.,0.,0.));
#38302=DIRECTION('ref_axis',(0.,1.,0.));
#38303=DIRECTION('center_axis',(0.707106781186543,0.680690473905416,-0.191469263158418));
#38304=DIRECTION('ref_axis',(-0.707106781186552,0.680690473905407,-0.191469263158415));
#38305=DIRECTION('',(-1.,0.,0.));
#38306=DIRECTION('center_axis',(-0.707106781186546,0.694787886990048,-0.131414580971466));
#38307=DIRECTION('ref_axis',(0.707106781186549,0.694787886990046,-0.131414580971466));
#38308=DIRECTION('center_axis',(-1.,0.,0.));
#38309=DIRECTION('ref_axis',(0.,1.,0.));
#38310=DIRECTION('center_axis',(-0.707106781186549,-0.707052400311325,-0.00876944775867129));
#38311=DIRECTION('ref_axis',(-0.707106781186546,0.707052400311328,0.00876944775867133));
#38312=DIRECTION('',(1.,0.,0.));
#38313=DIRECTION('center_axis',(0.707106781186549,-0.707052400311325,-0.00876944775867129));
#38314=DIRECTION('ref_axis',(0.707106781186546,0.707052400311328,0.00876944775867133));
#38315=DIRECTION('center_axis',(1.,0.,0.));
#38316=DIRECTION('ref_axis',(0.,1.,0.));
#38317=DIRECTION('center_axis',(0.707106781186546,0.694787886990048,-0.131414580971466));
#38318=DIRECTION('ref_axis',(-0.707106781186549,0.694787886990046,-0.131414580971466));
#38319=DIRECTION('',(-1.,0.,0.));
#38320=DIRECTION('center_axis',(-0.707106781186548,0.703597544730292,-0.0703597544730292));
#38321=DIRECTION('ref_axis',(0.707106781186547,0.703597544730292,-0.0703597544730292));
#38322=DIRECTION('center_axis',(-1.,0.,0.));
#38323=DIRECTION('ref_axis',(0.,1.,0.));
#38324=DIRECTION('center_axis',(-0.707106781186548,-0.703597544730292,-0.070359754473029));
#38325=DIRECTION('ref_axis',(-0.707106781186547,0.703597544730292,0.070359754473029));
#38326=DIRECTION('',(1.,0.,0.));
#38327=DIRECTION('center_axis',(0.707106781186549,-0.70359754473029,-0.0703597544730288));
#38328=DIRECTION('ref_axis',(0.707106781186546,0.703597544730294,0.0703597544730292));
#38329=DIRECTION('center_axis',(1.,0.,0.));
#38330=DIRECTION('ref_axis',(0.,1.,0.));
#38331=DIRECTION('center_axis',(0.707106781186548,0.703597544730291,-0.0703597544730291));
#38332=DIRECTION('ref_axis',(-0.707106781186547,0.703597544730293,-0.0703597544730293));
#38333=DIRECTION('',(-1.,0.,0.));
#38334=DIRECTION('center_axis',(-0.707106781186548,0.707052400311326,-0.00876944775867148));
#38335=DIRECTION('ref_axis',(0.707106781186547,0.707052400311326,-0.00876944775867149));
#38336=DIRECTION('center_axis',(-1.,0.,0.));
#38337=DIRECTION('ref_axis',(0.,1.,0.));
#38338=DIRECTION('center_axis',(-0.707106781186548,-0.694787886990046,-0.131414580971466));
#38339=DIRECTION('ref_axis',(-0.707106781186547,0.694787886990047,0.131414580971466));
#38340=DIRECTION('',(1.,0.,0.));
#38341=DIRECTION('center_axis',(0.707106781186549,-0.694787886990045,-0.131414580971465));
#38342=DIRECTION('ref_axis',(0.707106781186546,0.694787886990049,0.131414580971466));
#38343=DIRECTION('center_axis',(1.,0.,0.));
#38344=DIRECTION('ref_axis',(0.,1.,0.));
#38345=DIRECTION('center_axis',(0.707106781186549,0.707052400311325,-0.00876944775867146));
#38346=DIRECTION('ref_axis',(-0.707106781186546,0.707052400311328,-0.0087694477586715));
#38347=DIRECTION('',(-1.,0.,0.));
#38348=DIRECTION('center_axis',(-0.707106781186545,0.705126160196082,0.0528875997482672));
#38349=DIRECTION('ref_axis',(0.70710678118655,0.705126160196077,0.0528875997482668));
#38350=DIRECTION('center_axis',(-1.,0.,0.));
#38351=DIRECTION('ref_axis',(0.,1.,0.));
#38352=DIRECTION('center_axis',(-0.707106781186538,-0.68069047390542,-0.191469263158418));
#38353=DIRECTION('ref_axis',(-0.707106781186557,0.680690473905402,0.191469263158413));
#38354=DIRECTION('',(1.,0.,0.));
#38355=DIRECTION('center_axis',(0.707106781186543,-0.680690473905416,-0.191469263158417));
#38356=DIRECTION('ref_axis',(0.707106781186552,0.680690473905407,0.191469263158415));
#38357=DIRECTION('center_axis',(1.,0.,0.));
#38358=DIRECTION('ref_axis',(0.,1.,0.));
#38359=DIRECTION('center_axis',(0.70710678118655,0.705126160196078,0.0528875997482669));
#38360=DIRECTION('ref_axis',(-0.707106781186546,0.705126160196081,0.0528875997482672));
#38361=DIRECTION('',(-1.,0.,0.));
#38362=DIRECTION('center_axis',(-0.707106781186546,0.697833484234925,0.114142140686716));
#38363=DIRECTION('ref_axis',(0.707106781186548,0.697833484234923,0.114142140686716));
#38364=DIRECTION('center_axis',(-1.,0.,0.));
#38365=DIRECTION('ref_axis',(0.,1.,0.));
#38366=DIRECTION('center_axis',(-0.707106781186544,-0.661412595302213,-0.25006674864043));
#38367=DIRECTION('ref_axis',(-0.707106781186551,0.661412595302206,0.250066748640427));
#38368=DIRECTION('',(1.,0.,0.));
#38369=DIRECTION('center_axis',(0.707106781186545,-0.661412595302212,-0.25006674864043));
#38370=DIRECTION('ref_axis',(0.70710678118655,0.661412595302208,0.250066748640428));
#38371=DIRECTION('center_axis',(1.,0.,0.));
#38372=DIRECTION('ref_axis',(0.,1.,0.));
#38373=DIRECTION('center_axis',(0.707106781186551,0.697833484234921,0.114142140686715));
#38374=DIRECTION('ref_axis',(-0.707106781186544,0.697833484234928,0.114142140686716));
#38375=DIRECTION('',(-1.,0.,0.));
#38376=DIRECTION('center_axis',(-0.707106781186533,0.685229874095377,0.174527991013633));
#38377=DIRECTION('ref_axis',(0.707106781186563,0.685229874095348,0.174527991013626));
#38378=DIRECTION('center_axis',(-1.,0.,0.));
#38379=DIRECTION('ref_axis',(0.,1.,0.));
#38380=DIRECTION('center_axis',(-0.707106781186553,-0.637100967476909,-0.306761075170854));
#38381=DIRECTION('ref_axis',(-0.707106781186542,0.637100967476919,0.306761075170859));
#38382=DIRECTION('',(1.,0.,0.));
#38383=DIRECTION('center_axis',(0.707106781186549,-0.637100967476913,-0.306761075170856));
#38384=DIRECTION('ref_axis',(0.707106781186546,0.637100967476915,0.306761075170857));
#38385=DIRECTION('center_axis',(1.,0.,0.));
#38386=DIRECTION('ref_axis',(0.,1.,0.));
#38387=DIRECTION('center_axis',(0.707106781186534,0.685229874095376,0.174527991013633));
#38388=DIRECTION('ref_axis',(-0.707106781186561,0.68522987409535,0.174527991013626));
#38389=DIRECTION('',(-1.,0.,0.));
#38390=DIRECTION('center_axis',(-0.707106781186556,0.667411250860817,0.233585577946044));
#38391=DIRECTION('ref_axis',(0.707106781186539,0.667411250860833,0.233585577946049));
#38392=DIRECTION('center_axis',(-1.,0.,0.));
#38393=DIRECTION('ref_axis',(0.,1.,0.));
#38394=DIRECTION('center_axis',(-0.707106781186546,-0.607940616597039,-0.361120764691834));
#38395=DIRECTION('ref_axis',(-0.707106781186549,0.607940616597036,0.361120764691832));
#38396=DIRECTION('',(1.,0.,0.));
#38397=DIRECTION('center_axis',(0.707106781186547,-0.607940616597037,-0.361120764691833));
#38398=DIRECTION('ref_axis',(0.707106781186548,0.607940616597037,0.361120764691833));
#38399=DIRECTION('center_axis',(1.,0.,0.));
#38400=DIRECTION('ref_axis',(0.,1.,0.));
#38401=DIRECTION('center_axis',(0.707106781186557,0.667411250860816,0.233585577946044));
#38402=DIRECTION('ref_axis',(-0.707106781186538,0.667411250860834,0.23358557794605));
#38403=DIRECTION('',(-1.,0.,0.));
#38404=DIRECTION('center_axis',(-0.707106781186549,0.644513225013304,0.290865437587466));
#38405=DIRECTION('ref_axis',(0.707106781186546,0.644513225013307,0.290865437587467));
#38406=DIRECTION('center_axis',(-1.,0.,0.));
#38407=DIRECTION('ref_axis',(0.,1.,0.));
#38408=DIRECTION('center_axis',(-0.707106781186541,-0.574153470540282,-0.412732107142829));
#38409=DIRECTION('ref_axis',(-0.707106781186554,0.574153470540271,0.412732107142821));
#38410=DIRECTION('',(1.,0.,0.));
#38411=DIRECTION('center_axis',(0.707106781186542,-0.574153470540281,-0.412732107142828));
#38412=DIRECTION('ref_axis',(0.707106781186553,0.574153470540272,0.412732107142822));
#38413=DIRECTION('center_axis',(1.,0.,0.));
#38414=DIRECTION('ref_axis',(0.,1.,0.));
#38415=DIRECTION('center_axis',(0.707106781186551,0.644513225013302,0.290865437587465));
#38416=DIRECTION('ref_axis',(-0.707106781186544,0.644513225013308,0.290865437587468));
#38417=DIRECTION('',(-1.,0.,0.));
#38418=DIRECTION('center_axis',(-0.707106781186545,0.616710064355711,0.345931635619494));
#38419=DIRECTION('ref_axis',(0.70710678118655,0.616710064355706,0.345931635619492));
#38420=DIRECTION('center_axis',(-1.,0.,0.));
#38421=DIRECTION('ref_axis',(0.,1.,0.));
#38422=DIRECTION('center_axis',(-0.707106781186546,-0.535996669889361,-0.461202309044001));
#38423=DIRECTION('ref_axis',(-0.707106781186549,0.535996669889358,0.461202309043999));
#38424=DIRECTION('',(1.,0.,0.));
#38425=DIRECTION('center_axis',(0.707106781186547,-0.53599666988936,-0.461202309044));
#38426=DIRECTION('ref_axis',(0.707106781186548,0.535996669889359,0.461202309044));
#38427=DIRECTION('center_axis',(1.,0.,0.));
#38428=DIRECTION('ref_axis',(0.,1.,0.));
#38429=DIRECTION('center_axis',(0.707106781186546,0.61671006435571,0.345931635619494));
#38430=DIRECTION('ref_axis',(-0.707106781186549,0.616710064355708,0.345931635619492));
#38431=DIRECTION('',(-1.,0.,0.));
#38432=DIRECTION('center_axis',(-0.70710678118654,0.584213367728653,0.398365085025227));
#38433=DIRECTION('ref_axis',(0.707106781186555,0.584213367728641,0.398365085025218));
#38434=DIRECTION('center_axis',(-1.,0.,0.));
#38435=DIRECTION('ref_axis',(0.,1.,0.));
#38436=DIRECTION('center_axis',(-0.70710678118654,-0.493760610936952,-0.506162482891787));
#38437=DIRECTION('ref_axis',(-0.707106781186555,0.493760610936941,0.506162482891777));
#38438=DIRECTION('',(1.,0.,0.));
#38439=DIRECTION('center_axis',(0.707106781186551,-0.493760610936944,-0.50616248289178));
#38440=DIRECTION('ref_axis',(0.707106781186545,0.493760610936949,0.506162482891784));
#38441=DIRECTION('center_axis',(1.,0.,0.));
#38442=DIRECTION('ref_axis',(0.,1.,0.));
#38443=DIRECTION('center_axis',(0.707106781186542,0.584213367728652,0.398365085025226));
#38444=DIRECTION('ref_axis',(-0.707106781186553,0.584213367728642,0.398365085025219));
#38445=DIRECTION('',(-1.,0.,0.));
#38446=DIRECTION('center_axis',(-0.707106781186558,0.547270454615486,0.447766735594489));
#38447=DIRECTION('ref_axis',(0.707106781186537,0.547270454615502,0.447766735594502));
#38448=DIRECTION('center_axis',(-1.,0.,0.));
#38449=DIRECTION('ref_axis',(0.,1.,0.));
#38450=DIRECTION('center_axis',(-0.70710678118655,-0.447766735594494,-0.547270454615492));
#38451=DIRECTION('ref_axis',(-0.707106781186545,0.447766735594497,0.547270454615496));
#38452=DIRECTION('',(1.,0.,0.));
#38453=DIRECTION('center_axis',(0.707106781186551,-0.447766735594493,-0.547270454615491));
#38454=DIRECTION('ref_axis',(0.707106781186544,0.447766735594498,0.547270454615497));
#38455=DIRECTION('center_axis',(1.,0.,0.));
#38456=DIRECTION('ref_axis',(0.,1.,0.));
#38457=DIRECTION('center_axis',(0.707106781186551,0.547270454615491,0.447766735594493));
#38458=DIRECTION('ref_axis',(-0.707106781186544,0.547270454615497,0.447766735594498));
#38459=DIRECTION('',(-1.,0.,0.));
#38460=DIRECTION('center_axis',(-0.707106781186558,0.506162482891774,0.493760610936939));
#38461=DIRECTION('ref_axis',(0.707106781186537,0.506162482891789,0.493760610936954));
#38462=DIRECTION('center_axis',(-1.,0.,0.));
#38463=DIRECTION('ref_axis',(0.,1.,0.));
#38464=DIRECTION('center_axis',(-0.707106781186547,-0.398365085025223,-0.584213367728647));
#38465=DIRECTION('ref_axis',(-0.707106781186548,0.398365085025223,0.584213367728646));
#38466=DIRECTION('',(1.,0.,0.));
#38467=DIRECTION('center_axis',(0.707106781186549,-0.398365085025222,-0.584213367728646));
#38468=DIRECTION('ref_axis',(0.707106781186546,0.398365085025223,0.584213367728648));
#38469=DIRECTION('center_axis',(1.,0.,0.));
#38470=DIRECTION('ref_axis',(0.,1.,0.));
#38471=DIRECTION('center_axis',(0.70710678118656,0.506162482891773,0.493760610936938));
#38472=DIRECTION('ref_axis',(-0.707106781186535,0.506162482891791,0.493760610936955));
#38473=DIRECTION('',(-1.,0.,0.));
#38474=DIRECTION('center_axis',(-0.707106781186541,0.461202309044004,0.535996669889364));
#38475=DIRECTION('ref_axis',(0.707106781186554,0.461202309043996,0.535996669889354));
#38476=DIRECTION('center_axis',(-1.,0.,0.));
#38477=DIRECTION('ref_axis',(0.,1.,0.));
#38478=DIRECTION('center_axis',(-0.707106781186545,-0.345931635619495,-0.616710064355711));
#38479=DIRECTION('ref_axis',(-0.70710678118655,0.345931635619492,0.616710064355706));
#38480=DIRECTION('',(1.,0.,0.));
#38481=DIRECTION('center_axis',(0.707106781186546,-0.345931635619494,-0.61671006435571));
#38482=DIRECTION('ref_axis',(0.707106781186549,0.345931635619493,0.616710064355707));
#38483=DIRECTION('center_axis',(1.,0.,0.));
#38484=DIRECTION('ref_axis',(0.,1.,0.));
#38485=DIRECTION('center_axis',(0.707106781186552,0.461202309043997,0.535996669889356));
#38486=DIRECTION('ref_axis',(-0.707106781186543,0.461202309044003,0.535996669889363));
#38487=DIRECTION('',(-1.,0.,0.));
#38488=DIRECTION('center_axis',(-0.707106781186536,0.412732107142832,0.574153470540286));
#38489=DIRECTION('ref_axis',(0.707106781186559,0.412732107142818,0.574153470540266));
#38490=DIRECTION('center_axis',(-1.,0.,0.));
#38491=DIRECTION('ref_axis',(0.,1.,0.));
#38492=DIRECTION('center_axis',(-0.707106781186549,-0.290865437587467,-0.644513225013303));
#38493=DIRECTION('ref_axis',(-0.707106781186546,0.290865437587468,0.644513225013307));
#38494=DIRECTION('',(1.,0.,0.));
#38495=DIRECTION('center_axis',(0.707106781186551,-0.290865437587466,-0.644513225013302));
#38496=DIRECTION('ref_axis',(0.707106781186544,0.290865437587469,0.644513225013308));
#38497=DIRECTION('center_axis',(1.,0.,0.));
#38498=DIRECTION('ref_axis',(0.,1.,0.));
#38499=DIRECTION('center_axis',(0.707106781186547,0.412732107142825,0.574153470540276));
#38500=DIRECTION('ref_axis',(-0.707106781186548,0.412732107142825,0.574153470540276));
#38501=DIRECTION('',(-1.,0.,0.));
#38502=DIRECTION('center_axis',(-0.707106781186546,0.361120764691834,0.607940616597038));
#38503=DIRECTION('ref_axis',(0.707106781186549,0.361120764691833,0.607940616597036));
#38504=DIRECTION('center_axis',(-1.,0.,0.));
#38505=DIRECTION('ref_axis',(0.,1.,0.));
#38506=DIRECTION('center_axis',(-0.70710678118655,-0.233585577946047,-0.667411250860823));
#38507=DIRECTION('ref_axis',(-0.707106781186545,0.233585577946048,0.667411250860827));
#38508=DIRECTION('',(1.,0.,0.));
#38509=DIRECTION('center_axis',(0.707106781186551,-0.233585577946046,-0.667411250860821));
#38510=DIRECTION('ref_axis',(0.707106781186544,0.233585577946049,0.667411250860829));
#38511=DIRECTION('center_axis',(1.,0.,0.));
#38512=DIRECTION('ref_axis',(0.,1.,0.));
#38513=DIRECTION('center_axis',(0.707106781186547,0.361120764691833,0.607940616597037));
#38514=DIRECTION('ref_axis',(-0.707106781186548,0.361120764691833,0.607940616597037));
#38515=DIRECTION('',(-1.,0.,0.));
#38516=DIRECTION('center_axis',(-0.707106781186547,0.306761075170857,0.637100967476914));
#38517=DIRECTION('ref_axis',(0.707106781186548,0.306761075170857,0.637100967476913));
#38518=DIRECTION('center_axis',(-1.,0.,0.));
#38519=DIRECTION('ref_axis',(0.,1.,0.));
#38520=DIRECTION('center_axis',(-0.707106781186545,-0.17452799101363,-0.685229874095365));
#38521=DIRECTION('ref_axis',(-0.707106781186551,0.174527991013629,0.68522987409536));
#38522=DIRECTION('',(1.,0.,0.));
#38523=DIRECTION('center_axis',(0.707106781186546,-0.17452799101363,-0.685229874095364));
#38524=DIRECTION('ref_axis',(0.707106781186549,0.174527991013629,0.685229874095361));
#38525=DIRECTION('center_axis',(1.,0.,0.));
#38526=DIRECTION('ref_axis',(0.,1.,0.));
#38527=DIRECTION('center_axis',(0.707106781186549,0.306761075170857,0.637100967476913));
#38528=DIRECTION('ref_axis',(-0.707106781186546,0.306761075170858,0.637100967476915));
#38529=DIRECTION('',(-1.,0.,0.));
#38530=DIRECTION('center_axis',(-0.707106781186547,0.250066748640429,0.661412595302211));
#38531=DIRECTION('ref_axis',(0.707106781186548,0.250066748640428,0.661412595302209));
#38532=DIRECTION('center_axis',(-1.,0.,0.));
#38533=DIRECTION('ref_axis',(0.,1.,0.));
#38534=DIRECTION('center_axis',(-0.70710678118655,-0.114142140686715,-0.697833484234922));
#38535=DIRECTION('ref_axis',(-0.707106781186545,0.114142140686716,0.697833484234926));
#38536=DIRECTION('',(1.,0.,0.));
#38537=DIRECTION('center_axis',(0.707106781186545,-0.114142140686716,-0.697833484234927));
#38538=DIRECTION('ref_axis',(0.70710678118655,0.114142140686715,0.697833484234922));
#38539=DIRECTION('center_axis',(1.,0.,0.));
#38540=DIRECTION('ref_axis',(0.,1.,0.));
#38541=DIRECTION('center_axis',(0.707106781186545,0.25006674864043,0.661412595302212));
#38542=DIRECTION('ref_axis',(-0.70710678118655,0.250066748640428,0.661412595302208));
#38543=DIRECTION('',(-1.,0.,0.));
#38544=DIRECTION('center_axis',(-0.707106781186541,0.191469263158418,0.680690473905417));
#38545=DIRECTION('ref_axis',(0.707106781186554,0.191469263158414,0.680690473905405));
#38546=DIRECTION('center_axis',(-1.,0.,0.));
#38547=DIRECTION('ref_axis',(0.,1.,0.));
#38548=DIRECTION('center_axis',(-0.707106781186545,-0.0528875997482674,
-0.705126160196082));
#38549=DIRECTION('ref_axis',(-0.70710678118655,0.052887599748267,0.705126160196077));
#38550=DIRECTION('',(1.,0.,0.));
#38551=DIRECTION('center_axis',(0.707106781186546,-0.0528875997482673,-0.705126160196081));
#38552=DIRECTION('ref_axis',(0.707106781186549,0.0528875997482671,0.705126160196078));
#38553=DIRECTION('center_axis',(1.,0.,0.));
#38554=DIRECTION('ref_axis',(0.,1.,0.));
#38555=DIRECTION('center_axis',(0.707106781186546,0.191469263158417,0.680690473905413));
#38556=DIRECTION('ref_axis',(-0.707106781186549,0.191469263158416,0.68069047390541));
#38557=DIRECTION('',(-1.,0.,0.));
#38558=DIRECTION('center_axis',(-0.707106781186545,0.131414580971466,0.694787886990049));
#38559=DIRECTION('ref_axis',(0.70710678118655,0.131414580971465,0.694787886990044));
#38560=DIRECTION('center_axis',(-1.,0.,0.));
#38561=DIRECTION('ref_axis',(0.,1.,0.));
#38562=DIRECTION('center_axis',(-0.707106781186548,0.00876944775867127,
-0.707052400311326));
#38563=DIRECTION('ref_axis',(0.707106781186547,0.00876944775867126,-0.707052400311326));
#38564=DIRECTION('',(1.,0.,0.));
#38565=DIRECTION('center_axis',(0.707106781186549,0.00876944775867125,-0.707052400311324));
#38566=DIRECTION('ref_axis',(-0.707106781186546,0.00876944775867128,-0.707052400311328));
#38567=DIRECTION('center_axis',(1.,0.,0.));
#38568=DIRECTION('ref_axis',(0.,1.,0.));
#38569=DIRECTION('center_axis',(0.707106781186546,0.131414580971466,0.694787886990048));
#38570=DIRECTION('ref_axis',(-0.707106781186549,0.131414580971466,0.694787886990046));
#38571=DIRECTION('',(-1.,0.,0.));
#38572=DIRECTION('center_axis',(-0.707106781186548,0.0703597544730292,0.703597544730292));
#38573=DIRECTION('ref_axis',(0.707106781186547,0.0703597544730293,0.703597544730292));
#38574=DIRECTION('center_axis',(-1.,0.,0.));
#38575=DIRECTION('ref_axis',(0.,1.,0.));
#38576=DIRECTION('center_axis',(-0.707106781186547,0.070359754473029,-0.703597544730292));
#38577=DIRECTION('ref_axis',(0.707106781186548,0.0703597544730289,-0.703597544730292));
#38578=DIRECTION('',(1.,0.,0.));
#38579=DIRECTION('center_axis',(0.707106781186549,0.0703597544730288,-0.70359754473029));
#38580=DIRECTION('ref_axis',(-0.707106781186546,0.0703597544730291,-0.703597544730294));
#38581=DIRECTION('center_axis',(1.,0.,0.));
#38582=DIRECTION('ref_axis',(0.,1.,0.));
#38583=DIRECTION('center_axis',(0.707106781186548,0.0703597544730291,0.703597544730291));
#38584=DIRECTION('ref_axis',(-0.707106781186547,0.0703597544730294,0.703597544730293));
#38585=DIRECTION('',(-1.,0.,0.));
#38586=DIRECTION('center_axis',(-0.707106781186548,0.00876944775867152,
0.707052400311326));
#38587=DIRECTION('ref_axis',(0.707106781186547,0.00876944775867157,0.707052400311326));
#38588=DIRECTION('center_axis',(-1.,0.,0.));
#38589=DIRECTION('ref_axis',(0.,1.,0.));
#38590=DIRECTION('center_axis',(-0.707106781186548,0.131414580971466,-0.694787886990046));
#38591=DIRECTION('ref_axis',(0.707106781186547,0.131414580971466,-0.694787886990047));
#38592=DIRECTION('',(1.,0.,0.));
#38593=DIRECTION('center_axis',(0.707106781186548,0.131414580971466,-0.694787886990046));
#38594=DIRECTION('ref_axis',(-0.707106781186547,0.131414580971466,-0.694787886990047));
#38595=DIRECTION('center_axis',(1.,0.,0.));
#38596=DIRECTION('ref_axis',(0.,1.,0.));
#38597=DIRECTION('center_axis',(0.707106781186549,0.0087694477586715,0.707052400311324));
#38598=DIRECTION('ref_axis',(-0.707106781186546,0.00876944775867159,0.707052400311328));
#38599=DIRECTION('',(-1.,0.,0.));
#38600=DIRECTION('center_axis',(-0.707106781186545,-0.0528875997482672,
0.705126160196082));
#38601=DIRECTION('ref_axis',(-0.70710678118655,0.0528875997482668,-0.705126160196077));
#38602=DIRECTION('center_axis',(-1.,0.,0.));
#38603=DIRECTION('ref_axis',(0.,1.,0.));
#38604=DIRECTION('center_axis',(-0.707106781186544,0.191469263158417,-0.680690473905414));
#38605=DIRECTION('ref_axis',(0.707106781186551,0.191469263158415,-0.680690473905408));
#38606=DIRECTION('',(1.,0.,0.));
#38607=DIRECTION('center_axis',(0.707106781186546,0.191469263158416,-0.680690473905413));
#38608=DIRECTION('ref_axis',(-0.707106781186549,0.191469263158415,-0.68069047390541));
#38609=DIRECTION('center_axis',(1.,0.,0.));
#38610=DIRECTION('ref_axis',(0.,1.,0.));
#38611=DIRECTION('center_axis',(0.707106781186549,-0.0528875997482668,0.705126160196077));
#38612=DIRECTION('ref_axis',(0.707106781186546,0.0528875997482672,-0.705126160196081));
#38613=DIRECTION('',(-1.,0.,0.));
#38614=DIRECTION('center_axis',(-0.70710678118655,-0.114142140686715,0.697833484234922));
#38615=DIRECTION('ref_axis',(-0.707106781186545,0.114142140686716,-0.697833484234926));
#38616=DIRECTION('center_axis',(-1.,0.,0.));
#38617=DIRECTION('ref_axis',(0.,1.,0.));
#38618=DIRECTION('center_axis',(-0.707106781186544,0.25006674864043,-0.661412595302213));
#38619=DIRECTION('ref_axis',(0.707106781186551,0.250066748640427,-0.661412595302206));
#38620=DIRECTION('',(1.,0.,0.));
#38621=DIRECTION('center_axis',(0.707106781186545,0.250066748640429,-0.661412595302212));
#38622=DIRECTION('ref_axis',(-0.70710678118655,0.250066748640428,-0.661412595302208));
#38623=DIRECTION('center_axis',(1.,0.,0.));
#38624=DIRECTION('ref_axis',(0.,1.,0.));
#38625=DIRECTION('center_axis',(0.707106781186551,-0.114142140686715,0.697833484234921));
#38626=DIRECTION('ref_axis',(0.707106781186544,0.114142140686716,-0.697833484234928));
#38627=DIRECTION('',(-1.,0.,0.));
#38628=DIRECTION('center_axis',(-0.707106781186545,-0.17452799101363,0.685229874095366));
#38629=DIRECTION('ref_axis',(-0.70710678118655,0.174527991013628,-0.68522987409536));
#38630=DIRECTION('center_axis',(-1.,0.,0.));
#38631=DIRECTION('ref_axis',(0.,1.,0.));
#38632=DIRECTION('center_axis',(-0.707106781186547,0.306761075170857,-0.637100967476915));
#38633=DIRECTION('ref_axis',(0.707106781186548,0.306761075170856,-0.637100967476914));
#38634=DIRECTION('',(1.,0.,0.));
#38635=DIRECTION('center_axis',(0.707106781186549,0.306761075170856,-0.637100967476913));
#38636=DIRECTION('ref_axis',(-0.707106781186546,0.306761075170857,-0.637100967476915));
#38637=DIRECTION('center_axis',(1.,0.,0.));
#38638=DIRECTION('ref_axis',(0.,1.,0.));
#38639=DIRECTION('center_axis',(0.70710678118654,-0.174527991013631,0.68522987409537));
#38640=DIRECTION('ref_axis',(0.707106781186555,0.174527991013627,-0.685229874095356));
#38641=DIRECTION('',(-1.,0.,0.));
#38642=DIRECTION('center_axis',(-0.70710678118655,-0.233585577946046,0.667411250860823));
#38643=DIRECTION('ref_axis',(-0.707106781186545,0.233585577946047,-0.667411250860828));
#38644=DIRECTION('center_axis',(-1.,0.,0.));
#38645=DIRECTION('ref_axis',(0.,1.,0.));
#38646=DIRECTION('center_axis',(-0.70710678118654,0.361120764691836,-0.607940616597043));
#38647=DIRECTION('ref_axis',(0.707106781186555,0.361120764691829,-0.607940616597031));
#38648=DIRECTION('',(1.,0.,0.));
#38649=DIRECTION('center_axis',(0.707106781186542,0.361120764691835,-0.607940616597042));
#38650=DIRECTION('ref_axis',(-0.707106781186553,0.36112076469183,-0.607940616597033));
#38651=DIRECTION('center_axis',(1.,0.,0.));
#38652=DIRECTION('ref_axis',(0.,1.,0.));
#38653=DIRECTION('center_axis',(0.707106781186551,-0.233585577946045,0.667411250860822));
#38654=DIRECTION('ref_axis',(0.707106781186544,0.233585577946048,-0.667411250860829));
#38655=DIRECTION('',(-1.,0.,0.));
#38656=DIRECTION('center_axis',(-0.707106781186555,-0.290865437587464,0.644513225013298));
#38657=DIRECTION('ref_axis',(-0.70710678118654,0.29086543758747,-0.644513225013312));
#38658=DIRECTION('center_axis',(-1.,0.,0.));
#38659=DIRECTION('ref_axis',(0.,1.,0.));
#38660=DIRECTION('center_axis',(-0.707106781186546,0.412732107142826,-0.574153470540278));
#38661=DIRECTION('ref_axis',(0.707106781186549,0.412732107142824,-0.574153470540275));
#38662=DIRECTION('',(1.,0.,0.));
#38663=DIRECTION('center_axis',(0.707106781186547,0.412732107142825,-0.574153470540276));
#38664=DIRECTION('ref_axis',(-0.707106781186548,0.412732107142825,-0.574153470540276));
#38665=DIRECTION('center_axis',(1.,0.,0.));
#38666=DIRECTION('ref_axis',(0.,1.,0.));
#38667=DIRECTION('center_axis',(0.707106781186557,-0.290865437587463,0.644513225013297));
#38668=DIRECTION('ref_axis',(0.707106781186538,0.290865437587471,-0.644513225013314));
#38669=DIRECTION('',(-1.,0.,0.));
#38670=DIRECTION('center_axis',(-0.707106781186539,-0.345931635619497,0.616710064355716));
#38671=DIRECTION('ref_axis',(-0.707106781186556,0.345931635619489,-0.616710064355701));
#38672=DIRECTION('center_axis',(-1.,0.,0.));
#38673=DIRECTION('ref_axis',(0.,1.,0.));
#38674=DIRECTION('center_axis',(-0.707106781186546,0.461202309044001,-0.535996669889361));
#38675=DIRECTION('ref_axis',(0.707106781186549,0.461202309043999,-0.535996669889358));
#38676=DIRECTION('',(1.,0.,0.));
#38677=DIRECTION('center_axis',(0.707106781186547,0.461202309044,-0.53599666988936));
#38678=DIRECTION('ref_axis',(-0.707106781186548,0.461202309044,-0.535996669889359));
#38679=DIRECTION('center_axis',(1.,0.,0.));
#38680=DIRECTION('ref_axis',(0.,1.,0.));
#38681=DIRECTION('center_axis',(0.707106781186546,-0.345931635619494,0.61671006435571));
#38682=DIRECTION('ref_axis',(0.707106781186549,0.345931635619493,-0.616710064355707));
#38683=DIRECTION('',(-1.,0.,0.));
#38684=DIRECTION('center_axis',(-0.70710678118654,-0.398365085025227,0.584213367728653));
#38685=DIRECTION('ref_axis',(-0.707106781186555,0.398365085025218,-0.584213367728641));
#38686=DIRECTION('center_axis',(-1.,0.,0.));
#38687=DIRECTION('ref_axis',(0.,1.,0.));
#38688=DIRECTION('center_axis',(-0.707106781186549,0.506162482891781,-0.493760610936946));
#38689=DIRECTION('ref_axis',(0.707106781186546,0.506162482891783,-0.493760610936948));
#38690=DIRECTION('',(1.,0.,0.));
#38691=DIRECTION('center_axis',(0.707106781186551,0.50616248289178,-0.493760610936944));
#38692=DIRECTION('ref_axis',(-0.707106781186544,0.506162482891784,-0.493760610936949));
#38693=DIRECTION('center_axis',(1.,0.,0.));
#38694=DIRECTION('ref_axis',(0.,1.,0.));
#38695=DIRECTION('center_axis',(0.707106781186542,-0.398365085025226,0.584213367728652));
#38696=DIRECTION('ref_axis',(0.707106781186554,0.398365085025219,-0.584213367728642));
#38697=DIRECTION('',(-1.,0.,0.));
#38698=DIRECTION('center_axis',(-0.70710678118655,-0.447766735594494,0.547270454615492));
#38699=DIRECTION('ref_axis',(-0.707106781186545,0.447766735594496,-0.547270454615496));
#38700=DIRECTION('center_axis',(-1.,0.,0.));
#38701=DIRECTION('ref_axis',(0.,1.,0.));
#38702=DIRECTION('center_axis',(-0.70710678118655,0.547270454615492,-0.447766735594494));
#38703=DIRECTION('ref_axis',(0.707106781186545,0.547270454615496,-0.447766735594497));
#38704=DIRECTION('',(1.,0.,0.));
#38705=DIRECTION('center_axis',(0.707106781186551,0.547270454615491,-0.447766735594493));
#38706=DIRECTION('ref_axis',(-0.707106781186544,0.547270454615497,-0.447766735594498));
#38707=DIRECTION('center_axis',(1.,0.,0.));
#38708=DIRECTION('ref_axis',(0.,1.,0.));
#38709=DIRECTION('center_axis',(0.707106781186551,-0.447766735594493,0.547270454615491));
#38710=DIRECTION('ref_axis',(0.707106781186544,0.447766735594498,-0.547270454615497));
#38711=DIRECTION('',(-1.,0.,0.));
#38712=DIRECTION('center_axis',(-0.707106781186558,-0.493760610936939,0.506162482891775));
#38713=DIRECTION('ref_axis',(-0.707106781186537,0.493760610936954,-0.50616248289179));
#38714=DIRECTION('center_axis',(-1.,0.,0.));
#38715=DIRECTION('ref_axis',(0.,1.,0.));
#38716=DIRECTION('center_axis',(-0.707106781186557,0.584213367728639,-0.398365085025217));
#38717=DIRECTION('ref_axis',(0.707106781186538,0.584213367728655,-0.398365085025228));
#38718=DIRECTION('',(1.,0.,0.));
#38719=DIRECTION('center_axis',(0.707106781186542,0.584213367728652,-0.398365085025226));
#38720=DIRECTION('ref_axis',(-0.707106781186553,0.584213367728642,-0.39836508502522));
#38721=DIRECTION('center_axis',(1.,0.,0.));
#38722=DIRECTION('ref_axis',(0.,1.,0.));
#38723=DIRECTION('center_axis',(0.70710678118656,-0.493760610936938,0.506162482891773));
#38724=DIRECTION('ref_axis',(0.707106781186535,0.493760610936955,-0.506162482891791));
#38725=DIRECTION('',(-1.,0.,0.));
#38726=DIRECTION('center_axis',(-0.707106781186541,-0.535996669889364,0.461202309044004));
#38727=DIRECTION('ref_axis',(-0.707106781186554,0.535996669889354,-0.461202309043996));
#38728=DIRECTION('center_axis',(-1.,0.,0.));
#38729=DIRECTION('ref_axis',(0.,1.,0.));
#38730=DIRECTION('center_axis',(-0.70710678118655,0.616710064355706,-0.345931635619492));
#38731=DIRECTION('ref_axis',(0.707106781186545,0.616710064355711,-0.345931635619495));
#38732=DIRECTION('',(1.,0.,0.));
#38733=DIRECTION('center_axis',(0.707106781186552,0.616710064355705,-0.345931635619491));
#38734=DIRECTION('ref_axis',(-0.707106781186543,0.616710064355712,-0.345931635619496));
#38735=DIRECTION('center_axis',(1.,0.,0.));
#38736=DIRECTION('ref_axis',(0.,1.,0.));
#38737=DIRECTION('center_axis',(0.707106781186552,-0.535996669889356,0.461202309043997));
#38738=DIRECTION('ref_axis',(0.707106781186543,0.535996669889363,-0.461202309044003));
#38739=DIRECTION('',(-1.,0.,0.));
#38740=DIRECTION('center_axis',(-0.707106781186536,-0.574153470540286,0.412732107142832));
#38741=DIRECTION('ref_axis',(-0.707106781186559,0.574153470540266,-0.412732107142818));
#38742=DIRECTION('center_axis',(-1.,0.,0.));
#38743=DIRECTION('ref_axis',(0.,1.,0.));
#38744=DIRECTION('center_axis',(-0.707106781186549,0.644513225013303,-0.290865437587467));
#38745=DIRECTION('ref_axis',(0.707106781186546,0.644513225013307,-0.290865437587468));
#38746=DIRECTION('',(1.,0.,0.));
#38747=DIRECTION('center_axis',(0.707106781186551,0.644513225013302,-0.290865437587466));
#38748=DIRECTION('ref_axis',(-0.707106781186544,0.644513225013308,-0.290865437587469));
#38749=DIRECTION('center_axis',(1.,0.,0.));
#38750=DIRECTION('ref_axis',(0.,1.,0.));
#38751=DIRECTION('center_axis',(0.707106781186547,-0.574153470540276,0.412732107142825));
#38752=DIRECTION('ref_axis',(0.707106781186548,0.574153470540276,-0.412732107142825));
#38753=DIRECTION('',(-1.,0.,0.));
#38754=DIRECTION('center_axis',(-0.707106781186546,-0.607940616597038,0.361120764691834));
#38755=DIRECTION('ref_axis',(-0.707106781186549,0.607940616597036,-0.361120764691833));
#38756=DIRECTION('center_axis',(-1.,0.,0.));
#38757=DIRECTION('ref_axis',(0.,1.,0.));
#38758=DIRECTION('center_axis',(-0.70710678118655,0.667411250860823,-0.233585577946047));
#38759=DIRECTION('ref_axis',(0.707106781186545,0.667411250860827,-0.233585577946048));
#38760=DIRECTION('',(1.,0.,0.));
#38761=DIRECTION('center_axis',(0.707106781186551,0.667411250860821,-0.233585577946046));
#38762=DIRECTION('ref_axis',(-0.707106781186544,0.667411250860829,-0.233585577946049));
#38763=DIRECTION('center_axis',(1.,0.,0.));
#38764=DIRECTION('ref_axis',(0.,1.,0.));
#38765=DIRECTION('center_axis',(0.707106781186547,-0.607940616597037,0.361120764691833));
#38766=DIRECTION('ref_axis',(0.707106781186548,0.607940616597037,-0.361120764691833));
#38767=DIRECTION('',(-1.,0.,0.));
#38768=DIRECTION('center_axis',(-0.707106781186541,-0.637100967476919,0.30676107517086));
#38769=DIRECTION('ref_axis',(-0.707106781186554,0.637100967476908,-0.306761075170855));
#38770=DIRECTION('center_axis',(-1.,0.,0.));
#38771=DIRECTION('ref_axis',(0.,1.,0.));
#38772=DIRECTION('center_axis',(-0.707106781186539,0.685229874095371,-0.174527991013632));
#38773=DIRECTION('ref_axis',(0.707106781186556,0.685229874095354,-0.174527991013628));
#38774=DIRECTION('',(1.,0.,0.));
#38775=DIRECTION('center_axis',(0.707106781186549,0.685229874095361,-0.174527991013629));
#38776=DIRECTION('ref_axis',(-0.707106781186546,0.685229874095364,-0.17452799101363));
#38777=DIRECTION('center_axis',(1.,0.,0.));
#38778=DIRECTION('ref_axis',(0.,1.,0.));
#38779=DIRECTION('center_axis',(0.707106781186543,-0.637100967476918,0.306761075170859));
#38780=DIRECTION('ref_axis',(0.707106781186552,0.63710096747691,-0.306761075170855));
#38781=DIRECTION('',(-1.,0.,0.));
#38782=DIRECTION('center_axis',(-0.707106781186544,-0.661412595302213,0.25006674864043));
#38783=DIRECTION('ref_axis',(-0.707106781186551,0.661412595302206,-0.250066748640427));
#38784=DIRECTION('center_axis',(-1.,0.,0.));
#38785=DIRECTION('ref_axis',(0.,1.,0.));
#38786=DIRECTION('center_axis',(-0.707106781186546,0.697833484234925,-0.114142140686716));
#38787=DIRECTION('ref_axis',(0.707106781186548,0.697833484234923,-0.114142140686715));
#38788=DIRECTION('',(1.,0.,0.));
#38789=DIRECTION('center_axis',(0.707106781186548,0.697833484234924,-0.114142140686716));
#38790=DIRECTION('ref_axis',(-0.707106781186547,0.697833484234925,-0.114142140686716));
#38791=DIRECTION('center_axis',(1.,0.,0.));
#38792=DIRECTION('ref_axis',(0.,1.,0.));
#38793=DIRECTION('center_axis',(0.707106781186545,-0.661412595302212,0.25006674864043));
#38794=DIRECTION('ref_axis',(0.70710678118655,0.661412595302208,-0.250066748640428));
#38795=DIRECTION('',(-1.,0.,0.));
#38796=DIRECTION('center_axis',(-0.707106781186541,-0.680690473905417,0.191469263158418));
#38797=DIRECTION('ref_axis',(-0.707106781186554,0.680690473905405,-0.191469263158414));
#38798=DIRECTION('center_axis',(-1.,0.,0.));
#38799=DIRECTION('ref_axis',(0.,1.,0.));
#38800=DIRECTION('center_axis',(-0.707106781186545,0.705126160196082,-0.0528875997482675));
#38801=DIRECTION('ref_axis',(0.70710678118655,0.705126160196077,-0.0528875997482671));
#38802=DIRECTION('',(1.,0.,0.));
#38803=DIRECTION('center_axis',(0.707106781186546,0.705126160196081,-0.0528875997482674));
#38804=DIRECTION('ref_axis',(-0.707106781186549,0.705126160196078,-0.0528875997482672));
#38805=DIRECTION('center_axis',(1.,0.,0.));
#38806=DIRECTION('ref_axis',(0.,1.,0.));
#38807=DIRECTION('center_axis',(0.707106781186546,-0.680690473905413,0.191469263158417));
#38808=DIRECTION('ref_axis',(0.707106781186549,0.680690473905409,-0.191469263158416));
#38809=DIRECTION('',(-1.,0.,0.));
#38810=DIRECTION('center_axis',(-0.707106781186545,-0.694787886990049,0.131414580971466));
#38811=DIRECTION('ref_axis',(-0.70710678118655,0.694787886990044,-0.131414580971465));
#38812=DIRECTION('center_axis',(-1.,0.,0.));
#38813=DIRECTION('ref_axis',(0.,1.,0.));
#38814=DIRECTION('center_axis',(-0.707106781186548,0.707052400311326,0.00876944775867122));
#38815=DIRECTION('ref_axis',(0.707106781186547,0.707052400311326,0.00876944775867122));
#38816=DIRECTION('',(1.,0.,0.));
#38817=DIRECTION('center_axis',(0.707106781186549,0.707052400311324,0.00876944775867119));
#38818=DIRECTION('ref_axis',(-0.707106781186546,0.707052400311328,0.00876944775867124));
#38819=DIRECTION('center_axis',(1.,0.,0.));
#38820=DIRECTION('ref_axis',(0.,1.,0.));
#38821=DIRECTION('center_axis',(0.707106781186546,-0.694787886990048,0.131414580971466));
#38822=DIRECTION('ref_axis',(0.707106781186549,0.694787886990046,-0.131414580971466));
#38823=DIRECTION('center_axis',(-1.,0.,0.));
#38824=DIRECTION('ref_axis',(0.,0.,-1.));
#38825=DIRECTION('center_axis',(-1.,0.,0.));
#38826=DIRECTION('ref_axis',(0.,0.,-1.));
#38827=DIRECTION('center_axis',(1.,0.,0.));
#38828=DIRECTION('ref_axis',(0.,0.,-1.));
#38829=DIRECTION('center_axis',(-1.,0.,0.));
#38830=DIRECTION('ref_axis',(0.,-0.951056516295153,0.309016994374948));
#38831=DIRECTION('center_axis',(-1.,0.,0.));
#38832=DIRECTION('ref_axis',(0.,0.,1.));
#38833=DIRECTION('center_axis',(1.,0.,0.));
#38834=DIRECTION('ref_axis',(0.,0.,1.));
#38835=DIRECTION('center_axis',(-1.,0.,0.));
#38836=DIRECTION('ref_axis',(0.,0.,1.));
#38837=DIRECTION('center_axis',(-1.,0.,0.));
#38838=DIRECTION('ref_axis',(0.,0.,1.));
#38839=DIRECTION('center_axis',(1.,0.,0.));
#38840=DIRECTION('ref_axis',(0.,0.,1.));
#38841=DIRECTION('center_axis',(-1.,0.,0.));
#38842=DIRECTION('ref_axis',(0.,0.,1.));
#38843=DIRECTION('center_axis',(-1.,0.,0.));
#38844=DIRECTION('ref_axis',(0.,0.,1.));
#38845=DIRECTION('center_axis',(1.,0.,0.));
#38846=DIRECTION('ref_axis',(0.,0.,1.));
#38847=DIRECTION('center_axis',(-1.,0.,0.));
#38848=DIRECTION('ref_axis',(0.,0.,1.));
#38849=DIRECTION('center_axis',(-1.,0.,0.));
#38850=DIRECTION('ref_axis',(0.,0.,1.));
#38851=DIRECTION('center_axis',(1.,0.,0.));
#38852=DIRECTION('ref_axis',(0.,0.,1.));
#38853=DIRECTION('center_axis',(-1.,0.,0.));
#38854=DIRECTION('ref_axis',(0.,0.951056516295154,0.309016994374947));
#38855=DIRECTION('center_axis',(-1.,0.,0.));
#38856=DIRECTION('ref_axis',(0.,0.,1.));
#38857=DIRECTION('center_axis',(1.,0.,0.));
#38858=DIRECTION('ref_axis',(0.,0.,1.));
#38859=DIRECTION('center_axis',(-1.,0.,0.));
#38860=DIRECTION('ref_axis',(0.,0.,-1.));
#38861=DIRECTION('center_axis',(1.,0.,0.));
#38862=DIRECTION('ref_axis',(0.,0.,-1.));
#38863=DIRECTION('center_axis',(-1.,0.,0.));
#38864=DIRECTION('ref_axis',(0.,0.,-1.));
#38865=DIRECTION('center_axis',(-1.,0.,0.));
#38866=DIRECTION('ref_axis',(0.,0.,-1.));
#38867=DIRECTION('center_axis',(1.,0.,0.));
#38868=DIRECTION('ref_axis',(0.,0.,-1.));
#38869=DIRECTION('center_axis',(-1.,0.,0.));
#38870=DIRECTION('ref_axis',(0.,0.,-1.));
#38871=DIRECTION('center_axis',(-1.,0.,0.));
#38872=DIRECTION('ref_axis',(0.,0.,-1.));
#38873=DIRECTION('center_axis',(1.,0.,0.));
#38874=DIRECTION('ref_axis',(0.,0.,-1.));
#38875=DIRECTION('center_axis',(-1.,0.,0.));
#38876=DIRECTION('ref_axis',(0.,0.,-1.));
#38877=DIRECTION('center_axis',(-1.,0.,0.));
#38878=DIRECTION('ref_axis',(0.,0.,-1.));
#38879=DIRECTION('center_axis',(1.,0.,0.));
#38880=DIRECTION('ref_axis',(0.,0.,-1.));
#38881=DIRECTION('center_axis',(-1.,0.,0.));
#38882=DIRECTION('ref_axis',(0.,0.,-1.));
#38883=DIRECTION('center_axis',(1.,0.,0.));
#38884=DIRECTION('ref_axis',(0.,0.951056516295154,0.309016994374947));
#38885=DIRECTION('',(1.,0.,0.));
#38886=DIRECTION('center_axis',(-1.,0.,0.));
#38887=DIRECTION('ref_axis',(0.,0.,-1.));
#38888=DIRECTION('',(1.,0.,0.));
#38889=DIRECTION('center_axis',(1.,0.,0.));
#38890=DIRECTION('ref_axis',(0.,0.,-1.));
#38891=DIRECTION('',(1.,0.,0.));
#38892=DIRECTION('center_axis',(-1.,0.,0.));
#38893=DIRECTION('ref_axis',(0.,0.,-1.));
#38894=DIRECTION('center_axis',(1.,0.,0.));
#38895=DIRECTION('ref_axis',(0.,0.,-1.));
#38896=DIRECTION('',(1.,0.,0.));
#38897=DIRECTION('center_axis',(-1.,0.,0.));
#38898=DIRECTION('ref_axis',(0.,0.,-1.));
#38899=DIRECTION('center_axis',(1.,0.,0.));
#38900=DIRECTION('ref_axis',(0.,0.,-1.));
#38901=DIRECTION('',(1.,0.,0.));
#38902=DIRECTION('center_axis',(-1.,0.,0.));
#38903=DIRECTION('ref_axis',(0.,0.,-1.));
#38904=DIRECTION('center_axis',(1.,0.,0.));
#38905=DIRECTION('ref_axis',(0.,0.,-1.));
#38906=DIRECTION('',(1.,0.,0.));
#38907=DIRECTION('center_axis',(-1.,0.,0.));
#38908=DIRECTION('ref_axis',(0.,0.,-1.));
#38909=DIRECTION('center_axis',(1.,0.,0.));
#38910=DIRECTION('ref_axis',(0.,0.,-1.));
#38911=DIRECTION('',(1.,0.,0.));
#38912=DIRECTION('center_axis',(-1.,0.,0.));
#38913=DIRECTION('ref_axis',(0.,0.,-1.));
#38914=DIRECTION('center_axis',(1.,0.,0.));
#38915=DIRECTION('ref_axis',(0.,0.,-1.));
#38916=DIRECTION('center_axis',(-1.,0.,0.));
#38917=DIRECTION('ref_axis',(0.,0.,-1.));
#38918=DIRECTION('center_axis',(-1.,0.,0.));
#38919=DIRECTION('ref_axis',(0.,0.,-1.));
#38920=DIRECTION('center_axis',(-1.,0.,0.));
#38921=DIRECTION('ref_axis',(0.,0.,-1.));
#38922=DIRECTION('center_axis',(-1.,0.,0.));
#38923=DIRECTION('ref_axis',(0.,0.,-1.));
#38924=DIRECTION('center_axis',(-1.,0.,0.));
#38925=DIRECTION('ref_axis',(0.,0.,-1.));
#38926=DIRECTION('center_axis',(0.707106781186548,0.703597544730291,0.070359754473029));
#38927=DIRECTION('ref_axis',(0.099014754297667,0.,-0.995085965347403));
#38928=DIRECTION('',(0.595596683047421,-0.539007590193132,-0.595596683047431));
#38929=DIRECTION('',(0.,0.0995037190209988,-0.995037190209989));
#38930=DIRECTION('',(0.,-0.0995037190209988,0.995037190209989));
#38931=DIRECTION('',(0.557191914001244,-0.615690134680804,0.557191914001238));
#38932=DIRECTION('center_axis',(1.,0.,0.));
#38933=DIRECTION('ref_axis',(0.,0.,-1.));
#38934=DIRECTION('',(0.,1.,0.));
#38935=DIRECTION('',(0.,0.0995037190209988,0.995037190209989));
#38936=DIRECTION('center_axis',(0.707106781186554,0.,0.707106781186541));
#38937=DIRECTION('ref_axis',(0.707106781186541,0.,-0.707106781186554));
#38938=DIRECTION('',(0.557191914001233,0.61569013468081,-0.557191914001243));
#38939=DIRECTION('',(0.,-1.,0.));
#38940=DIRECTION('',(0.705516335778299,-0.0670328270320415,-0.705516335778311));
#38941=DIRECTION('center_axis',(0.,0.671005320760942,0.741452533551882));
#38942=DIRECTION('ref_axis',(1.,0.,0.));
#38943=DIRECTION('',(-1.,0.,0.));
#38944=DIRECTION('',(0.,-0.741452533551882,0.671005320760942));
#38945=DIRECTION('',(1.,0.,0.));
#38946=DIRECTION('center_axis',(0.56100663158041,-0.555465791309817,0.613782790576081));
#38947=DIRECTION('ref_axis',(0.738128342492238,0.,-0.674660321947023));
#38948=DIRECTION('',(0.,0.74145253355187,0.671005320760956));
#38949=DIRECTION('',(-0.705516335778304,-0.708685007986273,0.00350134337820634));
#38950=DIRECTION('center_axis',(-0.561006631580427,0.555465791309797,0.613782790576083));
#38951=DIRECTION('ref_axis',(0.738128342492228,0.,0.674660321947034));
#38952=DIRECTION('',(0.705516335778308,0.708685007986269,0.00350134337825648));
#38953=DIRECTION('',(-0.705516335778288,0.067032827032046,-0.705516335778322));
#38954=DIRECTION('center_axis',(-0.707106781186547,0.703597544730292,0.0703597544730291));
#38955=DIRECTION('ref_axis',(0.0990147542976674,0.,0.995085965347403));
#38956=DIRECTION('',(0.,-0.0995037190209988,0.995037190209989));
#38957=DIRECTION('',(0.,0.0995037190209988,-0.995037190209989));
#38958=DIRECTION('center_axis',(-0.561006631580422,-0.555465791309811,0.613782790576075));
#38959=DIRECTION('ref_axis',(0.738128342492227,0.,0.674660321947036));
#38960=DIRECTION('',(0.705516335778288,0.0670328270320413,0.705516335778322));
#38961=DIRECTION('',(-0.705516335778306,0.708685007986271,-0.0035013433782314));
#38962=DIRECTION('',(0.,-0.74145253355187,-0.671005320760956));
#38963=DIRECTION('center_axis',(-0.707106781186548,-0.703597544730292,0.0703597544730291));
#38964=DIRECTION('ref_axis',(0.0990147542976672,0.,0.995085965347403));
#38965=DIRECTION('',(0.,0.0995037190209988,0.995037190209989));
#38966=DIRECTION('',(0.,-0.0995037190209988,-0.995037190209989));
#38967=DIRECTION('center_axis',(0.,-0.671005320760956,0.74145253355187));
#38968=DIRECTION('ref_axis',(1.,0.,0.));
#38969=DIRECTION('',(-1.,0.,0.));
#38970=DIRECTION('',(1.,0.,0.));
#38971=DIRECTION('center_axis',(-0.707106781186565,0.,0.70710678118653));
#38972=DIRECTION('ref_axis',(0.70710678118653,0.,0.707106781186565));
#38973=DIRECTION('',(0.,1.,0.));
#38974=DIRECTION('',(0.,-1.,0.));
#38975=DIRECTION('center_axis',(0.707106781186548,-0.703597544730291,0.070359754473029));
#38976=DIRECTION('ref_axis',(0.099014754297667,0.,-0.995085965347403));
#38977=DIRECTION('',(0.,-0.0995037190209988,-0.995037190209989));
#38978=DIRECTION('center_axis',(0.,0.995037190209989,0.0995037190209988));
#38979=DIRECTION('ref_axis',(0.,-0.0995037190209988,0.995037190209989));
#38980=DIRECTION('center_axis',(0.,0.,1.));
#38981=DIRECTION('ref_axis',(0.,-1.,0.));
#38982=DIRECTION('center_axis',(0.56100663158041,0.499857381275776,0.659859195364379));
#38983=DIRECTION('ref_axis',(0.761867344215962,0.,-0.647733085319344));
#38984=DIRECTION('',(0.705516335778303,-0.705683085390289,-0.0652539879547519));
#38985=DIRECTION('',(0.,0.797113049929627,-0.603830096659556));
#38986=DIRECTION('',(-0.705516335778303,-0.128267547152789,0.696989337291012));
#38987=DIRECTION('center_axis',(0.56100663158041,-0.60684677127256,0.56303512813933));
#38988=DIRECTION('ref_axis',(0.708381704532383,0.,-0.705829554980376));
#38989=DIRECTION('',(0.7055163357783,-0.00528794662205797,-0.708673928947921));
#38990=DIRECTION('',(0.,0.680149115692518,0.733073789207257));
#38991=DIRECTION('',(-0.705516335778302,-0.706293409755775,-0.0582779485356024));
#38992=DIRECTION('center_axis',(-0.561006631580394,0.499857381275784,0.659859195364387));
#38993=DIRECTION('ref_axis',(0.761867344215974,0.,0.64773308531933));
#38994=DIRECTION('',(0.,-0.797113049929627,0.603830096659556));
#38995=DIRECTION('',(0.705516335778304,0.70568308539029,0.0652539879547266));
#38996=DIRECTION('',(-0.705516335778317,0.128267547152785,-0.696989337290998));
#38997=DIRECTION('center_axis',(-0.707106781186548,0.694787886990046,0.131414580971466));
#38998=DIRECTION('ref_axis',(0.182719541232954,0.,0.983165077314903));
#38999=DIRECTION('',(0.,-0.185848282703424,0.982578452753869));
#39000=DIRECTION('',(0.,0.185848282703424,-0.982578452753869));
#39001=DIRECTION('center_axis',(-0.561006631580395,-0.606846771272568,0.563035128139337));
#39002=DIRECTION('ref_axis',(0.708381704532398,0.,0.705829554980361));
#39003=DIRECTION('',(0.705516335778314,0.00528794662205805,0.708673928947907));
#39004=DIRECTION('',(-0.705516335778303,0.706293409755772,0.0582779485356272));
#39005=DIRECTION('',(0.,-0.680149115692518,-0.733073789207257));
#39006=DIRECTION('center_axis',(-0.707106781186548,-0.707052400311326,0.00876944775867132));
#39007=DIRECTION('ref_axis',(0.0124009183210273,0.,0.999923105656027));
#39008=DIRECTION('',(0.,0.0124018719548353,0.999923093828728));
#39009=DIRECTION('',(0.,-0.0124018719548353,-0.999923093828728));
#39010=DIRECTION('center_axis',(0.,-0.733073789207257,0.680149115692518));
#39011=DIRECTION('ref_axis',(1.,0.,0.));
#39012=DIRECTION('',(-1.,0.,0.));
#39013=DIRECTION('',(1.,0.,0.));
#39014=DIRECTION('center_axis',(-0.707106781186531,-0.0616284167162208,
0.704416026402775));
#39015=DIRECTION('ref_axis',(0.705757556807969,0.,0.708453436019931));
#39016=DIRECTION('',(0.,0.996194698091746,0.0871557427476582));
#39017=DIRECTION('',(0.,-0.996194698091746,-0.0871557427476582));
#39018=DIRECTION('center_axis',(0.,0.603830096659556,0.797113049929627));
#39019=DIRECTION('ref_axis',(1.,0.,0.));
#39020=DIRECTION('',(-1.,0.,0.));
#39021=DIRECTION('',(1.,0.,0.));
#39022=DIRECTION('center_axis',(0.707106781186549,-0.707052400311325,0.00876944775867131));
#39023=DIRECTION('ref_axis',(0.0124009183210273,0.,-0.999923105656027));
#39024=DIRECTION('',(0.,0.0124018719548353,0.999923093828728));
#39025=DIRECTION('',(0.,-0.0124018719548353,-0.999923093828728));
#39026=DIRECTION('center_axis',(0.707106781186545,-0.0616284167162196,0.704416026402761));
#39027=DIRECTION('ref_axis',(0.705757556807954,0.,-0.708453436019945));
#39028=DIRECTION('',(0.,0.996194698091746,0.0871557427476582));
#39029=DIRECTION('',(0.,-0.996194698091746,-0.0871557427476582));
#39030=DIRECTION('center_axis',(0.707106781186549,0.694787886990045,0.131414580971465));
#39031=DIRECTION('ref_axis',(0.182719541232953,0.,-0.983165077314903));
#39032=DIRECTION('',(0.,-0.185848282703424,0.982578452753869));
#39033=DIRECTION('',(0.,0.185848282703424,-0.982578452753869));
#39034=DIRECTION('center_axis',(1.,0.,0.));
#39035=DIRECTION('ref_axis',(0.,0.0871557427476582,-0.996194698091746));
#39036=DIRECTION('center_axis',(0.,0.98257845275387,0.185848282703424));
#39037=DIRECTION('ref_axis',(0.,-0.185848282703424,0.982578452753869));
#39038=DIRECTION('center_axis',(0.,-0.0871557427476582,0.996194698091746));
#39039=DIRECTION('ref_axis',(0.,-0.996194698091746,-0.0871557427476582));
#39040=DIRECTION('center_axis',(0.5610066315804,-0.65360928088182,0.508002428407545));
#39041=DIRECTION('ref_axis',(0.671222048820197,0.,-0.741256339721703));
#39042=DIRECTION('',(0.70551633577831,0.0564971782546651,-0.706438085609211));
#39043=DIRECTION('',(0.,0.613669352377492,0.789563123475628));
#39044=DIRECTION('',(-0.705516335778305,-0.698526492205411,-0.11961371007187));
#39045=DIRECTION('center_axis',(0.,-0.789563123475628,0.613669352377492));
#39046=DIRECTION('ref_axis',(1.,0.,0.));
#39047=DIRECTION('',(0.557191914001251,-0.509581057609725,-0.655640386718952));
#39048=DIRECTION('',(1.,0.,0.));
#39049=DIRECTION('',(-1.,0.,0.));
#39050=DIRECTION('',(-0.557191914001243,-0.509581057609728,-0.655640386718956));
#39051=DIRECTION('center_axis',(0.70710678118655,-0.705126160196078,-0.0528875997482671));
#39052=DIRECTION('ref_axis',(-0.0745860273602096,0.,-0.997214582987344));
#39053=DIRECTION('',(0.,-0.0747943608453594,0.997198978933359));
#39054=DIRECTION('',(0.,0.0747943608453594,-0.997198978933359));
#39055=DIRECTION('center_axis',(0.561006631580396,0.440444754748108,0.700913673242075));
#39056=DIRECTION('ref_axis',(0.780718990354275,0.,-0.624882275392894));
#39057=DIRECTION('',(0.705516335778308,-0.697310488411385,-0.1265100102815));
#39058=DIRECTION('',(0.,0.846707054687385,-0.532059360920014));
#39059=DIRECTION('',(-0.705516335778308,-0.188526073789645,0.683157829093256));
#39060=DIRECTION('center_axis',(0.,0.532059360920014,0.846707054687385));
#39061=DIRECTION('ref_axis',(1.,0.,0.));
#39062=DIRECTION('',(0.557191914001251,-0.703091778563843,0.441813446929307));
#39063=DIRECTION('',(1.,0.,0.));
#39064=DIRECTION('',(-1.,0.,0.));
#39065=DIRECTION('',(-0.557191914001251,-0.703091778563842,0.441813446929307));
#39066=DIRECTION('center_axis',(0.707106781186543,-0.122787803968974,0.696364240320023));
#39067=DIRECTION('ref_axis',(0.701673843159868,0.,-0.712498293208665));
#39068=DIRECTION('',(0.,0.984807753012208,0.17364817766693));
#39069=DIRECTION('',(0.,-0.984807753012208,-0.17364817766693));
#39070=DIRECTION('center_axis',(0.707106781186543,0.680690473905416,0.191469263158417));
#39071=DIRECTION('ref_axis',(0.261366100937226,0.,-0.965239742903737));
#39072=DIRECTION('',(0.,-0.270778428736215,0.962641699975202));
#39073=DIRECTION('',(0.,0.270778428736215,-0.962641699975202));
#39074=DIRECTION('center_axis',(-0.707106781186545,-0.705126160196082,-0.0528875997482674));
#39075=DIRECTION('ref_axis',(-0.0745860273602106,0.,0.997214582987344));
#39076=DIRECTION('',(-0.595596683047423,0.634243132390279,-0.49295054534778));
#39077=DIRECTION('',(0.,0.0747943608453594,-0.997198978933359));
#39078=DIRECTION('',(0.,-0.0747943608453594,0.997198978933359));
#39079=DIRECTION('center_axis',(0.,-0.17364817766693,0.984807753012208));
#39080=DIRECTION('ref_axis',(0.,-0.984807753012208,-0.17364817766693));
#39081=DIRECTION('',(0.,0.984807753012208,0.17364817766693));
#39082=DIRECTION('center_axis',(-0.707106781186541,-0.122787803968974,0.696364240320025));
#39083=DIRECTION('ref_axis',(0.701673843159869,0.,0.712498293208664));
#39084=DIRECTION('',(0.595596683047431,0.42739457511896,0.680145916919143));
#39085=DIRECTION('',(0.,-0.984807753012208,-0.17364817766693));
#39086=DIRECTION('center_axis',(-0.707106781186538,0.68069047390542,0.191469263158419));
#39087=DIRECTION('ref_axis',(0.261366100937229,0.,0.965239742903736));
#39088=DIRECTION('',(0.,0.270778428736215,-0.962641699975202));
#39089=DIRECTION('',(0.,-0.270778428736215,0.962641699975202));
#39090=DIRECTION('center_axis',(0.,0.962641699975202,0.270778428736215));
#39091=DIRECTION('ref_axis',(0.,-0.270778428736215,0.962641699975202));
#39092=DIRECTION('center_axis',(0.,-0.997198978933359,-0.0747943608453594));
#39093=DIRECTION('ref_axis',(0.,0.0747943608453594,-0.997198978933359));
#39094=DIRECTION('center_axis',(0.561006631580395,0.37768007768897,0.736633774843153));
#39095=DIRECTION('ref_axis',(0.795555689966288,0.,-0.605880470193802));
#39096=DIRECTION('',(0.705516335778309,-0.683630937568086,-0.186803215041197));
#39097=DIRECTION('',(0.,0.889857107503286,-0.456239332177625));
#39098=DIRECTION('',(-0.705516335778301,-0.247349803169823,0.664127077314131));
#39099=DIRECTION('center_axis',(0.561006631580428,-0.695397429203483,0.449103523455304));
#39100=DIRECTION('ref_axis',(0.624948053917873,0.,-0.780666337114816));
#39101=DIRECTION('',(0.705516335778292,0.117852325490946,-0.698825821880065));
#39102=DIRECTION('',(0.,0.542519194747178,0.84004340562311));
#39103=DIRECTION('',(-0.705516335778305,-0.685443366267552,-0.18003913904971));
#39104=DIRECTION('center_axis',(-0.561006631580391,0.377680077688971,0.736633774843155));
#39105=DIRECTION('ref_axis',(0.795555689966291,0.,0.605880470193798));
#39106=DIRECTION('',(0.,-0.889857107503286,0.456239332177625));
#39107=DIRECTION('',(0.705516335778314,0.683630937568081,0.186803215041198));
#39108=DIRECTION('',(-0.705516335778302,0.247349803169829,-0.664127077314128));
#39109=DIRECTION('center_axis',(-0.707106781186541,0.661412595302216,0.250066748640431));
#39110=DIRECTION('ref_axis',(0.333412439312666,0.,0.942781069661232));
#39111=DIRECTION('',(0.,-0.353647787425838,0.935378662600772));
#39112=DIRECTION('',(0.,0.353647787425838,-0.935378662600772));
#39113=DIRECTION('center_axis',(-0.561006631580427,-0.695397429203484,0.449103523455304));
#39114=DIRECTION('ref_axis',(0.624948053917874,0.,0.780666337114815));
#39115=DIRECTION('',(0.705516335778294,-0.117852325490946,0.698825821880063));
#39116=DIRECTION('',(-0.705516335778306,0.68544336626755,0.180039139049709));
#39117=DIRECTION('',(0.,-0.542519194747178,-0.84004340562311));
#39118=DIRECTION('center_axis',(-0.70710678118655,-0.697833484234922,-0.114142140686715));
#39119=DIRECTION('ref_axis',(-0.159358523666363,0.,0.987220776186805));
#39120=DIRECTION('',(0.,-0.161421363397451,0.986885577683101));
#39121=DIRECTION('',(0.,0.161421363397451,-0.986885577683101));
#39122=DIRECTION('center_axis',(0.,-0.84004340562311,0.542519194747178));
#39123=DIRECTION('ref_axis',(1.,0.,0.));
#39124=DIRECTION('',(-1.,0.,0.));
#39125=DIRECTION('',(1.,0.,0.));
#39126=DIRECTION('center_axis',(-0.707106781186552,-0.183012701892218,0.683012701892215));
#39127=DIRECTION('ref_axis',(0.694746590606862,0.,0.719254596676408));
#39128=DIRECTION('',(0.,0.965925826289068,0.258819045102521));
#39129=DIRECTION('',(0.,-0.965925826289068,-0.258819045102521));
#39130=DIRECTION('center_axis',(0.,0.456239332177625,0.889857107503286));
#39131=DIRECTION('ref_axis',(1.,0.,0.));
#39132=DIRECTION('',(-1.,0.,0.));
#39133=DIRECTION('',(1.,0.,0.));
#39134=DIRECTION('center_axis',(0.707106781186551,-0.697833484234921,-0.114142140686715));
#39135=DIRECTION('ref_axis',(-0.159358523666362,0.,-0.987220776186805));
#39136=DIRECTION('',(0.,-0.161421363397451,0.986885577683101));
#39137=DIRECTION('',(0.,0.161421363397451,-0.986885577683101));
#39138=DIRECTION('center_axis',(0.707106781186553,-0.183012701892218,0.683012701892214));
#39139=DIRECTION('ref_axis',(0.69474659060686,0.,-0.719254596676409));
#39140=DIRECTION('',(0.,0.965925826289068,0.258819045102521));
#39141=DIRECTION('',(0.,-0.965925826289068,-0.258819045102521));
#39142=DIRECTION('center_axis',(0.707106781186545,0.661412595302212,0.25006674864043));
#39143=DIRECTION('ref_axis',(0.333412439312663,0.,-0.942781069661234));
#39144=DIRECTION('',(0.,-0.353647787425838,0.935378662600772));
#39145=DIRECTION('',(0.,0.353647787425838,-0.935378662600772));
#39146=DIRECTION('center_axis',(1.,0.,0.));
#39147=DIRECTION('ref_axis',(0.,0.258819045102521,-0.965925826289068));
#39148=DIRECTION('center_axis',(0.,0.935378662600772,0.353647787425838));
#39149=DIRECTION('ref_axis',(0.,-0.353647787425838,0.935378662600772));
#39150=DIRECTION('center_axis',(0.,-0.258819045102521,0.965925826289068));
#39151=DIRECTION('ref_axis',(0.,-0.965925826289068,-0.258819045102521));
#39152=DIRECTION('center_axis',(0.56100663158041,0.312041027189168,0.76674764862602));
#39153=DIRECTION('ref_axis',(0.807044487383574,0.,-0.590490639539514));
#39154=DIRECTION('',(0.70551633577831,-0.664748542502243,-0.245674734539575));
#39155=DIRECTION('',(0.,0.926234810420662,-0.376947046632547));
#39156=DIRECTION('',(-0.705516335778298,-0.304291051193938,0.640041917465765));
#39157=DIRECTION('center_axis',(0.561006631580392,-0.73189318319651,0.386786669513444));
#39158=DIRECTION('ref_axis',(0.567619122871716,0.,-0.823291279773048));
#39159=DIRECTION('',(0.705516335778307,0.178310545369053,-0.685895071683813));
#39160=DIRECTION('',(0.,0.467240138462762,0.884130450221741));
#39161=DIRECTION('',(-0.705516335778315,-0.667143602430337,-0.239094361468882));
#39162=DIRECTION('center_axis',(-0.561006631580397,0.312041027189172,0.766747648626028));
#39163=DIRECTION('ref_axis',(0.807044487383583,0.,0.590490639539502));
#39164=DIRECTION('',(0.,-0.926234810420662,0.376947046632547));
#39165=DIRECTION('',(0.705516335778304,0.66474854250226,0.245674734539547));
#39166=DIRECTION('',(-0.705516335778316,0.304291051193919,-0.640041917465754));
#39167=DIRECTION('center_axis',(-0.707106781186553,0.637100967476909,0.306761075170854));
#39168=DIRECTION('ref_axis',(0.397987666358438,0.,0.917390765937049));
#39169=DIRECTION('',(0.,-0.433825672914778,0.900996828806872));
#39170=DIRECTION('',(0.,0.433825672914778,-0.900996828806872));
#39171=DIRECTION('center_axis',(-0.56100663158039,-0.731893183196511,0.386786669513445));
#39172=DIRECTION('ref_axis',(0.567619122871719,0.,0.823291279773046));
#39173=DIRECTION('',(0.705516335778319,-0.178310545369067,0.685895071683797));
#39174=DIRECTION('',(-0.705516335778307,0.667143602430338,0.239094361468903));
#39175=DIRECTION('',(0.,-0.467240138462762,-0.884130450221741));
#39176=DIRECTION('center_axis',(-0.707106781186539,-0.685229874095371,-0.174527991013631));
#39177=DIRECTION('ref_axis',(-0.239628661022763,0.,0.97086461714105));
#39178=DIRECTION('',(0.,-0.246819851905204,0.96906138128887));
#39179=DIRECTION('',(0.,0.246819851905204,-0.96906138128887));
#39180=DIRECTION('center_axis',(0.,-0.884130450221741,0.467240138462762));
#39181=DIRECTION('ref_axis',(0.,-0.467240138462762,-0.884130450221741));
#39182=DIRECTION('',(-1.,0.,0.));
#39183=DIRECTION('',(1.,0.,0.));
#39184=DIRECTION('center_axis',(-0.707106781186536,-0.241844762647979,0.664463024388686));
#39185=DIRECTION('ref_axis',(0.684791078771748,0.,0.728739444818671));
#39186=DIRECTION('',(0.,0.939692620785908,0.342020143325669));
#39187=DIRECTION('',(0.,-0.939692620785908,-0.342020143325669));
#39188=DIRECTION('center_axis',(0.,0.376947046632547,0.926234810420662));
#39189=DIRECTION('ref_axis',(1.,0.,0.));
#39190=DIRECTION('',(-1.,0.,0.));
#39191=DIRECTION('',(1.,0.,0.));
#39192=DIRECTION('center_axis',(0.707106781186534,-0.685229874095376,-0.174527991013633));
#39193=DIRECTION('ref_axis',(-0.239628661022766,0.,-0.970864617141049));
#39194=DIRECTION('',(0.,-0.246819851905204,0.96906138128887));
#39195=DIRECTION('',(0.,0.246819851905204,-0.96906138128887));
#39196=DIRECTION('center_axis',(0.707106781186551,-0.241844762647974,0.664463024388671));
#39197=DIRECTION('ref_axis',(0.684791078771732,0.,-0.728739444818686));
#39198=DIRECTION('',(0.,0.939692620785908,0.342020143325669));
#39199=DIRECTION('',(0.,-0.939692620785908,-0.342020143325669));
#39200=DIRECTION('center_axis',(0.707106781186549,0.637100967476913,0.306761075170856));
#39201=DIRECTION('ref_axis',(0.397987666358442,0.,-0.917390765937047));
#39202=DIRECTION('',(0.,-0.433825672914778,0.900996828806872));
#39203=DIRECTION('',(0.,0.433825672914778,-0.900996828806872));
#39204=DIRECTION('center_axis',(1.,0.,0.));
#39205=DIRECTION('ref_axis',(0.,0.342020143325669,-0.939692620785908));
#39206=DIRECTION('center_axis',(0.,0.900996828806872,0.433825672914778));
#39207=DIRECTION('ref_axis',(0.,-0.433825672914778,0.900996828806872));
#39208=DIRECTION('center_axis',(0.,-0.342020143325669,0.939692620785908));
#39209=DIRECTION('ref_axis',(0.,-0.939692620785908,-0.342020143325669));
#39210=DIRECTION('center_axis',(0.707106781186553,0.607940616597033,0.36112076469183));
#39211=DIRECTION('ref_axis',(0.454822071931215,0.,-0.890582327965358));
#39212=DIRECTION('',(0.59559668304742,-0.236796741375872,-0.76758836261155));
#39213=DIRECTION('',(0.,0.510701883081733,-0.859757865108992));
#39214=DIRECTION('',(0.,-0.510701883081733,0.859757865108992));
#39215=DIRECTION('',(0.557191914001231,-0.793484241614037,0.244785476043498));
#39216=DIRECTION('center_axis',(1.,0.,0.));
#39217=DIRECTION('ref_axis',(0.,0.422618261740699,-0.90630778703665));
#39218=DIRECTION('',(0.,0.90630778703665,0.422618261740699));
#39219=DIRECTION('',(0.,-0.330339892306057,0.943862042647771));
#39220=DIRECTION('center_axis',(0.707106781186551,-0.298836238730118,0.640856382055785));
#39221=DIRECTION('ref_axis',(0.671542934237814,0.,-0.740965645273293));
#39222=DIRECTION('',(0.557191914001249,0.793484241614025,-0.244785476043494));
#39223=DIRECTION('',(0.,-0.90630778703665,-0.422618261740699));
#39224=DIRECTION('',(0.705516335778313,0.237411714330102,-0.66774424583727));
#39225=DIRECTION('center_axis',(0.,0.294785966455752,0.955563307154868));
#39226=DIRECTION('ref_axis',(1.,0.,0.));
#39227=DIRECTION('',(-1.,0.,0.));
#39228=DIRECTION('',(0.,-0.955563307154868,0.294785966455752));
#39229=DIRECTION('',(1.,0.,0.));
#39230=DIRECTION('center_axis',(0.561006631580425,-0.762818788136162,0.321526135468429));
#39231=DIRECTION('ref_axis',(0.497247150959866,0.,-0.867608938901793));
#39232=DIRECTION('',(0.,0.388405102597383,0.921488728241597));
#39233=DIRECTION('',(-0.705516335778293,-0.643766472946365,-0.296329931428075));
#39234=DIRECTION('center_axis',(-0.5610066315804,0.244027156056943,0.791026109827971));
#39235=DIRECTION('ref_axis',(0.815685591418257,0.,0.578495476173019));
#39236=DIRECTION('',(0.705516335778303,0.640807009641843,0.302676520965595));
#39237=DIRECTION('',(-0.705516335778314,0.358916460582501,-0.611085652157594));
#39238=DIRECTION('center_axis',(-0.707106781186546,0.607940616597039,0.361120764691834));
#39239=DIRECTION('ref_axis',(0.454822071931222,0.,0.890582327965354));
#39240=DIRECTION('',(0.,-0.510701883081733,0.859757865108992));
#39241=DIRECTION('',(0.,0.510701883081733,-0.859757865108992));
#39242=DIRECTION('center_axis',(-0.561006631580432,-0.762818788136158,0.321526135468427));
#39243=DIRECTION('ref_axis',(0.497247150959859,0.,0.867608938901797));
#39244=DIRECTION('',(0.705516335778298,-0.237411714330121,0.667744245837279));
#39245=DIRECTION('',(-0.705516335778289,0.643766472946371,0.296329931428072));
#39246=DIRECTION('',(0.,-0.388405102597383,-0.921488728241597));
#39247=DIRECTION('center_axis',(-0.707106781186562,-0.667411250860812,-0.233585577946042));
#39248=DIRECTION('ref_axis',(-0.31366848359403,0.,0.949532559947168));
#39249=DIRECTION('',(0.,-0.330339892306057,0.943862042647771));
#39250=DIRECTION('',(0.,0.330339892306057,-0.943862042647771));
#39251=DIRECTION('center_axis',(0.,-0.921488728241597,0.388405102597383));
#39252=DIRECTION('ref_axis',(0.,-0.388405102597383,-0.921488728241597));
#39253=DIRECTION('',(-1.,0.,0.));
#39254=DIRECTION('',(1.,0.,0.));
#39255=DIRECTION('center_axis',(-0.70710678118655,-0.298836238730119,0.640856382055787));
#39256=DIRECTION('ref_axis',(0.671542934237816,0.,0.740965645273291));
#39257=DIRECTION('',(0.,0.90630778703665,0.422618261740699));
#39258=DIRECTION('',(0.,-0.90630778703665,-0.422618261740699));
#39259=DIRECTION('center_axis',(0.707106781186557,-0.667411250860816,-0.233585577946044));
#39260=DIRECTION('ref_axis',(-0.313668483594033,0.,-0.949532559947167));
#39261=DIRECTION('',(0.,0.330339892306057,-0.943862042647771));
#39262=DIRECTION('center_axis',(0.,0.859757865108992,0.510701883081733));
#39263=DIRECTION('ref_axis',(0.,-0.510701883081733,0.859757865108992));
#39264=DIRECTION('center_axis',(0.,-0.422618261740699,0.90630778703665));
#39265=DIRECTION('ref_axis',(0.,-0.90630778703665,-0.422618261740699));
#39266=DIRECTION('center_axis',(0.561006631580408,0.174156090919479,0.809284384699502));
#39267=DIRECTION('ref_axis',(0.821843752318935,0.,-0.569712951208179));
#39268=DIRECTION('',(0.705516335778312,-0.611988548508171,-0.357374756306047));
#39269=DIRECTION('',(0.,0.977619390136733,-0.210381387077569));
#39270=DIRECTION('',(-0.705516335778306,-0.410810298986386,0.577478656052905));
#39271=DIRECTION('center_axis',(0.561006631580416,-0.787938881495562,0.253818593389686));
#39272=DIRECTION('ref_axis',(0.412208150462307,0.,-0.911089699586404));
#39273=DIRECTION('',(0.705516335778306,0.29470603679192,-0.644511483084942));
#39274=DIRECTION('',(0.,0.306614069375781,0.951833920629446));
#39275=DIRECTION('',(-0.705516335778295,-0.6154898918864,-0.351310251680243));
#39276=DIRECTION('center_axis',(-0.561006631580406,0.174156090919479,0.809284384699503));
#39277=DIRECTION('ref_axis',(0.821843752318936,0.,0.569712951208178));
#39278=DIRECTION('',(0.,-0.977619390136733,0.210381387077569));
#39279=DIRECTION('',(0.705516335778313,0.61198854850817,0.357374756306046));
#39280=DIRECTION('',(-0.705516335778307,0.410810298986385,-0.577478656052904));
#39281=DIRECTION('center_axis',(-0.707106781186541,0.574153470540282,0.412732107142829));
#39282=DIRECTION('ref_axis',(0.504101701135477,0.,0.863644298836227));
#39283=DIRECTION('',(0.,-0.583691343548208,0.81197562492164));
#39284=DIRECTION('',(0.,0.583691343548208,-0.81197562492164));
#39285=DIRECTION('center_axis',(-0.561006631580414,-0.787938881495563,0.253818593389686));
#39286=DIRECTION('ref_axis',(0.412208150462309,0.,0.911089699586403));
#39287=DIRECTION('',(0.705516335778305,-0.294706036791931,0.644511483084939));
#39288=DIRECTION('',(-0.705516335778296,0.615489891886399,0.351310251680242));
#39289=DIRECTION('',(0.,-0.306614069375781,-0.951833920629446));
#39290=DIRECTION('center_axis',(-0.707106781186555,-0.644513225013298,-0.290865437587464));
#39291=DIRECTION('ref_axis',(-0.380418570543382,0.,0.924814419862564));
#39292=DIRECTION('',(0.,-0.411345846661781,0.911479343942639));
#39293=DIRECTION('',(0.,0.411345846661781,-0.911479343942639));
#39294=DIRECTION('center_axis',(0.,-0.951833920629447,0.306614069375781));
#39295=DIRECTION('ref_axis',(0.,-0.306614069375781,-0.951833920629446));
#39296=DIRECTION('',(-1.,0.,0.));
#39297=DIRECTION('',(1.,0.,0.));
#39298=DIRECTION('center_axis',(-0.707106781186547,-0.353553390593274,0.612372435695795));
#39299=DIRECTION('ref_axis',(0.654653670707978,0.,0.755928946018454));
#39300=DIRECTION('',(0.,0.866025403784439,0.5));
#39301=DIRECTION('',(0.,-0.866025403784439,-0.5));
#39302=DIRECTION('center_axis',(0.,0.210381387077569,0.977619390136733));
#39303=DIRECTION('ref_axis',(1.,0.,0.));
#39304=DIRECTION('',(-1.,0.,0.));
#39305=DIRECTION('',(1.,0.,0.));
#39306=DIRECTION('center_axis',(0.707106781186557,-0.644513225013297,-0.290865437587463));
#39307=DIRECTION('ref_axis',(-0.38041857054338,0.,-0.924814419862564));
#39308=DIRECTION('',(0.,-0.411345846661781,0.911479343942639));
#39309=DIRECTION('',(0.,0.411345846661781,-0.911479343942639));
#39310=DIRECTION('center_axis',(0.707106781186549,-0.353553390593273,0.612372435695794));
#39311=DIRECTION('ref_axis',(0.654653670707976,0.,-0.755928946018455));
#39312=DIRECTION('',(0.,0.866025403784439,0.5));
#39313=DIRECTION('',(0.,-0.866025403784439,-0.5));
#39314=DIRECTION('center_axis',(0.707106781186542,0.57415347054028,0.412732107142828));
#39315=DIRECTION('ref_axis',(0.504101701135476,0.,-0.863644298836228));
#39316=DIRECTION('',(0.,-0.583691343548208,0.81197562492164));
#39317=DIRECTION('',(0.,0.583691343548208,-0.81197562492164));
#39318=DIRECTION('center_axis',(1.,0.,0.));
#39319=DIRECTION('ref_axis',(0.,0.5,-0.866025403784439));
#39320=DIRECTION('center_axis',(0.,0.81197562492164,0.583691343548208));
#39321=DIRECTION('ref_axis',(0.,-0.583691343548208,0.81197562492164));
#39322=DIRECTION('center_axis',(0.,-0.5,0.866025403784439));
#39323=DIRECTION('ref_axis',(0.,-0.866025403784439,-0.5));
#39324=DIRECTION('center_axis',(0.561006631580412,-0.807062284196263,0.184179338555415));
#39325=DIRECTION('ref_axis',(0.311921838389587,0.,-0.950107765853779));
#39326=DIRECTION('',(0.705516335778304,0.349757468365403,-0.616373598779652));
#39327=DIRECTION('',(0.,0.222489517947625,0.97493508214826));
#39328=DIRECTION('',(-0.705516335778314,-0.582529061106241,-0.403616888790129));
#39329=DIRECTION('center_axis',(0.,-0.97493508214826,0.222489517947625));
#39330=DIRECTION('ref_axis',(0.,-0.222489517947625,-0.97493508214826));
#39331=DIRECTION('',(0.557191914001254,-0.184751680075895,-0.809570248762115));
#39332=DIRECTION('',(1.,0.,0.));
#39333=DIRECTION('',(-1.,0.,0.));
#39334=DIRECTION('',(-0.557191914001257,-0.184751680075895,-0.809570248762113));
#39335=DIRECTION('center_axis',(0.707106781186546,-0.61671006435571,-0.345931635619494));
#39336=DIRECTION('ref_axis',(-0.439451044888514,0.,-0.898266541259549));
#39337=DIRECTION('',(0.,-0.489221210746995,0.872159737063827));
#39338=DIRECTION('',(0.,0.489221210746995,-0.872159737063827));
#39339=DIRECTION('center_axis',(0.561006631580408,0.1029595927718,0.8213835167442));
#39340=DIRECTION('ref_axis',(0.82577204978196,0.,-0.564004008672722));
#39341=DIRECTION('',(0.705516335778304,-0.578512484991598,-0.409353153962201));
#39342=DIRECTION('',(0.,0.992235199256928,-0.124375678311979));
#39343=DIRECTION('',(-0.705516335778303,-0.459577622960939,0.539476698684503));
#39344=DIRECTION('center_axis',(0.,0.124375678311979,0.992235199256928));
#39345=DIRECTION('ref_axis',(1.,0.,0.));
#39346=DIRECTION('',(0.55719191400126,-0.823935984868783,0.103279542068703));
#39347=DIRECTION('',(1.,0.,0.));
#39348=DIRECTION('',(-1.,0.,0.));
#39349=DIRECTION('',(-0.557191914001244,-0.823935984868793,0.103279542068704));
#39350=DIRECTION('center_axis',(0.707106781186547,-0.405579787672639,0.579227965339569));
#39351=DIRECTION('ref_axis',(0.633687274224642,0.,-0.773589321594955));
#39352=DIRECTION('',(0.,0.819152044288992,0.573576436351046));
#39353=DIRECTION('',(0.,-0.819152044288992,-0.573576436351046));
#39354=DIRECTION('center_axis',(0.707106781186547,0.53599666988936,0.461202309044));
#39355=DIRECTION('ref_axis',(0.546305769586287,0.,-0.837585820150231));
#39356=DIRECTION('',(0.,-0.652238560447812,0.758013759944347));
#39357=DIRECTION('',(0.,0.652238560447812,-0.758013759944347));
#39358=DIRECTION('center_axis',(-0.707106781186539,-0.616710064355716,-0.345931635619497));
#39359=DIRECTION('ref_axis',(-0.439451044888521,0.,0.898266541259546));
#39360=DIRECTION('',(-0.595596683047429,0.783149392358831,-0.178722187740901));
#39361=DIRECTION('',(0.,0.489221210746995,-0.872159737063827));
#39362=DIRECTION('',(0.,-0.489221210746995,0.872159737063827));
#39363=DIRECTION('center_axis',(0.,-0.573576436351046,0.819152044288992));
#39364=DIRECTION('ref_axis',(0.,-0.819152044288992,-0.573576436351046));
#39365=DIRECTION('',(0.,0.819152044288992,0.573576436351046));
#39366=DIRECTION('center_axis',(-0.707106781186532,-0.405579787672648,0.579227965339582));
#39367=DIRECTION('ref_axis',(0.633687274224659,0.,0.773589321594942));
#39368=DIRECTION('',(0.595596683047437,0.0999089464291446,0.797046293239175));
#39369=DIRECTION('',(0.,-0.819152044288992,-0.573576436351046));
#39370=DIRECTION('center_axis',(-0.707106781186546,0.535996669889361,0.461202309044001));
#39371=DIRECTION('ref_axis',(0.546305769586289,0.,0.83758582015023));
#39372=DIRECTION('',(0.,0.652238560447812,-0.758013759944347));
#39373=DIRECTION('',(0.,-0.652238560447812,0.758013759944347));
#39374=DIRECTION('center_axis',(0.,0.758013759944347,0.652238560447812));
#39375=DIRECTION('ref_axis',(0.,-0.652238560447812,0.758013759944347));
#39376=DIRECTION('center_axis',(0.,-0.872159737063827,-0.489221210746995));
#39377=DIRECTION('ref_axis',(0.,0.489221210746995,-0.872159737063827));
#39378=DIRECTION('center_axis',(0.56100663158041,0.0309795099544078,0.827231424261547));
#39379=DIRECTION('ref_axis',(0.827628669643383,0.,-0.561276032968025));
#39380=DIRECTION('',(0.705516335778304,-0.540633592148827,-0.458216126942529));
#39381=DIRECTION('',(0.,0.999299499382783,-0.037423395534326));
#39382=DIRECTION('',(-0.705516335778297,-0.50484728372422,0.497368997894162));
#39383=DIRECTION('center_axis',(0.561006631580422,-0.820043455596693,0.113138367744206));
#39384=DIRECTION('ref_axis',(0.197690230426216,0.,-0.980264542250728));
#39385=DIRECTION('',(0.70551633577829,0.402147034415294,-0.583544739211107));
#39386=DIRECTION('',(0.,0.136671686945037,0.990616399010029));
#39387=DIRECTION('',(-0.705516335778305,-0.545134832430407,-0.452851757665825));
#39388=DIRECTION('center_axis',(-0.561006631580388,0.0309795099544084,0.827231424261562));
#39389=DIRECTION('ref_axis',(0.827628669643398,0.,0.561276032968003));
#39390=DIRECTION('',(0.,-0.999299499382783,0.037423395534326));
#39391=DIRECTION('',(0.705516335778314,0.540633592148832,0.458216126942508));
#39392=DIRECTION('',(-0.705516335778307,0.504847283724225,-0.497368997894142));
#39393=DIRECTION('center_axis',(-0.70710678118654,0.493760610936952,0.506162482891787));
#39394=DIRECTION('ref_axis',(0.582064997116551,0.,0.813142262541868));
#39395=DIRECTION('',(0.,-0.715821848069997,0.698282952552655));
#39396=DIRECTION('',(0.,0.715821848069997,-0.698282952552655));
#39397=DIRECTION('center_axis',(-0.561006631580398,-0.820043455596709,0.113138367744208));
#39398=DIRECTION('ref_axis',(0.197690230426228,0.,0.980264542250726));
#39399=DIRECTION('',(0.70551633577832,-0.402147034415284,0.583544739211079));
#39400=DIRECTION('',(-0.705516335778308,0.545134832430382,0.45285175766585));
#39401=DIRECTION('',(0.,-0.136671686945037,-0.990616399010029));
#39402=DIRECTION('center_axis',(-0.70710678118654,-0.584213367728653,-0.398365085025227));
#39403=DIRECTION('ref_axis',(-0.490839120629142,0.,0.871250226777595));
#39404=DIRECTION('',(0.,-0.563373306018581,0.826202467961513));
#39405=DIRECTION('',(0.,0.563373306018581,-0.826202467961513));
#39406=DIRECTION('center_axis',(0.,-0.990616399010029,0.136671686945037));
#39407=DIRECTION('ref_axis',(0.,-0.136671686945037,-0.990616399010029));
#39408=DIRECTION('',(-1.,0.,0.));
#39409=DIRECTION('',(1.,0.,0.));
#39410=DIRECTION('center_axis',(-0.70710678118653,-0.454519477672055,0.541675220419715));
#39411=DIRECTION('ref_axis',(0.608120402411362,0.,0.793844806099431));
#39412=DIRECTION('',(0.,0.766044443118978,0.642787609686539));
#39413=DIRECTION('',(0.,-0.766044443118978,-0.642787609686539));
#39414=DIRECTION('center_axis',(0.,0.037423395534326,0.999299499382783));
#39415=DIRECTION('ref_axis',(1.,0.,0.));
#39416=DIRECTION('',(-1.,0.,0.));
#39417=DIRECTION('',(1.,0.,0.));
#39418=DIRECTION('center_axis',(0.707106781186542,-0.584213367728652,-0.398365085025226));
#39419=DIRECTION('ref_axis',(-0.490839120629141,0.,-0.871250226777596));
#39420=DIRECTION('',(0.,-0.563373306018581,0.826202467961513));
#39421=DIRECTION('',(0.,0.563373306018581,-0.826202467961513));
#39422=DIRECTION('center_axis',(0.707106781186559,-0.454519477672036,0.541675220419693));
#39423=DIRECTION('ref_axis',(0.60812040241133,0.,-0.793844806099455));
#39424=DIRECTION('',(0.,0.766044443118978,0.642787609686539));
#39425=DIRECTION('',(0.,-0.766044443118978,-0.642787609686539));
#39426=DIRECTION('center_axis',(0.707106781186551,0.493760610936944,0.50616248289178));
#39427=DIRECTION('ref_axis',(0.58206499711654,0.,-0.813142262541876));
#39428=DIRECTION('',(0.,-0.715821848069997,0.698282952552655));
#39429=DIRECTION('',(0.,0.715821848069997,-0.698282952552655));
#39430=DIRECTION('center_axis',(1.,0.,0.));
#39431=DIRECTION('ref_axis',(0.,0.642787609686539,-0.766044443118978));
#39432=DIRECTION('center_axis',(0.,0.698282952552655,0.715821848069998));
#39433=DIRECTION('ref_axis',(0.,-0.715821848069997,0.698282952552655));
#39434=DIRECTION('center_axis',(0.,-0.642787609686539,0.766044443118978));
#39435=DIRECTION('ref_axis',(0.,-0.766044443118978,-0.642787609686539));
#39436=DIRECTION('center_axis',(0.561006631580394,-0.041236345639636,0.826783601144283));
#39437=DIRECTION('ref_axis',(0.827487445286316,0.,-0.561484218739517));
#39438=DIRECTION('',(0.705516335778304,-0.498640151226356,-0.503591798518316));
#39439=DIRECTION('',(0.,0.998758526924799,0.049813701880158));
#39440=DIRECTION('',(-0.705516335778303,-0.546274751823203,0.451476018710246));
#39441=DIRECTION('center_axis',(0.561006631580414,-0.826783601144269,0.0412363456396373));
#39442=DIRECTION('ref_axis',(0.0733064378127061,0.,-0.997309463594531));
#39443=DIRECTION('',(0.705516335778305,0.451476018710272,-0.546274751823179));
#39444=DIRECTION('',(0.,0.0498137018801604,0.998758526924799));
#39445=DIRECTION('',(-0.705516335778304,-0.503591798518341,-0.49864015122633));
#39446=DIRECTION('center_axis',(-0.561006631580412,-0.0412363456396354,
0.826783601144271));
#39447=DIRECTION('ref_axis',(0.827487445286305,0.,0.561484218739534));
#39448=DIRECTION('',(0.,-0.998758526924799,-0.049813701880158));
#39449=DIRECTION('',(0.705516335778288,0.498640151226367,0.503591798518327));
#39450=DIRECTION('',(-0.705516335778307,0.546274751823178,-0.451476018710271));
#39451=DIRECTION('center_axis',(-0.70710678118655,0.447766735594494,0.547270454615492));
#39452=DIRECTION('ref_axis',(0.61205637248212,0.,0.790814135498366));
#39453=DIRECTION('',(0.,-0.773957299203321,0.633237790257263));
#39454=DIRECTION('',(0.,0.773957299203321,-0.633237790257263));
#39455=DIRECTION('center_axis',(-0.561006631580413,-0.82678360114427,0.0412363456396374));
#39456=DIRECTION('ref_axis',(0.0733064378127065,0.,0.997309463594531));
#39457=DIRECTION('',(0.705516335778307,-0.451476018710271,0.546274751823178));
#39458=DIRECTION('',(-0.705516335778306,0.50359179851834,0.498640151226329));
#39459=DIRECTION('',(0.,-0.0498137018801604,-0.998758526924799));
#39460=DIRECTION('center_axis',(-0.70710678118655,-0.547270454615492,-0.447766735594494));
#39461=DIRECTION('ref_axis',(-0.534994468449985,0.,0.844855560867015));
#39462=DIRECTION('',(0.,-0.633237790257263,0.773957299203321));
#39463=DIRECTION('',(0.,0.633237790257263,-0.773957299203321));
#39464=DIRECTION('center_axis',(0.,-0.998758526924799,0.0498137018801604));
#39465=DIRECTION('ref_axis',(0.,-0.0498137018801604,-0.998758526924799));
#39466=DIRECTION('',(-1.,0.,0.));
#39467=DIRECTION('',(1.,0.,0.));
#39468=DIRECTION('center_axis',(-0.707106781186547,-0.500000000000001,0.500000000000001));
#39469=DIRECTION('ref_axis',(0.577350269189627,0.,0.816496580927725));
#39470=DIRECTION('',(0.,0.707106781186548,0.707106781186548));
#39471=DIRECTION('',(0.,-0.707106781186547,-0.707106781186547));
#39472=DIRECTION('center_axis',(0.,-0.049813701880158,0.998758526924799));
#39473=DIRECTION('ref_axis',(1.,0.,0.));
#39474=DIRECTION('',(-1.,0.,0.));
#39475=DIRECTION('',(1.,0.,0.));
#39476=DIRECTION('center_axis',(0.707106781186552,-0.547270454615491,-0.447766735594493));
#39477=DIRECTION('ref_axis',(-0.534994468449983,0.,-0.844855560867016));
#39478=DIRECTION('',(0.,-0.633237790257263,0.773957299203321));
#39479=DIRECTION('',(0.,0.633237790257263,-0.773957299203321));
#39480=DIRECTION('center_axis',(0.707106781186548,-0.5,0.5));
#39481=DIRECTION('ref_axis',(0.577350269189625,0.,-0.816496580927726));
#39482=DIRECTION('',(0.,0.707106781186548,0.707106781186548));
#39483=DIRECTION('',(0.,-0.707106781186548,-0.707106781186548));
#39484=DIRECTION('center_axis',(0.707106781186552,0.447766735594493,0.547270454615491));
#39485=DIRECTION('ref_axis',(0.612056372482119,0.,-0.790814135498367));
#39486=DIRECTION('',(0.,-0.773957299203321,0.633237790257263));
#39487=DIRECTION('',(0.,0.773957299203321,-0.633237790257263));
#39488=DIRECTION('center_axis',(1.,0.,0.));
#39489=DIRECTION('ref_axis',(0.,0.707106781186548,-0.707106781186548));
#39490=DIRECTION('center_axis',(0.,0.633237790257263,0.773957299203321));
#39491=DIRECTION('ref_axis',(0.,-0.773957299203321,0.633237790257263));
#39492=DIRECTION('center_axis',(0.,-0.707106781186548,0.707106781186548));
#39493=DIRECTION('ref_axis',(0.,-0.707106781186548,-0.707106781186548));
#39494=DIRECTION('center_axis',(0.707106781186549,0.398365085025222,0.584213367728646));
#39495=DIRECTION('ref_axis',(0.636934375125929,0.,-0.770918025332747));
#39496=DIRECTION('',(0.595596683047418,0.109786128885441,-0.795745937499692));
#39497=DIRECTION('',(0.,0.826202467961513,-0.563373306018581));
#39498=DIRECTION('',(0.,-0.826202467961513,0.563373306018581));
#39499=DIRECTION('',(0.557191914001254,-0.822591759450525,-0.1134899478179));
#39500=DIRECTION('center_axis',(1.,0.,0.));
#39501=DIRECTION('ref_axis',(0.,0.766044443118978,-0.642787609686539));
#39502=DIRECTION('',(0.,0.642787609686539,0.766044443118978));
#39503=DIRECTION('',(0.,-0.698282952552655,0.715821848069998));
#39504=DIRECTION('center_axis',(0.707106781186559,-0.541675220419693,0.454519477672036));
#39505=DIRECTION('ref_axis',(0.540716203060924,0.,-0.8412050806714));
#39506=DIRECTION('',(0.557191914001221,0.822591759450547,0.113489947817903));
#39507=DIRECTION('',(0.,-0.642787609686539,-0.766044443118978));
#39508=DIRECTION('',(0.705516335778297,0.497368997894187,-0.504847283724195));
#39509=DIRECTION('center_axis',(0.,-0.136671686945054,0.990616399010027));
#39510=DIRECTION('ref_axis',(1.,0.,0.));
#39511=DIRECTION('',(-1.,0.,0.));
#39512=DIRECTION('',(0.,-0.990616399010027,-0.136671686945054));
#39513=DIRECTION('',(1.,0.,0.));
#39514=DIRECTION('center_axis',(0.56100663158042,-0.827231424261539,-0.0309795099544281));
#39515=DIRECTION('ref_axis',(-0.055137286528771,0.,-0.998478782766186));
#39516=DIRECTION('',(0.,-0.0374233955343508,0.999299499382783));
#39517=DIRECTION('',(-0.705516335778304,-0.458216126942529,-0.540633592148827));
#39518=DIRECTION('center_axis',(-0.561006631580388,-0.113138367744223,0.820043455596714));
#39519=DIRECTION('ref_axis',(0.825342782028785,0.,0.56463199710341));
#39520=DIRECTION('',(0.7055163357783,0.45285175766587,0.545134832430375));
#39521=DIRECTION('',(-0.705516335778316,0.583544739211101,-0.402147034415257));
#39522=DIRECTION('center_axis',(-0.707106781186547,0.398365085025223,0.584213367728647));
#39523=DIRECTION('ref_axis',(0.636934375125931,0.,0.770918025332746));
#39524=DIRECTION('',(0.,-0.826202467961513,0.563373306018581));
#39525=DIRECTION('',(0.,0.826202467961513,-0.563373306018581));
#39526=DIRECTION('center_axis',(-0.56100663158042,-0.827231424261539,-0.0309795099544281));
#39527=DIRECTION('ref_axis',(-0.055137286528771,0.,0.998478782766186));
#39528=DIRECTION('',(0.705516335778325,-0.49736899789418,0.504847283724163));
#39529=DIRECTION('',(-0.705516335778286,0.458216126942515,0.540633592148861));
#39530=DIRECTION('',(0.,0.0374233955343508,-0.999299499382783));
#39531=DIRECTION('center_axis',(-0.707106781186558,-0.506162482891774,-0.493760610936939));
#39532=DIRECTION('ref_axis',(-0.572517134274658,0.,0.819892755768663));
#39533=DIRECTION('',(0.,-0.698282952552655,0.715821848069998));
#39534=DIRECTION('',(0.,0.698282952552655,-0.715821848069998));
#39535=DIRECTION('center_axis',(0.,-0.999299499382783,-0.0374233955343508));
#39536=DIRECTION('ref_axis',(0.,0.0374233955343508,-0.999299499382783));
#39537=DIRECTION('',(-1.,0.,0.));
#39538=DIRECTION('',(1.,0.,0.));
#39539=DIRECTION('center_axis',(-0.70710678118653,-0.541675220419715,0.454519477672055));
#39540=DIRECTION('ref_axis',(0.540716203060955,0.,0.84120508067138));
#39541=DIRECTION('',(0.,0.642787609686539,0.766044443118978));
#39542=DIRECTION('',(0.,-0.642787609686539,-0.766044443118978));
#39543=DIRECTION('center_axis',(0.707106781186551,-0.50616248289178,-0.493760610936944));
#39544=DIRECTION('ref_axis',(-0.572517134274666,0.,-0.819892755768658));
#39545=DIRECTION('',(0.,0.698282952552655,-0.715821848069998));
#39546=DIRECTION('center_axis',(0.,0.563373306018581,0.826202467961513));
#39547=DIRECTION('ref_axis',(0.,-0.826202467961513,0.563373306018581));
#39548=DIRECTION('center_axis',(0.,-0.766044443118978,0.642787609686539));
#39549=DIRECTION('ref_axis',(0.,-0.642787609686539,-0.766044443118978));
#39550=DIRECTION('center_axis',(0.56100663158041,-0.184179338555411,0.807062284196266));
#39551=DIRECTION('ref_axis',(0.821109284001917,0.,-0.570771008133611));
#39552=DIRECTION('',(0.705516335778307,-0.40361688879015,-0.582529061106235));
#39553=DIRECTION('',(0.,0.974935082148261,0.22248951794762));
#39554=DIRECTION('',(-0.705516335778304,-0.616373598779652,0.349757468365403));
#39555=DIRECTION('center_axis',(0.561006631580401,-0.821383516744203,-0.102959592771817));
#39556=DIRECTION('ref_axis',(-0.180511696561755,0.,-0.983572837874449));
#39557=DIRECTION('',(0.705516335778307,0.539476698684506,-0.459577622960929));
#39558=DIRECTION('',(0.,-0.124375678312,0.992235199256925));
#39559=DIRECTION('',(-0.705516335778296,-0.409353153962171,-0.578512484991629));
#39560=DIRECTION('center_axis',(-0.561006631580408,-0.184179338555411,0.807062284196267));
#39561=DIRECTION('ref_axis',(0.821109284001918,0.,0.570771008133609));
#39562=DIRECTION('',(0.,-0.974935082148261,-0.22248951794762));
#39563=DIRECTION('',(0.705516335778308,0.403616888790149,0.582529061106233));
#39564=DIRECTION('',(-0.705516335778306,0.616373598779651,-0.349757468365402));
#39565=DIRECTION('center_axis',(-0.707106781186545,0.345931635619495,0.616710064355711));
#39566=DIRECTION('ref_axis',(0.657291420225582,0.,0.753636509796226));
#39567=DIRECTION('',(0.,-0.872159737063827,0.489221210746995));
#39568=DIRECTION('',(0.,0.872159737063827,-0.489221210746995));
#39569=DIRECTION('center_axis',(-0.561006631580399,-0.821383516744204,-0.102959592771817));
#39570=DIRECTION('ref_axis',(-0.180511696561756,0.,0.983572837874449));
#39571=DIRECTION('',(0.705516335778309,-0.539476698684505,0.459577622960928));
#39572=DIRECTION('',(-0.705516335778298,0.40935315396217,0.578512484991627));
#39573=DIRECTION('',(0.,0.124375678312,-0.992235199256925));
#39574=DIRECTION('center_axis',(-0.707106781186551,-0.461202309043998,-0.535996669889357));
#39575=DIRECTION('ref_axis',(-0.604079438549189,0.,0.796924106751764));
#39576=DIRECTION('',(0.,-0.758013759944347,0.652238560447812));
#39577=DIRECTION('',(0.,0.758013759944347,-0.652238560447812));
#39578=DIRECTION('center_axis',(0.,-0.992235199256925,-0.124375678312));
#39579=DIRECTION('ref_axis',(0.,0.124375678312,-0.992235199256925));
#39580=DIRECTION('',(-1.,0.,0.));
#39581=DIRECTION('',(1.,0.,0.));
#39582=DIRECTION('center_axis',(-0.707106781186546,-0.579227965339571,0.40557978767264));
#39583=DIRECTION('ref_axis',(0.497542812164525,0.,0.867439421552546));
#39584=DIRECTION('',(0.,0.573576436351046,0.819152044288992));
#39585=DIRECTION('',(0.,-0.573576436351046,-0.819152044288992));
#39586=DIRECTION('center_axis',(0.,-0.22248951794762,0.974935082148261));
#39587=DIRECTION('ref_axis',(1.,0.,0.));
#39588=DIRECTION('',(-1.,0.,0.));
#39589=DIRECTION('',(1.,0.,0.));
#39590=DIRECTION('center_axis',(0.707106781186552,-0.461202309043997,-0.535996669889356));
#39591=DIRECTION('ref_axis',(-0.604079438549187,0.,-0.796924106751765));
#39592=DIRECTION('',(0.,-0.758013759944347,0.652238560447812));
#39593=DIRECTION('',(0.,0.758013759944347,-0.652238560447812));
#39594=DIRECTION('center_axis',(0.707106781186547,-0.579227965339569,0.405579787672639));
#39595=DIRECTION('ref_axis',(0.497542812164523,0.,-0.867439421552547));
#39596=DIRECTION('',(0.,0.573576436351046,0.819152044288992));
#39597=DIRECTION('',(0.,-0.573576436351046,-0.819152044288992));
#39598=DIRECTION('center_axis',(0.707106781186546,0.345931635619494,0.61671006435571));
#39599=DIRECTION('ref_axis',(0.657291420225581,0.,-0.753636509796227));
#39600=DIRECTION('',(0.,-0.872159737063827,0.489221210746995));
#39601=DIRECTION('',(0.,0.872159737063827,-0.489221210746995));
#39602=DIRECTION('center_axis',(1.,0.,0.));
#39603=DIRECTION('ref_axis',(0.,0.819152044288992,-0.573576436351046));
#39604=DIRECTION('center_axis',(0.,0.489221210746995,0.872159737063827));
#39605=DIRECTION('ref_axis',(0.,-0.872159737063827,0.489221210746995));
#39606=DIRECTION('center_axis',(0.,-0.819152044288992,0.573576436351046));
#39607=DIRECTION('ref_axis',(0.,-0.573576436351046,-0.819152044288992));
#39608=DIRECTION('center_axis',(0.56100663158041,-0.809284384699501,-0.174156090919474));
#39609=DIRECTION('ref_axis',(-0.296477762129624,0.,-0.955039756535093));
#39610=DIRECTION('',(0.705516335778306,0.577478656052905,-0.410810298986386));
#39611=DIRECTION('',(0.,-0.210381387077564,0.977619390136734));
#39612=DIRECTION('',(-0.705516335778301,-0.357374756306042,-0.611988548508187));
#39613=DIRECTION('center_axis',(0.,-0.977619390136734,-0.210381387077564));
#39614=DIRECTION('ref_axis',(0.,0.210381387077564,-0.977619390136734));
#39615=DIRECTION('',(0.557191914001251,0.174697284967946,-0.811799254493653));
#39616=DIRECTION('',(1.,0.,0.));
#39617=DIRECTION('',(-1.,0.,0.));
#39618=DIRECTION('',(-0.55719191400123,0.174697284967949,-0.811799254493666));
#39619=DIRECTION('center_axis',(0.707106781186555,-0.412732107142821,-0.57415347054027));
#39620=DIRECTION('ref_axis',(-0.630347388214425,0.,-0.776313190774994));
#39621=DIRECTION('',(0.,-0.81197562492164,0.583691343548209));
#39622=DIRECTION('',(0.,0.81197562492164,-0.583691343548209));
#39623=DIRECTION('center_axis',(0.561006631580402,-0.253818593389698,0.787938881495568));
#39624=DIRECTION('ref_axis',(0.814616058663784,0.,-0.580000583592019));
#39625=DIRECTION('',(0.7055163357783,-0.351310251680245,-0.615489891886393));
#39626=DIRECTION('',(0.,0.951833920629443,0.306614069375792));
#39627=DIRECTION('',(-0.705516335778309,-0.644511483084945,0.294706036791908));
#39628=DIRECTION('center_axis',(0.,-0.306614069375792,0.951833920629443));
#39629=DIRECTION('ref_axis',(1.,0.,0.));
#39630=DIRECTION('',(0.557191914001229,-0.790387419648759,-0.254607340492422));
#39631=DIRECTION('',(1.,0.,0.));
#39632=DIRECTION('',(-1.,0.,0.));
#39633=DIRECTION('',(-0.557191914001243,-0.79038741964875,-0.254607340492419));
#39634=DIRECTION('center_axis',(0.707106781186546,-0.612372435695796,0.353553390593275));
#39635=DIRECTION('ref_axis',(0.44721359549996,0.,-0.894427190999915));
#39636=DIRECTION('',(0.,0.5,0.866025403784439));
#39637=DIRECTION('',(0.,-0.5,-0.866025403784439));
#39638=DIRECTION('center_axis',(0.707106781186551,0.290865437587466,0.644513225013302));
#39639=DIRECTION('ref_axis',(0.673638686438954,0.,-0.739060836557317));
#39640=DIRECTION('',(0.,-0.911479343942638,0.411345846661781));
#39641=DIRECTION('',(0.,0.911479343942638,-0.411345846661781));
#39642=DIRECTION('center_axis',(-0.707106781186541,-0.412732107142829,-0.574153470540282));
#39643=DIRECTION('ref_axis',(-0.63034738821444,0.,0.776313190774982));
#39644=DIRECTION('',(-0.595596683047425,0.78530565302539,0.168995924416156));
#39645=DIRECTION('',(0.,0.81197562492164,-0.583691343548209));
#39646=DIRECTION('',(0.,-0.81197562492164,0.583691343548209));
#39647=DIRECTION('center_axis',(0.,-0.866025403784439,0.5));
#39648=DIRECTION('ref_axis',(0.,-0.5,-0.866025403784439));
#39649=DIRECTION('',(0.,0.5,0.866025403784439));
#39650=DIRECTION('center_axis',(-0.707106781186558,-0.612372435695785,0.353553390593269));
#39651=DIRECTION('ref_axis',(0.447213595499947,0.,0.894427190999921));
#39652=DIRECTION('',(0.595596683047419,-0.246298062832259,0.764592607463602));
#39653=DIRECTION('',(0.,-0.5,-0.866025403784438));
#39654=DIRECTION('center_axis',(-0.707106781186549,0.290865437587466,0.644513225013304));
#39655=DIRECTION('ref_axis',(0.673638686438956,0.,0.739060836557315));
#39656=DIRECTION('',(0.,0.911479343942638,-0.411345846661781));
#39657=DIRECTION('',(0.,-0.911479343942638,0.411345846661781));
#39658=DIRECTION('center_axis',(0.,0.411345846661781,0.911479343942639));
#39659=DIRECTION('ref_axis',(0.,-0.911479343942638,0.411345846661781));
#39660=DIRECTION('center_axis',(0.,-0.583691343548209,-0.81197562492164));
#39661=DIRECTION('ref_axis',(0.,0.81197562492164,-0.583691343548209));
#39662=DIRECTION('center_axis',(0.561006631580424,-0.321526135468413,0.762818788136169));
#39663=DIRECTION('ref_axis',(0.805595332751381,0.,-0.592466167683179));
#39664=DIRECTION('',(0.705516335778305,-0.29632993142808,-0.64376647294635));
#39665=DIRECTION('',(0.,0.921488728241605,0.388405102597364));
#39666=DIRECTION('',(-0.705516335778301,-0.667744245837284,0.237411714330098));
#39667=DIRECTION('center_axis',(0.561006631580402,-0.79102610982797,-0.244027156056943));
#39668=DIRECTION('ref_axis',(-0.398879012810071,0.,-0.917003562228448));
#39669=DIRECTION('',(0.705516335778309,0.611085652157592,-0.358916460582513));
#39670=DIRECTION('',(0.,-0.294785966455749,0.955563307154869));
#39671=DIRECTION('',(-0.705516335778301,-0.302676520965596,-0.640807009641845));
#39672=DIRECTION('center_axis',(-0.56100663158041,-0.321526135468408,0.762818788136182));
#39673=DIRECTION('ref_axis',(0.805595332751393,0.,0.592466167683162));
#39674=DIRECTION('',(0.,-0.921488728241605,-0.388405102597364));
#39675=DIRECTION('',(0.705516335778301,0.296329931428102,0.643766472946344));
#39676=DIRECTION('',(-0.705516335778315,0.667744245837269,-0.237411714330102));
#39677=DIRECTION('center_axis',(-0.70710678118655,0.233585577946046,0.667411250860823));
#39678=DIRECTION('ref_axis',(0.686399640790371,0.,0.727224541062009));
#39679=DIRECTION('',(0.,-0.943862042647771,0.330339892306057));
#39680=DIRECTION('',(0.,0.943862042647771,-0.330339892306057));
#39681=DIRECTION('center_axis',(-0.5610066315804,-0.791026109827971,-0.244027156056943));
#39682=DIRECTION('ref_axis',(-0.398879012810073,0.,0.917003562228447));
#39683=DIRECTION('',(0.705516335778317,-0.611085652157596,0.35891646058249));
#39684=DIRECTION('',(-0.705516335778303,0.302676520965595,0.640807009641843));
#39685=DIRECTION('',(0.,0.294785966455749,-0.955563307154869));
#39686=DIRECTION('center_axis',(-0.707106781186551,-0.361120764691831,-0.607940616597034));
#39687=DIRECTION('ref_axis',(-0.651933718094179,0.,0.758275957163288));
#39688=DIRECTION('',(0.,-0.859757865108992,0.510701883081733));
#39689=DIRECTION('',(0.,0.859757865108992,-0.510701883081733));
#39690=DIRECTION('center_axis',(0.,-0.955563307154869,-0.294785966455749));
#39691=DIRECTION('ref_axis',(0.,0.294785966455749,-0.955563307154869));
#39692=DIRECTION('',(-1.,0.,0.));
#39693=DIRECTION('',(1.,0.,0.));
#39694=DIRECTION('center_axis',(-0.707106781186538,-0.640856382055797,0.298836238730124));
#39695=DIRECTION('ref_axis',(0.389281620635034,0.,0.921118787038763));
#39696=DIRECTION('',(0.,0.422618261740699,0.90630778703665));
#39697=DIRECTION('',(0.,-0.422618261740699,-0.90630778703665));
#39698=DIRECTION('center_axis',(0.,-0.388405102597364,0.921488728241605));
#39699=DIRECTION('ref_axis',(1.,0.,0.));
#39700=DIRECTION('',(-1.,0.,0.));
#39701=DIRECTION('',(1.,0.,0.));
#39702=DIRECTION('center_axis',(0.707106781186553,-0.36112076469183,-0.607940616597033));
#39703=DIRECTION('ref_axis',(-0.651933718094177,0.,-0.758275957163289));
#39704=DIRECTION('',(0.,-0.859757865108992,0.510701883081733));
#39705=DIRECTION('',(0.,0.859757865108992,-0.510701883081733));
#39706=DIRECTION('center_axis',(0.707106781186554,-0.640856382055783,0.298836238730117));
#39707=DIRECTION('ref_axis',(0.389281620635019,0.,-0.921118787038769));
#39708=DIRECTION('',(0.,0.422618261740699,0.90630778703665));
#39709=DIRECTION('',(0.,-0.422618261740699,-0.90630778703665));
#39710=DIRECTION('center_axis',(0.707106781186551,0.233585577946046,0.667411250860822));
#39711=DIRECTION('ref_axis',(0.68639964079037,0.,-0.72722454106201));
#39712=DIRECTION('',(0.,-0.943862042647771,0.330339892306057));
#39713=DIRECTION('',(0.,0.943862042647771,-0.330339892306057));
#39714=DIRECTION('center_axis',(1.,0.,0.));
#39715=DIRECTION('ref_axis',(0.,0.90630778703665,-0.422618261740699));
#39716=DIRECTION('center_axis',(0.,0.330339892306057,0.943862042647771));
#39717=DIRECTION('ref_axis',(0.,-0.943862042647771,0.330339892306057));
#39718=DIRECTION('center_axis',(0.,-0.90630778703665,0.422618261740699));
#39719=DIRECTION('ref_axis',(0.,-0.422618261740699,-0.90630778703665));
#39720=DIRECTION('center_axis',(0.561006631580401,-0.386786669513441,0.731893183196504));
#39721=DIRECTION('ref_axis',(0.793664727118314,0.,-0.60835540675514));
#39722=DIRECTION('',(0.70551633577831,-0.23909436146888,-0.667143602430344));
#39723=DIRECTION('',(0.,0.884130450221741,0.467240138462762));
#39724=DIRECTION('',(-0.705516335778305,-0.685895071683811,0.178310545369065));
#39725=DIRECTION('center_axis',(0.561006631580418,-0.766747648626013,-0.312041027189173));
#39726=DIRECTION('ref_axis',(-0.486084108127403,0.,-0.873912032086747));
#39727=DIRECTION('',(0.705516335778306,0.640041917465772,-0.304291051193904));
#39728=DIRECTION('',(0.,-0.376947046632555,0.926234810420659));
#39729=DIRECTION('',(-0.705516335778304,-0.245674734539573,-0.66474854250225));
#39730=DIRECTION('center_axis',(-0.561006631580399,-0.386786669513442,0.731893183196506));
#39731=DIRECTION('ref_axis',(0.793664727118316,0.,0.608355406755138));
#39732=DIRECTION('',(0.,-0.884130450221741,-0.467240138462762));
#39733=DIRECTION('',(0.705516335778311,0.239094361468879,0.667143602430342));
#39734=DIRECTION('',(-0.705516335778307,0.68589507168381,-0.178310545369064));
#39735=DIRECTION('center_axis',(-0.707106781186539,0.174527991013632,0.685229874095371));
#39736=DIRECTION('ref_axis',(0.695910561235553,0.,0.718128463967846));
#39737=DIRECTION('',(0.,-0.96906138128887,0.246819851905204));
#39738=DIRECTION('',(0.,0.96906138128887,-0.246819851905204));
#39739=DIRECTION('center_axis',(-0.561006631580416,-0.766747648626014,-0.312041027189174));
#39740=DIRECTION('ref_axis',(-0.486084108127405,0.,0.873912032086746));
#39741=DIRECTION('',(0.705516335778307,-0.640041917465771,0.304291051193903));
#39742=DIRECTION('',(-0.705516335778305,0.245674734539572,0.664748542502249));
#39743=DIRECTION('',(0.,0.376947046632555,-0.926234810420659));
#39744=DIRECTION('center_axis',(-0.707106781186547,-0.306761075170857,-0.637100967476915));
#39745=DIRECTION('ref_axis',(-0.669373784875801,0.,0.742925794491647));
#39746=DIRECTION('',(0.,-0.900996828806872,0.433825672914778));
#39747=DIRECTION('',(0.,0.900996828806872,-0.433825672914778));
#39748=DIRECTION('center_axis',(0.,-0.926234810420659,-0.376947046632555));
#39749=DIRECTION('ref_axis',(0.,0.376947046632555,-0.926234810420659));
#39750=DIRECTION('',(-1.,0.,0.));
#39751=DIRECTION('',(1.,0.,0.));
#39752=DIRECTION('center_axis',(-0.70710678118655,-0.664463024388673,0.241844762647975));
#39753=DIRECTION('ref_axis',(0.323615577118183,0.,0.946188648339466));
#39754=DIRECTION('',(0.,0.342020143325669,0.939692620785908));
#39755=DIRECTION('',(0.,-0.342020143325669,-0.939692620785908));
#39756=DIRECTION('center_axis',(0.,-0.467240138462762,0.884130450221741));
#39757=DIRECTION('ref_axis',(1.,0.,0.));
#39758=DIRECTION('',(-1.,0.,0.));
#39759=DIRECTION('',(1.,0.,0.));
#39760=DIRECTION('center_axis',(0.707106781186549,-0.306761075170856,-0.637100967476913));
#39761=DIRECTION('ref_axis',(-0.669373784875799,0.,-0.742925794491649));
#39762=DIRECTION('',(0.,-0.900996828806872,0.433825672914778));
#39763=DIRECTION('',(0.,0.900996828806872,-0.433825672914778));
#39764=DIRECTION('center_axis',(0.707106781186551,-0.664463024388671,0.241844762647974));
#39765=DIRECTION('ref_axis',(0.323615577118182,0.,-0.946188648339466));
#39766=DIRECTION('',(0.,0.342020143325669,0.939692620785908));
#39767=DIRECTION('',(0.,-0.342020143325669,-0.939692620785908));
#39768=DIRECTION('center_axis',(0.70710678118654,0.174527991013631,0.68522987409537));
#39769=DIRECTION('ref_axis',(0.695910561235551,0.,-0.718128463967847));
#39770=DIRECTION('',(0.,-0.96906138128887,0.246819851905204));
#39771=DIRECTION('',(0.,0.96906138128887,-0.246819851905204));
#39772=DIRECTION('center_axis',(1.,0.,0.));
#39773=DIRECTION('ref_axis',(0.,0.939692620785908,-0.342020143325669));
#39774=DIRECTION('center_axis',(0.,0.246819851905204,0.96906138128887));
#39775=DIRECTION('ref_axis',(0.,-0.96906138128887,0.246819851905204));
#39776=DIRECTION('center_axis',(0.,-0.939692620785908,0.342020143325669));
#39777=DIRECTION('ref_axis',(0.,-0.342020143325669,-0.939692620785908));
#39778=DIRECTION('center_axis',(0.707106781186548,0.114142140686716,0.697833484234924));
#39779=DIRECTION('ref_axis',(0.702424227635742,0.,-0.711758529580314));
#39780=DIRECTION('',(0.595596683047422,0.43579678841082,-0.674793116705946));
#39781=DIRECTION('',(0.,0.986885577683101,-0.161421363397451));
#39782=DIRECTION('',(0.,-0.986885577683101,0.161421363397451));
#39783=DIRECTION('',(0.557191914001245,-0.697558392670361,-0.450499122958937));
#39784=DIRECTION('center_axis',(1.,0.,0.));
#39785=DIRECTION('ref_axis',(0.,0.965925826289068,-0.258819045102521));
#39786=DIRECTION('',(0.,0.258819045102521,0.965925826289068));
#39787=DIRECTION('',(0.,-0.935378662600772,0.353647787425838));
#39788=DIRECTION('center_axis',(0.707106781186552,-0.683012701892215,0.183012701892218));
#39789=DIRECTION('ref_axis',(0.250562807085728,0.,-0.968100345886376));
#39790=DIRECTION('',(0.557191914001229,0.69755839267037,0.450499122958943));
#39791=DIRECTION('',(0.,-0.258819045102521,-0.965925826289068));
#39792=DIRECTION('',(0.705516335778306,0.664127077314135,-0.2473498031698));
#39793=DIRECTION('center_axis',(0.,-0.542519194747167,0.840043405623117));
#39794=DIRECTION('ref_axis',(1.,0.,0.));
#39795=DIRECTION('',(-1.,0.,0.));
#39796=DIRECTION('',(0.,-0.840043405623117,-0.542519194747167));
#39797=DIRECTION('',(1.,0.,0.));
#39798=DIRECTION('center_axis',(0.561006631580396,-0.736633774843142,-0.37768007768899));
#39799=DIRECTION('ref_axis',(-0.558457227212258,0.,-0.829533317820566));
#39800=DIRECTION('',(0.,-0.456239332177649,0.889857107503274));
#39801=DIRECTION('',(-0.705516335778303,-0.186803215041171,-0.683630937568099));
#39802=DIRECTION('center_axis',(-0.561006631580404,-0.4491035234553,0.695397429203505));
#39803=DIRECTION('ref_axis',(0.778302413620333,0.,0.627889602520032));
#39804=DIRECTION('',(0.705516335778306,0.180039139049759,0.685443366267538));
#39805=DIRECTION('',(-0.705516335778306,0.69882582188005,-0.117852325490948));
#39806=DIRECTION('center_axis',(-0.707106781186546,0.114142140686716,0.697833484234925));
#39807=DIRECTION('ref_axis',(0.702424227635744,0.,0.711758529580313));
#39808=DIRECTION('',(0.,-0.986885577683101,0.161421363397451));
#39809=DIRECTION('',(0.,0.986885577683101,-0.161421363397451));
#39810=DIRECTION('center_axis',(-0.561006631580394,-0.736633774843143,-0.37768007768899));
#39811=DIRECTION('ref_axis',(-0.55845722721226,0.,0.829533317820565));
#39812=DIRECTION('',(0.705516335778307,-0.664127077314133,0.247349803169799));
#39813=DIRECTION('',(-0.705516335778305,0.18680321504117,0.683630937568098));
#39814=DIRECTION('',(0.,0.456239332177649,-0.889857107503274));
#39815=DIRECTION('center_axis',(-0.707106781186544,-0.25006674864043,-0.661412595302213));
#39816=DIRECTION('ref_axis',(-0.683116152038589,0.,0.730309744439982));
#39817=DIRECTION('',(0.,-0.935378662600772,0.353647787425838));
#39818=DIRECTION('',(0.,0.935378662600772,-0.353647787425838));
#39819=DIRECTION('center_axis',(0.,-0.889857107503274,-0.456239332177649));
#39820=DIRECTION('ref_axis',(0.,0.456239332177649,-0.889857107503274));
#39821=DIRECTION('',(-1.,0.,0.));
#39822=DIRECTION('',(1.,0.,0.));
#39823=DIRECTION('center_axis',(-0.707106781186551,-0.683012701892216,0.183012701892218));
#39824=DIRECTION('ref_axis',(0.250562807085729,0.,0.968100345886375));
#39825=DIRECTION('',(0.,0.258819045102521,0.965925826289068));
#39826=DIRECTION('',(0.,-0.258819045102521,-0.965925826289068));
#39827=DIRECTION('center_axis',(0.707106781186545,-0.25006674864043,-0.661412595302212));
#39828=DIRECTION('ref_axis',(-0.683116152038587,0.,-0.730309744439983));
#39829=DIRECTION('',(0.,0.935378662600772,-0.353647787425838));
#39830=DIRECTION('center_axis',(0.,0.161421363397451,0.986885577683101));
#39831=DIRECTION('ref_axis',(0.,-0.986885577683101,0.161421363397451));
#39832=DIRECTION('center_axis',(0.,-0.965925826289068,0.258819045102521));
#39833=DIRECTION('ref_axis',(0.,-0.258819045102521,-0.965925826289068));
#39834=DIRECTION('center_axis',(0.561006631580396,-0.508002428407528,0.653609280881837));
#39835=DIRECTION('ref_axis',(0.758814655754537,0.,-0.651306623804889));
#39836=DIRECTION('',(0.705516335778306,-0.119613710071895,-0.698526492205406));
#39837=DIRECTION('',(0.,0.789563123475645,0.613669352377469));
#39838=DIRECTION('',(-0.70551633577831,-0.706438085609211,0.0564971782546713));
#39839=DIRECTION('center_axis',(0.56100663158039,-0.700913673242072,-0.44044475474812));
#39840=DIRECTION('ref_axis',(-0.617521420133027,0.,-0.786554064052109));
#39841=DIRECTION('',(0.70551633577831,0.683157829093258,-0.188526073789633));
#39842=DIRECTION('',(0.,-0.532059360920026,0.846707054687377));
#39843=DIRECTION('',(-0.705516335778307,-0.126510010281474,-0.697310488411391));
#39844=DIRECTION('center_axis',(-0.561006631580394,-0.508002428407529,0.653609280881838));
#39845=DIRECTION('ref_axis',(0.758814655754539,0.,0.651306623804887));
#39846=DIRECTION('',(0.,-0.789563123475645,-0.613669352377469));
#39847=DIRECTION('',(0.705516335778308,0.119613710071895,0.698526492205404));
#39848=DIRECTION('',(-0.705516335778312,0.70643808560921,-0.0564971782546712));
#39849=DIRECTION('center_axis',(-0.707106781186545,0.0528875997482675,0.705126160196082));
#39850=DIRECTION('ref_axis',(0.706114387365564,0.,0.708097784176278));
#39851=DIRECTION('',(0.,-0.997198978933359,0.0747943608453595));
#39852=DIRECTION('',(0.,0.997198978933359,-0.0747943608453595));
#39853=DIRECTION('center_axis',(-0.561006631580388,-0.700913673242073,-0.44044475474812));
#39854=DIRECTION('ref_axis',(-0.617521420133029,0.,0.786554064052108));
#39855=DIRECTION('',(0.705516335778312,-0.683157829093257,0.188526073789632));
#39856=DIRECTION('',(-0.705516335778309,0.126510010281474,0.697310488411389));
#39857=DIRECTION('',(0.,0.532059360920026,-0.846707054687377));
#39858=DIRECTION('center_axis',(-0.707106781186544,-0.191469263158417,-0.680690473905414));
#39859=DIRECTION('ref_axis',(-0.693521587324702,0.,0.720435845800739));
#39860=DIRECTION('',(0.,-0.962641699975202,0.270778428736215));
#39861=DIRECTION('',(0.,0.962641699975202,-0.270778428736215));
#39862=DIRECTION('center_axis',(0.,-0.846707054687377,-0.532059360920026));
#39863=DIRECTION('ref_axis',(-1.,0.,0.));
#39864=DIRECTION('',(-1.,0.,0.));
#39865=DIRECTION('',(1.,0.,0.));
#39866=DIRECTION('center_axis',(-0.707106781186541,-0.696364240320026,0.122787803968974));
#39867=DIRECTION('ref_axis',(0.171087869746039,0.,0.985255774317391));
#39868=DIRECTION('',(0.,0.17364817766693,0.984807753012208));
#39869=DIRECTION('',(0.,-0.17364817766693,-0.984807753012208));
#39870=DIRECTION('center_axis',(0.,-0.61366935237747,0.789563123475645));
#39871=DIRECTION('ref_axis',(1.,0.,0.));
#39872=DIRECTION('',(-1.,0.,0.));
#39873=DIRECTION('',(1.,0.,0.));
#39874=DIRECTION('center_axis',(0.707106781186546,-0.191469263158417,-0.680690473905413));
#39875=DIRECTION('ref_axis',(-0.6935215873247,0.,-0.72043584580074));
#39876=DIRECTION('',(0.,-0.962641699975202,0.270778428736215));
#39877=DIRECTION('',(0.,0.962641699975202,-0.270778428736215));
#39878=DIRECTION('center_axis',(0.707106781186543,-0.696364240320024,0.122787803968974));
#39879=DIRECTION('ref_axis',(0.171087869746038,0.,-0.985255774317391));
#39880=DIRECTION('',(0.,0.17364817766693,0.984807753012208));
#39881=DIRECTION('',(0.,-0.17364817766693,-0.984807753012208));
#39882=DIRECTION('center_axis',(0.707106781186546,0.0528875997482674,0.705126160196081));
#39883=DIRECTION('ref_axis',(0.706114387365562,0.,-0.708097784176279));
#39884=DIRECTION('',(0.,-0.997198978933359,0.0747943608453595));
#39885=DIRECTION('',(0.,0.997198978933359,-0.0747943608453595));
#39886=DIRECTION('center_axis',(1.,0.,0.));
#39887=DIRECTION('ref_axis',(0.,0.984807753012208,-0.17364817766693));
#39888=DIRECTION('center_axis',(0.,0.0747943608453595,0.997198978933359));
#39889=DIRECTION('ref_axis',(0.,-0.997198978933359,0.0747943608453595));
#39890=DIRECTION('center_axis',(0.,-0.984807753012208,0.17364817766693));
#39891=DIRECTION('ref_axis',(0.,-0.17364817766693,-0.984807753012208));
#39892=DIRECTION('center_axis',(0.561006631580394,-0.659859195364386,-0.499857381275785));
#39893=DIRECTION('ref_axis',(-0.665244232298936,0.,-0.746625817523744));
#39894=DIRECTION('',(0.705516335778315,0.696989337290999,-0.128267547152788));
#39895=DIRECTION('',(0.,-0.603830096659559,0.797113049929624));
#39896=DIRECTION('',(-0.705516335778306,-0.0652539879547271,-0.705683085390288));
#39897=DIRECTION('center_axis',(0.,-0.797113049929624,-0.603830096659559));
#39898=DIRECTION('ref_axis',(-1.,0.,0.));
#39899=DIRECTION('',(0.557191914001245,0.501410699557118,-0.661909722954173));
#39900=DIRECTION('',(1.,0.,0.));
#39901=DIRECTION('',(-1.,0.,0.));
#39902=DIRECTION('',(-0.557191914001234,0.501410699557122,-0.66190972295418));
#39903=DIRECTION('center_axis',(0.707106781186545,-0.131414580971466,-0.694787886990049));
#39904=DIRECTION('ref_axis',(-0.700866150214856,0.,-0.713292814686232));
#39905=DIRECTION('',(0.,-0.982578452753869,0.185848282703424));
#39906=DIRECTION('',(0.,0.982578452753869,-0.185848282703424));
#39907=DIRECTION('center_axis',(0.561006631580395,-0.563035128139337,0.606846771272568));
#39908=DIRECTION('ref_axis',(0.734296425103064,0.,-0.678828962317357));
#39909=DIRECTION('',(0.705516335778303,-0.0582779485356275,-0.706293409755772));
#39910=DIRECTION('',(0.,0.733073789207257,0.680149115692518));
#39911=DIRECTION('',(-0.705516335778312,-0.708673928947909,-0.00528794662206119));
#39912=DIRECTION('center_axis',(0.,-0.680149115692518,0.733073789207257));
#39913=DIRECTION('ref_axis',(1.,0.,0.));
#39914=DIRECTION('',(0.557191914001236,-0.608732561538147,-0.564784772718639));
#39915=DIRECTION('',(1.,0.,0.));
#39916=DIRECTION('',(-1.,0.,0.));
#39917=DIRECTION('',(-0.55719191400124,-0.608732561538145,-0.564784772718638));
#39918=DIRECTION('center_axis',(0.707106781186545,-0.704416026402761,0.0616284167162197));
#39919=DIRECTION('ref_axis',(0.0868265938642484,0.,-0.996223440096615));
#39920=DIRECTION('',(0.,0.0871557427476584,0.996194698091746));
#39921=DIRECTION('',(0.,-0.0871557427476584,-0.996194698091746));
#39922=DIRECTION('center_axis',(0.707106781186549,-0.00876944775867117,
0.707052400311324));
#39923=DIRECTION('ref_axis',(0.70707958918054,0.,-0.707133972146918));
#39924=DIRECTION('',(0.,-0.999923093828728,-0.0124018719548351));
#39925=DIRECTION('',(0.,0.999923093828728,0.0124018719548351));
#39926=DIRECTION('center_axis',(-0.707106781186545,-0.131414580971466,-0.694787886990049));
#39927=DIRECTION('ref_axis',(-0.700866150214856,0.,0.713292814686232));
#39928=DIRECTION('',(-0.59559668304743,0.640307864722775,0.485046832292573));
#39929=DIRECTION('',(0.,0.982578452753869,-0.185848282703424));
#39930=DIRECTION('',(0.,-0.982578452753869,0.185848282703424));
#39931=DIRECTION('center_axis',(0.,-0.996194698091746,0.0871557427476584));
#39932=DIRECTION('ref_axis',(0.,-0.0871557427476584,-0.996194698091746));
#39933=DIRECTION('',(0.,0.0871557427476584,0.996194698091746));
#39934=DIRECTION('center_axis',(-0.707106781186556,-0.70441602640275,0.0616284167162188));
#39935=DIRECTION('ref_axis',(0.0868265938642457,0.,0.996223440096615));
#39936=DIRECTION('',(0.595596683047425,-0.546352650982967,0.588866174870648));
#39937=DIRECTION('',(0.,-0.0871557427476584,-0.996194698091746));
#39938=DIRECTION('center_axis',(-0.707106781186548,-0.00876944775867119,
0.707052400311326));
#39939=DIRECTION('ref_axis',(0.707079589180542,0.,0.707133972146916));
#39940=DIRECTION('',(0.,0.999923093828728,0.0124018719548351));
#39941=DIRECTION('',(0.,-0.999923093828728,-0.0124018719548351));
#39942=DIRECTION('center_axis',(0.,-0.0124018719548351,0.999923093828728));
#39943=DIRECTION('ref_axis',(0.,-0.999923093828728,-0.0124018719548351));
#39944=DIRECTION('center_axis',(0.,-0.185848282703424,-0.982578452753869));
#39945=DIRECTION('ref_axis',(0.,0.982578452753869,-0.185848282703424));
#39946=DIRECTION('center_axis',(0.561006631580415,-0.613782790576089,0.555465791309803));
#39947=DIRECTION('ref_axis',(0.703588880269149,0.,-0.710607266752603));
#39948=DIRECTION('',(0.705516335778305,0.00350134337823142,-0.708685007986272));
#39949=DIRECTION('',(0.,0.671005320760942,0.741452533551882));
#39950=DIRECTION('',(-0.705516335778299,-0.705516335778311,-0.067032827032045));
#39951=DIRECTION('center_axis',(0.561006631580416,-0.613782790576088,-0.555465791309803));
#39952=DIRECTION('ref_axis',(-0.703588880269148,0.,-0.710607266752604));
#39953=DIRECTION('',(0.705516335778299,0.705516335778311,-0.0670328270320441));
#39954=DIRECTION('',(0.,-0.671005320760943,0.741452533551882));
#39955=DIRECTION('',(-0.705516335778305,-0.00350134337823142,-0.708685007986272));
#39956=DIRECTION('center_axis',(-0.561006631580427,-0.613782790576083,0.555465791309797));
#39957=DIRECTION('ref_axis',(0.703588880269137,0.,0.710607266752615));
#39958=DIRECTION('',(0.,-0.671005320760942,-0.741452533551882));
#39959=DIRECTION('',(0.705516335778308,-0.00350134337825648,0.708685007986269));
#39960=DIRECTION('',(-0.705516335778288,0.705516335778322,0.0670328270320461));
#39961=DIRECTION('center_axis',(-0.707106781186547,-0.0703597544730291,
0.703597544730292));
#39962=DIRECTION('ref_axis',(0.705345615858599,0.,0.708863570928182));
#39963=DIRECTION('',(0.,-0.995037190209989,-0.0995037190209987));
#39964=DIRECTION('',(0.,0.995037190209989,0.0995037190209987));
#39965=DIRECTION('center_axis',(-0.561006631580428,-0.613782790576082,-0.555465791309797));
#39966=DIRECTION('ref_axis',(-0.703588880269137,0.,0.710607266752615));
#39967=DIRECTION('',(0.705516335778288,-0.705516335778322,0.0670328270320439));
#39968=DIRECTION('',(-0.705516335778307,0.00350134337825647,0.708685007986269));
#39969=DIRECTION('',(0.,0.671005320760943,-0.741452533551882));
#39970=DIRECTION('center_axis',(-0.707106781186548,-0.0703597544730291,
-0.703597544730292));
#39971=DIRECTION('ref_axis',(-0.705345615858598,0.,0.708863570928183));
#39972=DIRECTION('',(0.,-0.995037190209989,0.0995037190209988));
#39973=DIRECTION('',(0.,0.995037190209989,-0.0995037190209988));
#39974=DIRECTION('center_axis',(0.,-0.741452533551882,-0.671005320760943));
#39975=DIRECTION('ref_axis',(-1.,0.,0.));
#39976=DIRECTION('',(-1.,0.,0.));
#39977=DIRECTION('',(1.,0.,0.));
#39978=DIRECTION('center_axis',(-0.707106781186565,-0.70710678118653,4.32978028117736E-17));
#39979=DIRECTION('ref_axis',(6.12323399573647E-17,0.,1.));
#39980=DIRECTION('',(0.,6.12323399573677E-17,1.));
#39981=DIRECTION('',(0.,-6.12323399573677E-17,-1.));
#39982=DIRECTION('center_axis',(0.,-0.741452533551882,0.671005320760942));
#39983=DIRECTION('ref_axis',(1.,0.,0.));
#39984=DIRECTION('',(-1.,0.,0.));
#39985=DIRECTION('',(1.,0.,0.));
#39986=DIRECTION('center_axis',(0.707106781186548,-0.070359754473029,-0.703597544730291));
#39987=DIRECTION('ref_axis',(-0.705345615858597,0.,-0.708863570928184));
#39988=DIRECTION('',(0.,-0.995037190209989,0.0995037190209988));
#39989=DIRECTION('',(0.,0.995037190209989,-0.0995037190209988));
#39990=DIRECTION('center_axis',(0.707106781186554,-0.707106781186541,4.32978028117743E-17));
#39991=DIRECTION('ref_axis',(6.12323399573666E-17,0.,-1.));
#39992=DIRECTION('',(0.,6.12323399573677E-17,1.));
#39993=DIRECTION('',(0.,-6.12323399573677E-17,-1.));
#39994=DIRECTION('center_axis',(0.707106781186548,-0.070359754473029,0.703597544730291));
#39995=DIRECTION('ref_axis',(0.705345615858597,0.,-0.708863570928184));
#39996=DIRECTION('',(0.,-0.995037190209989,-0.0995037190209987));
#39997=DIRECTION('',(0.,0.995037190209989,0.0995037190209987));
#39998=DIRECTION('center_axis',(1.,0.,0.));
#39999=DIRECTION('ref_axis',(0.,1.,-6.12323399573677E-17));
#40000=DIRECTION('center_axis',(0.,-0.0995037190209987,0.995037190209989));
#40001=DIRECTION('ref_axis',(0.,-0.995037190209989,-0.0995037190209987));
#40002=DIRECTION('center_axis',(0.,-1.,6.12323399573677E-17));
#40003=DIRECTION('ref_axis',(0.,-6.12323399573677E-17,-1.));
#40004=DIRECTION('center_axis',(0.56100663158041,-0.65985919536438,0.499857381275775));
#40005=DIRECTION('ref_axis',(0.665244232298917,0.,-0.746625817523761));
#40006=DIRECTION('',(0.705516335778303,0.0652539879547519,-0.705683085390289));
#40007=DIRECTION('',(0.,0.603830096659555,0.797113049929628));
#40008=DIRECTION('',(-0.705516335778303,-0.696989337291012,-0.128267547152789));
#40009=DIRECTION('center_axis',(0.56100663158041,-0.56303512813933,-0.60684677127256));
#40010=DIRECTION('ref_axis',(-0.734296425103051,0.,-0.678828962317372));
#40011=DIRECTION('',(0.7055163357783,0.708673928947921,-0.00528794662205797));
#40012=DIRECTION('',(0.,-0.733073789207257,0.680149115692518));
#40013=DIRECTION('',(-0.705516335778302,0.0582779485356024,-0.706293409755775));
#40014=DIRECTION('center_axis',(-0.561006631580394,-0.659859195364389,0.499857381275781));
#40015=DIRECTION('ref_axis',(0.665244232298933,0.,0.746625817523747));
#40016=DIRECTION('',(0.,-0.603830096659555,-0.797113049929628));
#40017=DIRECTION('',(0.705516335778303,-0.0652539879547265,0.705683085390291));
#40018=DIRECTION('',(-0.705516335778317,0.696989337290998,0.128267547152788));
#40019=DIRECTION('center_axis',(-0.707106781186548,-0.131414580971466,0.694787886990046));
#40020=DIRECTION('ref_axis',(0.700866150214853,0.,0.713292814686235));
#40021=DIRECTION('',(0.,-0.98257845275387,-0.185848282703424));
#40022=DIRECTION('',(0.,0.98257845275387,0.185848282703424));
#40023=DIRECTION('center_axis',(-0.561006631580395,-0.563035128139337,-0.606846771272568));
#40024=DIRECTION('ref_axis',(-0.734296425103064,0.,0.678828962317357));
#40025=DIRECTION('',(0.705516335778314,-0.708673928947907,0.00528794662205805));
#40026=DIRECTION('',(-0.705516335778303,-0.0582779485356272,0.706293409755772));
#40027=DIRECTION('',(0.,0.733073789207257,-0.680149115692518));
#40028=DIRECTION('center_axis',(-0.707106781186548,-0.00876944775867143,
-0.707052400311326));
#40029=DIRECTION('ref_axis',(-0.707079589180542,0.,0.707133972146916));
#40030=DIRECTION('',(0.,-0.999923093828728,0.0124018719548355));
#40031=DIRECTION('',(0.,0.999923093828728,-0.0124018719548355));
#40032=DIRECTION('center_axis',(0.,-0.680149115692518,-0.733073789207257));
#40033=DIRECTION('ref_axis',(-1.,0.,0.));
#40034=DIRECTION('',(-1.,0.,0.));
#40035=DIRECTION('',(1.,0.,0.));
#40036=DIRECTION('center_axis',(-0.707106781186531,-0.704416026402775,-0.0616284167162207));
#40037=DIRECTION('ref_axis',(-0.0868265938642515,0.,0.996223440096614));
#40038=DIRECTION('',(0.,-0.087155742747658,0.996194698091746));
#40039=DIRECTION('',(0.,0.087155742747658,-0.996194698091746));
#40040=DIRECTION('center_axis',(0.,-0.797113049929628,0.603830096659555));
#40041=DIRECTION('ref_axis',(1.,0.,0.));
#40042=DIRECTION('',(-1.,0.,0.));
#40043=DIRECTION('',(1.,0.,0.));
#40044=DIRECTION('center_axis',(0.707106781186549,-0.00876944775867141,
-0.707052400311324));
#40045=DIRECTION('ref_axis',(-0.70707958918054,0.,-0.707133972146918));
#40046=DIRECTION('',(0.,-0.999923093828728,0.0124018719548355));
#40047=DIRECTION('',(0.,0.999923093828728,-0.0124018719548355));
#40048=DIRECTION('center_axis',(0.707106781186545,-0.704416026402761,-0.0616284167162195));
#40049=DIRECTION('ref_axis',(-0.0868265938642481,0.,-0.996223440096615));
#40050=DIRECTION('',(0.,-0.087155742747658,0.996194698091746));
#40051=DIRECTION('',(0.,0.087155742747658,-0.996194698091746));
#40052=DIRECTION('center_axis',(0.707106781186549,-0.131414580971465,0.694787886990045));
#40053=DIRECTION('ref_axis',(0.700866150214851,0.,-0.713292814686237));
#40054=DIRECTION('',(0.,-0.98257845275387,-0.185848282703424));
#40055=DIRECTION('',(0.,0.98257845275387,0.185848282703424));
#40056=DIRECTION('center_axis',(1.,0.,0.));
#40057=DIRECTION('ref_axis',(0.,0.996194698091746,0.087155742747658));
#40058=DIRECTION('center_axis',(0.,-0.185848282703424,0.98257845275387));
#40059=DIRECTION('ref_axis',(0.,-0.98257845275387,-0.185848282703424));
#40060=DIRECTION('center_axis',(0.,-0.996194698091746,-0.087155742747658));
#40061=DIRECTION('ref_axis',(0.,0.087155742747658,-0.996194698091746));
#40062=DIRECTION('center_axis',(0.707106781186546,-0.191469263158417,0.680690473905413));
#40063=DIRECTION('ref_axis',(0.6935215873247,0.,-0.72043584580074));
#40064=DIRECTION('',(0.595596683047428,0.680145916919136,-0.427394575118975));
#40065=DIRECTION('',(0.,0.962641699975202,0.270778428736215));
#40066=DIRECTION('',(0.,-0.962641699975202,-0.270778428736215));
#40067=DIRECTION('',(0.557191914001241,-0.441813446929312,-0.703091778563846));
#40068=DIRECTION('center_axis',(1.,0.,0.));
#40069=DIRECTION('ref_axis',(0.,0.984807753012208,0.17364817766693));
#40070=DIRECTION('',(0.,-0.17364817766693,0.984807753012208));
#40071=DIRECTION('',(0.,-0.997198978933359,-0.0747943608453594));
#40072=DIRECTION('center_axis',(0.707106781186543,-0.696364240320023,-0.122787803968974));
#40073=DIRECTION('ref_axis',(-0.171087869746038,0.,-0.985255774317392));
#40074=DIRECTION('',(0.557191914001248,0.44181344692931,0.703091778563843));
#40075=DIRECTION('',(0.,0.17364817766693,-0.984807753012208));
#40076=DIRECTION('',(0.70551633577831,0.706438085609211,0.0564971782546651));
#40077=DIRECTION('center_axis',(0.,-0.846707054687383,0.532059360920017));
#40078=DIRECTION('ref_axis',(1.,0.,0.));
#40079=DIRECTION('',(-1.,0.,0.));
#40080=DIRECTION('',(0.,-0.532059360920017,-0.846707054687383));
#40081=DIRECTION('',(1.,0.,0.));
#40082=DIRECTION('center_axis',(0.5610066315804,-0.508002428407545,-0.65360928088182));
#40083=DIRECTION('ref_axis',(-0.758814655754527,0.,-0.651306623804901));
#40084=DIRECTION('',(0.,-0.789563123475628,0.613669352377492));
#40085=DIRECTION('',(-0.705516335778305,0.11961371007187,-0.698526492205411));
#40086=DIRECTION('center_axis',(-0.561006631580394,-0.700913673242075,0.440444754748109));
#40087=DIRECTION('ref_axis',(0.617521420133015,0.,0.786554064052119));
#40088=DIRECTION('',(0.705516335778313,-0.1265100102815,0.697310488411381));
#40089=DIRECTION('',(-0.70551633577831,0.683157829093255,0.188526073789644));
#40090=DIRECTION('center_axis',(-0.707106781186538,-0.191469263158419,0.68069047390542));
#40091=DIRECTION('ref_axis',(0.693521587324708,0.,0.720435845800733));
#40092=DIRECTION('',(0.,-0.962641699975202,-0.270778428736215));
#40093=DIRECTION('',(0.,0.962641699975202,0.270778428736215));
#40094=DIRECTION('center_axis',(-0.561006631580398,-0.508002428407546,-0.653609280881821));
#40095=DIRECTION('ref_axis',(-0.758814655754528,0.,0.651306623804899));
#40096=DIRECTION('',(0.705516335778312,-0.70643808560921,-0.056497178254665));
#40097=DIRECTION('',(-0.705516335778307,-0.119613710071869,0.69852649220541));
#40098=DIRECTION('',(0.,0.789563123475628,-0.613669352377492));
#40099=DIRECTION('center_axis',(-0.707106781186548,0.0528875997482672,-0.705126160196079));
#40100=DIRECTION('ref_axis',(-0.706114387365561,0.,0.708097784176281));
#40101=DIRECTION('',(0.,-0.997198978933359,-0.0747943608453594));
#40102=DIRECTION('',(0.,0.997198978933359,0.0747943608453594));
#40103=DIRECTION('center_axis',(0.,-0.613669352377492,-0.789563123475628));
#40104=DIRECTION('ref_axis',(-1.,0.,0.));
#40105=DIRECTION('',(-1.,0.,0.));
#40106=DIRECTION('',(1.,0.,0.));
#40107=DIRECTION('center_axis',(-0.707106781186541,-0.696364240320025,-0.122787803968974));
#40108=DIRECTION('ref_axis',(-0.171087869746038,0.,0.985255774317391));
#40109=DIRECTION('',(0.,-0.17364817766693,0.984807753012208));
#40110=DIRECTION('',(0.,0.17364817766693,-0.984807753012208));
#40111=DIRECTION('center_axis',(0.707106781186549,0.0528875997482671,-0.705126160196077));
#40112=DIRECTION('ref_axis',(-0.706114387365559,0.,-0.708097784176282));
#40113=DIRECTION('',(0.,0.997198978933359,0.0747943608453594));
#40114=DIRECTION('center_axis',(0.,-0.270778428736215,0.962641699975202));
#40115=DIRECTION('ref_axis',(0.,-0.962641699975202,-0.270778428736215));
#40116=DIRECTION('center_axis',(0.,-0.984807753012208,-0.17364817766693));
#40117=DIRECTION('ref_axis',(0.,0.17364817766693,-0.984807753012208));
#40118=DIRECTION('center_axis',(0.561006631580395,-0.736633774843153,0.37768007768897));
#40119=DIRECTION('ref_axis',(0.558457227212238,0.,-0.829533317820579));
#40120=DIRECTION('',(0.705516335778309,0.186803215041197,-0.683630937568086));
#40121=DIRECTION('',(0.,0.456239332177625,0.889857107503286));
#40122=DIRECTION('',(-0.705516335778301,-0.664127077314131,-0.247349803169823));
#40123=DIRECTION('center_axis',(0.56100663158042,-0.449103523455307,-0.695397429203488));
#40124=DIRECTION('ref_axis',(-0.778302413620316,0.,-0.627889602520053));
#40125=DIRECTION('',(0.705516335778293,0.698825821880065,0.11785232549094));
#40126=DIRECTION('',(0.,-0.84004340562311,0.542519194747178));
#40127=DIRECTION('',(-0.705516335778311,0.180039139049711,-0.685443366267545));
#40128=DIRECTION('center_axis',(-0.561006631580394,-0.736633774843153,0.37768007768897));
#40129=DIRECTION('ref_axis',(0.55845722721224,0.,0.829533317820578));
#40130=DIRECTION('',(0.,-0.456239332177625,-0.889857107503286));
#40131=DIRECTION('',(0.705516335778311,-0.186803215041197,0.683630937568085));
#40132=DIRECTION('',(-0.705516335778303,0.664127077314129,0.247349803169823));
#40133=DIRECTION('center_axis',(-0.707106781186544,-0.25006674864043,0.661412595302213));
#40134=DIRECTION('ref_axis',(0.683116152038589,0.,0.730309744439982));
#40135=DIRECTION('',(0.,-0.935378662600772,-0.353647787425838));
#40136=DIRECTION('',(0.,0.935378662600772,0.353647787425838));
#40137=DIRECTION('center_axis',(-0.561006631580427,-0.449103523455304,-0.695397429203484));
#40138=DIRECTION('ref_axis',(-0.778302413620311,0.,0.627889602520059));
#40139=DIRECTION('',(0.705516335778293,-0.698825821880063,-0.117852325490952));
#40140=DIRECTION('',(-0.705516335778306,-0.180039139049709,0.68544336626755));
#40141=DIRECTION('',(0.,0.84004340562311,-0.542519194747178));
#40142=DIRECTION('center_axis',(-0.70710678118655,0.114142140686715,-0.697833484234922));
#40143=DIRECTION('ref_axis',(-0.702424227635741,0.,0.711758529580316));
#40144=DIRECTION('',(0.,-0.986885577683101,-0.161421363397451));
#40145=DIRECTION('',(0.,0.986885577683101,0.161421363397451));
#40146=DIRECTION('center_axis',(0.,-0.542519194747178,-0.84004340562311));
#40147=DIRECTION('ref_axis',(-1.,0.,0.));
#40148=DIRECTION('',(-1.,0.,0.));
#40149=DIRECTION('',(1.,0.,0.));
#40150=DIRECTION('center_axis',(-0.707106781186552,-0.683012701892215,-0.183012701892218));
#40151=DIRECTION('ref_axis',(-0.250562807085729,0.,0.968100345886376));
#40152=DIRECTION('',(0.,-0.258819045102521,0.965925826289068));
#40153=DIRECTION('',(0.,0.258819045102521,-0.965925826289068));
#40154=DIRECTION('center_axis',(0.,-0.889857107503286,0.456239332177625));
#40155=DIRECTION('ref_axis',(0.,-0.456239332177625,-0.889857107503286));
#40156=DIRECTION('',(-1.,0.,0.));
#40157=DIRECTION('',(1.,0.,0.));
#40158=DIRECTION('center_axis',(0.707106781186545,0.114142140686716,-0.697833484234927));
#40159=DIRECTION('ref_axis',(-0.702424227635745,0.,-0.711758529580311));
#40160=DIRECTION('',(0.,-0.986885577683101,-0.161421363397451));
#40161=DIRECTION('',(0.,0.986885577683101,0.161421363397451));
#40162=DIRECTION('center_axis',(0.707106781186553,-0.683012701892214,-0.183012701892218));
#40163=DIRECTION('ref_axis',(-0.250562807085728,0.,-0.968100345886376));
#40164=DIRECTION('',(0.,-0.258819045102521,0.965925826289068));
#40165=DIRECTION('',(0.,0.258819045102521,-0.965925826289068));
#40166=DIRECTION('center_axis',(0.707106781186545,-0.25006674864043,0.661412595302212));
#40167=DIRECTION('ref_axis',(0.683116152038587,0.,-0.730309744439983));
#40168=DIRECTION('',(0.,-0.935378662600772,-0.353647787425838));
#40169=DIRECTION('',(0.,0.935378662600772,0.353647787425838));
#40170=DIRECTION('center_axis',(1.,0.,0.));
#40171=DIRECTION('ref_axis',(0.,0.965925826289068,0.258819045102521));
#40172=DIRECTION('center_axis',(0.,-0.353647787425838,0.935378662600772));
#40173=DIRECTION('ref_axis',(0.,-0.935378662600772,-0.353647787425838));
#40174=DIRECTION('center_axis',(0.,-0.965925826289068,-0.258819045102521));
#40175=DIRECTION('ref_axis',(0.,0.258819045102521,-0.965925826289068));
#40176=DIRECTION('center_axis',(0.561006631580392,-0.386786669513444,-0.73189318319651));
#40177=DIRECTION('ref_axis',(-0.793664727118321,0.,-0.608355406755131));
#40178=DIRECTION('',(0.705516335778307,0.685895071683813,0.178310545369053));
#40179=DIRECTION('',(0.,-0.884130450221741,0.467240138462762));
#40180=DIRECTION('',(-0.705516335778315,0.239094361468882,-0.667143602430337));
#40181=DIRECTION('center_axis',(0.,-0.467240138462762,-0.884130450221741));
#40182=DIRECTION('ref_axis',(-1.,0.,0.));
#40183=DIRECTION('',(0.557191914001248,0.734167558056273,-0.387988617963614));
#40184=DIRECTION('',(1.,0.,0.));
#40185=DIRECTION('',(-1.,0.,0.));
#40186=DIRECTION('',(-0.55719191400126,0.734167558056266,-0.38798861796361));
#40187=DIRECTION('center_axis',(0.707106781186534,0.174527991013633,-0.685229874095376));
#40188=DIRECTION('ref_axis',(-0.695910561235558,0.,-0.718128463967841));
#40189=DIRECTION('',(0.,-0.96906138128887,-0.246819851905204));
#40190=DIRECTION('',(0.,0.96906138128887,0.246819851905204));
#40191=DIRECTION('center_axis',(0.56100663158041,-0.76674764862602,0.312041027189168));
#40192=DIRECTION('ref_axis',(0.486084108127403,0.,-0.873912032086747));
#40193=DIRECTION('',(0.70551633577831,0.245674734539575,-0.664748542502243));
#40194=DIRECTION('',(0.,0.376947046632547,0.926234810420662));
#40195=DIRECTION('',(-0.705516335778298,-0.640041917465765,-0.304291051193938));
#40196=DIRECTION('center_axis',(0.,-0.926234810420662,0.376947046632547));
#40197=DIRECTION('ref_axis',(0.,-0.376947046632547,-0.926234810420662));
#40198=DIRECTION('',(0.557191914001255,-0.313010701840811,-0.769130334536833));
#40199=DIRECTION('',(1.,0.,0.));
#40200=DIRECTION('',(-1.,0.,0.));
#40201=DIRECTION('',(-0.557191914001238,-0.313010701840815,-0.769130334536844));
#40202=DIRECTION('center_axis',(0.707106781186551,-0.664463024388671,-0.241844762647974));
#40203=DIRECTION('ref_axis',(-0.323615577118182,0.,-0.946188648339466));
#40204=DIRECTION('',(0.,-0.342020143325669,0.939692620785908));
#40205=DIRECTION('',(0.,0.342020143325669,-0.939692620785908));
#40206=DIRECTION('center_axis',(0.707106781186549,-0.306761075170856,0.637100967476913));
#40207=DIRECTION('ref_axis',(0.669373784875799,0.,-0.742925794491649));
#40208=DIRECTION('',(0.,-0.900996828806872,-0.433825672914778));
#40209=DIRECTION('',(0.,0.900996828806872,0.433825672914778));
#40210=DIRECTION('center_axis',(-0.707106781186539,0.174527991013631,-0.685229874095371));
#40211=DIRECTION('ref_axis',(-0.695910561235553,0.,0.718128463967846));
#40212=DIRECTION('',(-0.595596683047436,0.375326354772729,0.710207517952259));
#40213=DIRECTION('',(0.,0.96906138128887,0.246819851905204));
#40214=DIRECTION('',(0.,-0.96906138128887,-0.246819851905204));
#40215=DIRECTION('center_axis',(0.,-0.939692620785908,-0.342020143325669));
#40216=DIRECTION('ref_axis',(0.,0.342020143325669,-0.939692620785908));
#40217=DIRECTION('',(0.,-0.342020143325669,0.939692620785908));
#40218=DIRECTION('center_axis',(-0.707106781186536,-0.664463024388686,-0.241844762647979));
#40219=DIRECTION('ref_axis',(-0.323615577118194,0.,0.946188648339462));
#40220=DIRECTION('',(0.595596683047426,-0.744029261275698,0.302795392151933));
#40221=DIRECTION('',(0.,0.342020143325669,-0.939692620785908));
#40222=DIRECTION('center_axis',(-0.707106781186553,-0.306761075170854,0.637100967476909));
#40223=DIRECTION('ref_axis',(0.669373784875795,0.,0.742925794491652));
#40224=DIRECTION('',(0.,0.900996828806872,0.433825672914778));
#40225=DIRECTION('',(0.,-0.900996828806872,-0.433825672914778));
#40226=DIRECTION('center_axis',(0.,-0.433825672914778,0.900996828806872));
#40227=DIRECTION('ref_axis',(0.,-0.900996828806872,-0.433825672914778));
#40228=DIRECTION('center_axis',(0.,0.246819851905204,-0.96906138128887));
#40229=DIRECTION('ref_axis',(0.,0.96906138128887,0.246819851905204));
#40230=DIRECTION('center_axis',(0.561006631580396,-0.791026109827976,0.244027156056938));
#40231=DIRECTION('ref_axis',(0.398879012810069,0.,-0.917003562228449));
#40232=DIRECTION('',(0.705516335778307,0.302676520965598,-0.640807009641837));
#40233=DIRECTION('',(0.,0.294785966455742,0.955563307154871));
#40234=DIRECTION('',(-0.705516335778303,-0.611085652157587,-0.358916460582535));
#40235=DIRECTION('center_axis',(0.561006631580424,-0.321526135468413,-0.76281878813617));
#40236=DIRECTION('ref_axis',(-0.805595332751381,0.,-0.592466167683178));
#40237=DIRECTION('',(0.705516335778303,0.667744245837286,0.237411714330086));
#40238=DIRECTION('',(0.,-0.921488728241605,0.388405102597364));
#40239=DIRECTION('',(-0.705516335778299,0.296329931428078,-0.643766472946357));
#40240=DIRECTION('center_axis',(-0.561006631580408,-0.791026109827968,0.244027156056936));
#40241=DIRECTION('ref_axis',(0.398879012810058,0.,0.917003562228454));
#40242=DIRECTION('',(0.,-0.294785966455742,-0.955563307154871));
#40243=DIRECTION('',(0.705516335778314,-0.302676520965625,0.640807009641816));
#40244=DIRECTION('',(-0.705516335778287,0.611085652157596,0.35891646058255));
#40245=DIRECTION('center_axis',(-0.70710678118654,-0.361120764691837,0.607940616597043));
#40246=DIRECTION('ref_axis',(0.65193371809419,0.,0.758275957163278));
#40247=DIRECTION('',(0.,-0.859757865108992,-0.510701883081733));
#40248=DIRECTION('',(0.,0.859757865108992,0.510701883081733));
#40249=DIRECTION('center_axis',(-0.561006631580422,-0.321526135468414,-0.762818788136171));
#40250=DIRECTION('ref_axis',(-0.805595332751382,0.,0.592466167683177));
#40251=DIRECTION('',(0.705516335778289,-0.667744245837295,-0.237411714330105));
#40252=DIRECTION('',(-0.705516335778301,-0.296329931428077,0.643766472946356));
#40253=DIRECTION('',(0.,0.921488728241605,-0.388405102597364));
#40254=DIRECTION('center_axis',(-0.70710678118655,0.233585577946046,-0.667411250860823));
#40255=DIRECTION('ref_axis',(-0.686399640790371,0.,0.727224541062009));
#40256=DIRECTION('',(0.,-0.943862042647771,-0.330339892306057));
#40257=DIRECTION('',(0.,0.943862042647771,0.330339892306057));
#40258=DIRECTION('center_axis',(0.,-0.388405102597364,-0.921488728241605));
#40259=DIRECTION('ref_axis',(-1.,0.,0.));
#40260=DIRECTION('',(-1.,0.,0.));
#40261=DIRECTION('',(1.,0.,0.));
#40262=DIRECTION('center_axis',(-0.707106781186564,-0.640856382055774,-0.298836238730113));
#40263=DIRECTION('ref_axis',(-0.38928162063501,0.,0.921118787038773));
#40264=DIRECTION('',(0.,-0.422618261740699,0.90630778703665));
#40265=DIRECTION('',(0.,0.422618261740699,-0.90630778703665));
#40266=DIRECTION('center_axis',(0.,-0.955563307154871,0.294785966455742));
#40267=DIRECTION('ref_axis',(0.,-0.294785966455742,-0.955563307154871));
#40268=DIRECTION('',(-1.,0.,0.));
#40269=DIRECTION('',(1.,0.,0.));
#40270=DIRECTION('center_axis',(0.707106781186551,0.233585577946046,-0.667411250860822));
#40271=DIRECTION('ref_axis',(-0.686399640790369,0.,-0.72722454106201));
#40272=DIRECTION('',(0.,-0.943862042647771,-0.330339892306057));
#40273=DIRECTION('',(0.,0.943862042647771,0.330339892306057));
#40274=DIRECTION('center_axis',(0.707106781186551,-0.640856382055785,-0.298836238730118));
#40275=DIRECTION('ref_axis',(-0.389281620635021,0.,-0.921118787038768));
#40276=DIRECTION('',(0.,-0.422618261740699,0.90630778703665));
#40277=DIRECTION('',(0.,0.422618261740699,-0.90630778703665));
#40278=DIRECTION('center_axis',(0.707106781186547,-0.361120764691833,0.607940616597037));
#40279=DIRECTION('ref_axis',(0.651933718094183,0.,-0.758275957163284));
#40280=DIRECTION('',(0.,-0.859757865108992,-0.510701883081733));
#40281=DIRECTION('',(0.,0.859757865108992,0.510701883081733));
#40282=DIRECTION('center_axis',(1.,0.,0.));
#40283=DIRECTION('ref_axis',(0.,0.90630778703665,0.422618261740699));
#40284=DIRECTION('center_axis',(0.,-0.510701883081733,0.859757865108992));
#40285=DIRECTION('ref_axis',(0.,-0.859757865108992,-0.510701883081733));
#40286=DIRECTION('center_axis',(0.,-0.90630778703665,-0.422618261740699));
#40287=DIRECTION('ref_axis',(0.,0.422618261740699,-0.90630778703665));
#40288=DIRECTION('center_axis',(0.561006631580406,-0.809284384699504,0.174156090919475));
#40289=DIRECTION('ref_axis',(0.296477762129627,0.,-0.955039756535092));
#40290=DIRECTION('',(0.705516335778312,0.357374756306047,-0.611988548508171));
#40291=DIRECTION('',(0.,0.210381387077564,0.977619390136734));
#40292=DIRECTION('',(-0.705516335778298,-0.577478656052899,-0.410810298986407));
#40293=DIRECTION('center_axis',(0.561006631580407,-0.253818593389688,-0.787938881495568));
#40294=DIRECTION('ref_axis',(-0.814616058663781,0.,-0.580000583592023));
#40295=DIRECTION('',(0.705516335778306,0.644511483084942,0.29470603679192));
#40296=DIRECTION('',(0.,-0.951833920629446,0.306614069375781));
#40297=DIRECTION('',(-0.7055163357783,0.351310251680245,-0.615489891886393));
#40298=DIRECTION('center_axis',(-0.561006631580389,-0.809284384699515,0.174156090919477));
#40299=DIRECTION('ref_axis',(0.296477762129639,0.,0.955039756535089));
#40300=DIRECTION('',(0.,-0.210381387077564,-0.977619390136734));
#40301=DIRECTION('',(0.705516335778309,-0.357374756306019,0.611988548508191));
#40302=DIRECTION('',(-0.705516335778317,0.577478656052887,0.410810298986391));
#40303=DIRECTION('center_axis',(-0.707106781186541,-0.412732107142829,0.574153470540282));
#40304=DIRECTION('ref_axis',(0.63034738821444,0.,0.776313190774982));
#40305=DIRECTION('',(0.,-0.81197562492164,-0.583691343548208));
#40306=DIRECTION('',(0.,0.81197562492164,0.583691343548208));
#40307=DIRECTION('center_axis',(-0.561006631580389,-0.253818593389691,-0.787938881495579));
#40308=DIRECTION('ref_axis',(-0.814616058663794,0.,0.580000583592005));
#40309=DIRECTION('',(0.705516335778322,-0.644511483084929,-0.294706036791912));
#40310=DIRECTION('',(-0.705516335778301,-0.351310251680269,0.615489891886378));
#40311=DIRECTION('',(0.,0.951833920629446,-0.306614069375781));
#40312=DIRECTION('center_axis',(-0.707106781186549,0.290865437587466,-0.644513225013304));
#40313=DIRECTION('ref_axis',(-0.673638686438956,0.,0.739060836557315));
#40314=DIRECTION('',(0.,-0.911479343942639,-0.411345846661781));
#40315=DIRECTION('',(0.,0.911479343942639,0.411345846661781));
#40316=DIRECTION('center_axis',(0.,-0.306614069375781,-0.951833920629447));
#40317=DIRECTION('ref_axis',(-1.,0.,0.));
#40318=DIRECTION('',(-1.,0.,0.));
#40319=DIRECTION('',(1.,0.,0.));
#40320=DIRECTION('center_axis',(-0.707106781186533,-0.612372435695807,-0.353553390593281));
#40321=DIRECTION('ref_axis',(-0.447213595499973,0.,0.894427190999908));
#40322=DIRECTION('',(0.,-0.5,0.866025403784439));
#40323=DIRECTION('',(0.,0.5,-0.866025403784439));
#40324=DIRECTION('center_axis',(0.,-0.977619390136734,0.210381387077564));
#40325=DIRECTION('ref_axis',(0.,-0.210381387077564,-0.977619390136734));
#40326=DIRECTION('',(-1.,0.,0.));
#40327=DIRECTION('',(1.,0.,0.));
#40328=DIRECTION('center_axis',(0.707106781186551,0.290865437587465,-0.644513225013302));
#40329=DIRECTION('ref_axis',(-0.673638686438954,0.,-0.739060836557317));
#40330=DIRECTION('',(0.,-0.911479343942639,-0.411345846661781));
#40331=DIRECTION('',(0.,0.911479343942639,0.411345846661781));
#40332=DIRECTION('center_axis',(0.707106781186549,-0.612372435695794,-0.353553390593273));
#40333=DIRECTION('ref_axis',(-0.447213595499957,0.,-0.894427190999916));
#40334=DIRECTION('',(0.,-0.5,0.866025403784439));
#40335=DIRECTION('',(0.,0.5,-0.866025403784439));
#40336=DIRECTION('center_axis',(0.707106781186542,-0.412732107142828,0.57415347054028));
#40337=DIRECTION('ref_axis',(0.630347388214439,0.,-0.776313190774983));
#40338=DIRECTION('',(0.,-0.81197562492164,-0.583691343548208));
#40339=DIRECTION('',(0.,0.81197562492164,0.583691343548208));
#40340=DIRECTION('center_axis',(1.,0.,0.));
#40341=DIRECTION('ref_axis',(0.,0.866025403784439,0.5));
#40342=DIRECTION('center_axis',(0.,-0.583691343548208,0.81197562492164));
#40343=DIRECTION('ref_axis',(0.,-0.81197562492164,-0.583691343548208));
#40344=DIRECTION('center_axis',(0.,-0.866025403784439,-0.5));
#40345=DIRECTION('ref_axis',(0.,0.5,-0.866025403784439));
#40346=DIRECTION('center_axis',(0.707106781186547,-0.461202309044,0.53599666988936));
#40347=DIRECTION('ref_axis',(0.604079438549193,0.,-0.796924106751761));
#40348=DIRECTION('',(0.595596683047425,0.797046293239184,-0.099908946429145));
#40349=DIRECTION('',(0.,0.758013759944347,0.652238560447812));
#40350=DIRECTION('',(0.,-0.758013759944347,-0.652238560447812));
#40351=DIRECTION('',(0.557191914001244,-0.103279542068703,-0.823935984868794));
#40352=DIRECTION('center_axis',(1.,0.,0.));
#40353=DIRECTION('ref_axis',(0.,0.819152044288992,0.573576436351046));
#40354=DIRECTION('',(0.,-0.573576436351046,0.819152044288992));
#40355=DIRECTION('',(0.,-0.872159737063827,-0.489221210746995));
#40356=DIRECTION('center_axis',(0.707106781186547,-0.57922796533957,-0.405579787672639));
#40357=DIRECTION('ref_axis',(-0.497542812164523,0.,-0.867439421552547));
#40358=DIRECTION('',(0.55719191400124,0.103279542068703,0.823935984868796));
#40359=DIRECTION('',(0.,0.573576436351046,-0.819152044288992));
#40360=DIRECTION('',(0.705516335778315,0.616373598779637,0.349757468365408));
#40361=DIRECTION('center_axis',(0.,-0.992235199256928,0.124375678311978));
#40362=DIRECTION('ref_axis',(0.,-0.124375678311978,-0.992235199256928));
#40363=DIRECTION('',(-1.,0.,0.));
#40364=DIRECTION('',(0.,-0.124375678311978,-0.992235199256928));
#40365=DIRECTION('',(1.,0.,0.));
#40366=DIRECTION('center_axis',(0.561006631580405,-0.184179338555412,-0.807062284196269));
#40367=DIRECTION('ref_axis',(-0.821109284001921,0.,-0.570771008133607));
#40368=DIRECTION('',(0.,-0.974935082148261,0.22248951794762));
#40369=DIRECTION('',(-0.7055163357783,0.403616888790171,-0.582529061106229));
#40370=DIRECTION('center_axis',(-0.561006631580388,-0.821383516744214,0.102959592771799));
#40371=DIRECTION('ref_axis',(0.180511696561728,0.,0.983572837874454));
#40372=DIRECTION('',(0.705516335778303,-0.409353153962173,0.578512484991619));
#40373=DIRECTION('',(-0.705516335778314,0.539476698684484,0.459577622960944));
#40374=DIRECTION('center_axis',(-0.707106781186546,-0.461202309044001,0.535996669889361));
#40375=DIRECTION('ref_axis',(0.604079438549194,0.,0.79692410675176));
#40376=DIRECTION('',(0.,-0.758013759944347,-0.652238560447812));
#40377=DIRECTION('',(0.,0.758013759944347,0.652238560447812));
#40378=DIRECTION('center_axis',(-0.561006631580403,-0.184179338555412,-0.80706228419627));
#40379=DIRECTION('ref_axis',(-0.821109284001922,0.,0.570771008133605));
#40380=DIRECTION('',(0.705516335778317,-0.616373598779635,-0.349757468365407));
#40381=DIRECTION('',(-0.705516335778301,-0.40361688879017,0.582529061106227));
#40382=DIRECTION('',(0.,0.974935082148261,-0.22248951794762));
#40383=DIRECTION('center_axis',(-0.707106781186545,0.345931635619494,-0.616710064355711));
#40384=DIRECTION('ref_axis',(-0.657291420225582,0.,0.753636509796226));
#40385=DIRECTION('',(0.,-0.872159737063827,-0.489221210746995));
#40386=DIRECTION('',(0.,0.872159737063827,0.489221210746995));
#40387=DIRECTION('center_axis',(0.,-0.22248951794762,-0.974935082148261));
#40388=DIRECTION('ref_axis',(-1.,0.,0.));
#40389=DIRECTION('',(-1.,0.,0.));
#40390=DIRECTION('',(1.,0.,0.));
#40391=DIRECTION('center_axis',(-0.707106781186546,-0.579227965339571,-0.40557978767264));
#40392=DIRECTION('ref_axis',(-0.497542812164525,0.,0.867439421552546));
#40393=DIRECTION('',(0.,-0.573576436351046,0.819152044288992));
#40394=DIRECTION('',(0.,0.573576436351046,-0.819152044288992));
#40395=DIRECTION('center_axis',(0.707106781186546,0.345931635619494,-0.61671006435571));
#40396=DIRECTION('ref_axis',(-0.657291420225581,0.,-0.753636509796227));
#40397=DIRECTION('',(0.,0.872159737063827,0.489221210746995));
#40398=DIRECTION('center_axis',(0.,-0.652238560447812,0.758013759944347));
#40399=DIRECTION('ref_axis',(0.,-0.758013759944347,-0.652238560447812));
#40400=DIRECTION('center_axis',(0.,-0.819152044288992,-0.573576436351046));
#40401=DIRECTION('ref_axis',(0.,0.573576436351046,-0.819152044288992));
#40402=DIRECTION('center_axis',(0.56100663158041,-0.827231424261547,0.0309795099544078));
#40403=DIRECTION('ref_axis',(0.055137286528736,0.,-0.998478782766188));
#40404=DIRECTION('',(0.705516335778304,0.458216126942529,-0.540633592148827));
#40405=DIRECTION('',(0.,0.037423395534326,0.999299499382783));
#40406=DIRECTION('',(-0.705516335778297,-0.497368997894162,-0.50484728372422));
#40407=DIRECTION('center_axis',(0.561006631580388,-0.113138367744187,-0.820043455596719));
#40408=DIRECTION('ref_axis',(-0.825342782028786,0.,-0.564631997103409));
#40409=DIRECTION('',(0.705516335778318,0.58354473921108,0.402147034415285));
#40410=DIRECTION('',(0.,-0.990616399010033,0.136671686945011));
#40411=DIRECTION('',(-0.705516335778308,0.452851757665877,-0.545134832430359));
#40412=DIRECTION('center_axis',(-0.561006631580408,-0.827231424261548,0.0309795099544079));
#40413=DIRECTION('ref_axis',(0.0551372865287363,0.,0.998478782766188));
#40414=DIRECTION('',(0.,-0.037423395534326,-0.999299499382783));
#40415=DIRECTION('',(0.705516335778305,-0.458216126942528,0.540633592148826));
#40416=DIRECTION('',(-0.705516335778298,0.497368997894161,0.504847283724219));
#40417=DIRECTION('center_axis',(-0.707106781186549,-0.506162482891781,0.493760610936946));
#40418=DIRECTION('ref_axis',(0.572517134274668,0.,0.819892755768657));
#40419=DIRECTION('',(0.,-0.698282952552655,-0.715821848069998));
#40420=DIRECTION('',(0.,0.698282952552655,0.715821848069998));
#40421=DIRECTION('center_axis',(-0.561006631580386,-0.113138367744187,-0.82004345559672));
#40422=DIRECTION('ref_axis',(-0.825342782028787,0.,0.564631997103407));
#40423=DIRECTION('',(0.705516335778319,-0.583544739211079,-0.402147034415284));
#40424=DIRECTION('',(-0.70551633577831,-0.452851757665876,0.545134832430358));
#40425=DIRECTION('',(0.,0.990616399010033,-0.136671686945011));
#40426=DIRECTION('center_axis',(-0.70710678118654,0.398365085025227,-0.584213367728653));
#40427=DIRECTION('ref_axis',(-0.636934375125939,0.,0.770918025332739));
#40428=DIRECTION('',(0.,-0.826202467961513,-0.563373306018581));
#40429=DIRECTION('',(0.,0.826202467961513,0.563373306018581));
#40430=DIRECTION('center_axis',(0.,-0.136671686945011,-0.990616399010033));
#40431=DIRECTION('ref_axis',(-1.,0.,0.));
#40432=DIRECTION('',(-1.,0.,0.));
#40433=DIRECTION('',(1.,0.,0.));
#40434=DIRECTION('center_axis',(-0.707106781186548,-0.541675220419702,-0.454519477672043));
#40435=DIRECTION('ref_axis',(-0.540716203060936,0.,0.841205080671393));
#40436=DIRECTION('',(0.,-0.642787609686539,0.766044443118978));
#40437=DIRECTION('',(0.,0.642787609686539,-0.766044443118978));
#40438=DIRECTION('center_axis',(0.,-0.999299499382783,0.037423395534326));
#40439=DIRECTION('ref_axis',(0.,-0.037423395534326,-0.999299499382783));
#40440=DIRECTION('',(-1.,0.,0.));
#40441=DIRECTION('',(1.,0.,0.));
#40442=DIRECTION('center_axis',(0.707106781186542,0.398365085025226,-0.584213367728652));
#40443=DIRECTION('ref_axis',(-0.636934375125937,0.,-0.770918025332741));
#40444=DIRECTION('',(0.,-0.826202467961513,-0.563373306018581));
#40445=DIRECTION('',(0.,0.826202467961513,0.563373306018581));
#40446=DIRECTION('center_axis',(0.70710678118655,-0.5416752204197,-0.454519477672042));
#40447=DIRECTION('ref_axis',(-0.540716203060935,0.,-0.841205080671394));
#40448=DIRECTION('',(0.,-0.642787609686539,0.766044443118978));
#40449=DIRECTION('',(0.,0.642787609686539,-0.766044443118978));
#40450=DIRECTION('center_axis',(0.707106781186551,-0.50616248289178,0.493760610936944));
#40451=DIRECTION('ref_axis',(0.572517134274666,0.,-0.819892755768658));
#40452=DIRECTION('',(0.,-0.698282952552655,-0.715821848069998));
#40453=DIRECTION('',(0.,0.698282952552655,0.715821848069998));
#40454=DIRECTION('center_axis',(1.,0.,0.));
#40455=DIRECTION('ref_axis',(0.,0.766044443118978,0.642787609686539));
#40456=DIRECTION('center_axis',(0.,-0.715821848069998,0.698282952552655));
#40457=DIRECTION('ref_axis',(0.,-0.698282952552655,-0.715821848069998));
#40458=DIRECTION('center_axis',(0.,-0.766044443118978,-0.642787609686539));
#40459=DIRECTION('ref_axis',(0.,0.642787609686539,-0.766044443118978));
#40460=DIRECTION('center_axis',(0.561006631580414,-0.0412363456396373,-0.826783601144269));
#40461=DIRECTION('ref_axis',(-0.827487445286302,0.,-0.561484218739537));
#40462=DIRECTION('',(0.705516335778305,0.546274751823179,0.451476018710272));
#40463=DIRECTION('',(0.,-0.998758526924799,0.0498137018801604));
#40464=DIRECTION('',(-0.705516335778304,0.49864015122633,-0.503591798518341));
#40465=DIRECTION('center_axis',(0.,-0.0498137018801604,-0.998758526924799));
#40466=DIRECTION('ref_axis',(-1.,0.,0.));
#40467=DIRECTION('',(0.55719191400124,0.829352850155045,-0.041364488529864));
#40468=DIRECTION('',(1.,0.,0.));
#40469=DIRECTION('',(-1.,0.,0.));
#40470=DIRECTION('',(-0.557191914001243,0.829352850155043,-0.0413644885298639));
#40471=DIRECTION('center_axis',(0.707106781186551,0.447766735594493,-0.547270454615491));
#40472=DIRECTION('ref_axis',(-0.612056372482119,0.,-0.790814135498367));
#40473=DIRECTION('',(0.,-0.773957299203321,-0.633237790257263));
#40474=DIRECTION('',(0.,0.773957299203321,0.633237790257263));
#40475=DIRECTION('center_axis',(0.561006631580404,-0.826783601144275,-0.0412363456396555));
#40476=DIRECTION('ref_axis',(-0.0733064378127395,0.,-0.997309463594529));
#40477=DIRECTION('',(0.705516335778296,0.503591798518335,-0.498640151226349));
#40478=DIRECTION('',(0.,-0.0498137018801819,0.998758526924798));
#40479=DIRECTION('',(-0.705516335778303,-0.451476018710246,-0.546274751823203));
#40480=DIRECTION('center_axis',(0.,-0.998758526924798,-0.0498137018801819));
#40481=DIRECTION('ref_axis',(0.,0.0498137018801819,-0.998758526924798));
#40482=DIRECTION('',(0.557191914001234,0.0413644885298821,-0.829352850155049));
#40483=DIRECTION('',(1.,0.,0.));
#40484=DIRECTION('',(-1.,0.,0.));
#40485=DIRECTION('',(-0.557191914001249,0.0413644885298816,-0.829352850155038));
#40486=DIRECTION('center_axis',(0.707106781186548,-0.5,-0.5));
#40487=DIRECTION('ref_axis',(-0.577350269189625,0.,-0.816496580927727));
#40488=DIRECTION('',(0.,-0.707106781186547,0.707106781186548));
#40489=DIRECTION('',(0.,0.707106781186547,-0.707106781186548));
#40490=DIRECTION('center_axis',(0.707106781186552,-0.547270454615491,0.447766735594493));
#40491=DIRECTION('ref_axis',(0.534994468449983,0.,-0.844855560867016));
#40492=DIRECTION('',(0.,-0.633237790257263,-0.773957299203321));
#40493=DIRECTION('',(0.,0.633237790257263,0.773957299203321));
#40494=DIRECTION('center_axis',(-0.70710678118655,0.447766735594494,-0.547270454615492));
#40495=DIRECTION('ref_axis',(-0.61205637248212,0.,0.790814135498366));
#40496=DIRECTION('',(-0.595596683047422,0.0400145312984556,0.802286375571637));
#40497=DIRECTION('',(0.,0.773957299203321,0.633237790257263));
#40498=DIRECTION('',(0.,-0.773957299203321,-0.633237790257263));
#40499=DIRECTION('center_axis',(0.,-0.707106781186548,-0.707106781186547));
#40500=DIRECTION('ref_axis',(0.,0.707106781186547,-0.707106781186548));
#40501=DIRECTION('',(0.,-0.707106781186547,0.707106781186548));
#40502=DIRECTION('center_axis',(-0.707106781186547,-0.500000000000001,-0.500000000000001));
#40503=DIRECTION('ref_axis',(-0.577350269189627,0.,0.816496580927725));
#40504=DIRECTION('',(0.595596683047432,-0.802286375571628,-0.0400145312984774));
#40505=DIRECTION('',(0.,0.707106781186547,-0.707106781186548));
#40506=DIRECTION('center_axis',(-0.70710678118655,-0.547270454615492,0.447766735594494));
#40507=DIRECTION('ref_axis',(0.534994468449985,0.,0.844855560867015));
#40508=DIRECTION('',(0.,0.633237790257263,0.773957299203321));
#40509=DIRECTION('',(0.,-0.633237790257263,-0.773957299203321));
#40510=DIRECTION('center_axis',(0.,-0.773957299203321,0.633237790257263));
#40511=DIRECTION('ref_axis',(0.,-0.633237790257263,-0.773957299203321));
#40512=DIRECTION('center_axis',(0.,0.633237790257263,-0.773957299203321));
#40513=DIRECTION('ref_axis',(0.,0.773957299203321,0.633237790257263));
#40514=DIRECTION('center_axis',(0.561006631580392,-0.820043455596711,-0.113138367744223));
#40515=DIRECTION('ref_axis',(-0.197690230426254,0.,-0.98026454225072));
#40516=DIRECTION('',(0.705516335778306,0.545134832430383,-0.452851757665851));
#40517=DIRECTION('',(0.,-0.136671686945054,0.990616399010027));
#40518=DIRECTION('',(-0.705516335778304,-0.402147034415252,-0.583544739211119));
#40519=DIRECTION('center_axis',(0.5610066315804,0.0309795099544278,-0.827231424261552));
#40520=DIRECTION('ref_axis',(-0.827628669643389,0.,-0.561276032968016));
#40521=DIRECTION('',(0.705516335778306,0.504847283724201,0.497368997894168));
#40522=DIRECTION('',(0.,-0.999299499382783,-0.0374233955343499));
#40523=DIRECTION('',(-0.705516335778302,0.540633592148851,-0.458216126942503));
#40524=DIRECTION('center_axis',(-0.56100663158039,-0.820043455596712,-0.113138367744223));
#40525=DIRECTION('ref_axis',(-0.197690230426255,0.,0.98026454225072));
#40526=DIRECTION('',(0.,0.136671686945054,-0.990616399010027));
#40527=DIRECTION('',(0.705516335778308,-0.545134832430382,0.45285175766585));
#40528=DIRECTION('',(-0.705516335778306,0.402147034415251,0.583544739211118));
#40529=DIRECTION('center_axis',(-0.707106781186547,-0.584213367728647,0.398365085025223));
#40530=DIRECTION('ref_axis',(0.490839120629135,0.,0.871250226777599));
#40531=DIRECTION('',(0.,-0.563373306018581,-0.826202467961513));
#40532=DIRECTION('',(0.,0.563373306018581,0.826202467961513));
#40533=DIRECTION('center_axis',(-0.561006631580419,0.0309795099544274,-0.82723142426154));
#40534=DIRECTION('ref_axis',(-0.827628669643377,0.,0.561276032968035));
#40535=DIRECTION('',(0.705516335778298,-0.504847283724194,-0.497368997894186));
#40536=DIRECTION('',(-0.705516335778296,-0.540633592148843,0.458216126942521));
#40537=DIRECTION('',(0.,0.999299499382783,0.0374233955343499));
#40538=DIRECTION('center_axis',(-0.707106781186558,0.493760610936939,-0.506162482891774));
#40539=DIRECTION('ref_axis',(-0.582064997116532,0.,0.813142262541882));
#40540=DIRECTION('',(0.,-0.715821848069998,-0.698282952552655));
#40541=DIRECTION('',(0.,0.715821848069998,0.698282952552655));
#40542=DIRECTION('center_axis',(0.,0.0374233955343499,-0.999299499382783));
#40543=DIRECTION('ref_axis',(-1.,0.,0.));
#40544=DIRECTION('',(-1.,0.,0.));
#40545=DIRECTION('',(1.,0.,0.));
#40546=DIRECTION('center_axis',(-0.707106781186558,-0.454519477672037,-0.541675220419694));
#40547=DIRECTION('ref_axis',(-0.608120402411332,0.,0.793844806099454));
#40548=DIRECTION('',(0.,-0.766044443118978,0.642787609686539));
#40549=DIRECTION('',(0.,0.766044443118978,-0.642787609686539));
#40550=DIRECTION('center_axis',(0.,-0.990616399010027,-0.136671686945054));
#40551=DIRECTION('ref_axis',(0.,0.136671686945054,-0.990616399010027));
#40552=DIRECTION('',(-1.,0.,0.));
#40553=DIRECTION('',(1.,0.,0.));
#40554=DIRECTION('center_axis',(0.70710678118656,0.493760610936938,-0.506162482891773));
#40555=DIRECTION('ref_axis',(-0.58206499711653,0.,-0.813142262541884));
#40556=DIRECTION('',(0.,-0.715821848069998,-0.698282952552655));
#40557=DIRECTION('',(0.,0.715821848069998,0.698282952552655));
#40558=DIRECTION('center_axis',(0.70710678118655,-0.454519477672042,-0.5416752204197));
#40559=DIRECTION('ref_axis',(-0.608120402411341,0.,-0.793844806099447));
#40560=DIRECTION('',(0.,-0.766044443118978,0.642787609686539));
#40561=DIRECTION('',(0.,0.766044443118978,-0.642787609686539));
#40562=DIRECTION('center_axis',(0.707106781186549,-0.584213367728646,0.398365085025222));
#40563=DIRECTION('ref_axis',(0.490839120629133,0.,-0.8712502267776));
#40564=DIRECTION('',(0.,-0.563373306018581,-0.826202467961513));
#40565=DIRECTION('',(0.,0.563373306018581,0.826202467961513));
#40566=DIRECTION('center_axis',(1.,0.,0.));
#40567=DIRECTION('ref_axis',(0.,0.642787609686539,0.766044443118978));
#40568=DIRECTION('center_axis',(0.,-0.826202467961513,0.563373306018581));
#40569=DIRECTION('ref_axis',(0.,-0.563373306018581,-0.826202467961513));
#40570=DIRECTION('center_axis',(0.,-0.642787609686539,-0.766044443118978));
#40571=DIRECTION('ref_axis',(0.,0.766044443118978,-0.642787609686539));
#40572=DIRECTION('center_axis',(0.56100663158041,-0.807062284196261,-0.18417933855543));
#40573=DIRECTION('ref_axis',(-0.311921838389611,0.,-0.950107765853772));
#40574=DIRECTION('',(0.705516335778302,0.582529061106243,-0.403616888790147));
#40575=DIRECTION('',(0.,-0.222489517947642,0.974935082148255));
#40576=DIRECTION('',(-0.705516335778307,-0.349757468365392,-0.616373598779655));
#40577=DIRECTION('center_axis',(0.56100663158042,0.102959592771817,-0.82138351674419));
#40578=DIRECTION('ref_axis',(-0.825772049781951,0.,-0.564004008672735));
#40579=DIRECTION('',(0.705516335778302,0.459577622960913,0.539476698684527));
#40580=DIRECTION('',(0.,-0.992235199256925,-0.124375678312001));
#40581=DIRECTION('',(-0.705516335778294,0.578512484991614,-0.409353153962195));
#40582=DIRECTION('center_axis',(-0.561006631580408,-0.807062284196262,-0.18417933855543));
#40583=DIRECTION('ref_axis',(-0.311921838389613,0.,0.950107765853771));
#40584=DIRECTION('',(0.,0.222489517947642,-0.974935082148255));
#40585=DIRECTION('',(0.705516335778303,-0.582529061106242,0.403616888790146));
#40586=DIRECTION('',(-0.705516335778309,0.349757468365391,0.616373598779654));
#40587=DIRECTION('center_axis',(-0.707106781186545,-0.616710064355711,0.345931635619495));
#40588=DIRECTION('ref_axis',(0.439451044888515,0.,0.898266541259548));
#40589=DIRECTION('',(0.,-0.489221210746995,-0.872159737063827));
#40590=DIRECTION('',(0.,0.489221210746995,0.872159737063827));
#40591=DIRECTION('center_axis',(-0.561006631580396,0.102959592771819,-0.821383516744206));
#40592=DIRECTION('ref_axis',(-0.825772049781968,0.,0.564004008672711));
#40593=DIRECTION('',(0.705516335778305,-0.459577622960938,-0.539476698684502));
#40594=DIRECTION('',(-0.705516335778313,-0.578512484991602,0.409353153962179));
#40595=DIRECTION('',(0.,0.992235199256925,0.124375678312001));
#40596=DIRECTION('center_axis',(-0.707106781186541,0.535996669889364,-0.461202309044004));
#40597=DIRECTION('ref_axis',(-0.546305769586294,0.,0.837585820150226));
#40598=DIRECTION('',(0.,-0.652238560447812,-0.758013759944346));
#40599=DIRECTION('',(0.,0.652238560447812,0.758013759944346));
#40600=DIRECTION('center_axis',(0.,0.124375678312001,-0.992235199256925));
#40601=DIRECTION('ref_axis',(-1.,0.,0.));
#40602=DIRECTION('',(-1.,0.,0.));
#40603=DIRECTION('',(1.,0.,0.));
#40604=DIRECTION('center_axis',(-0.707106781186546,-0.40557978767264,-0.579227965339571));
#40605=DIRECTION('ref_axis',(-0.633687274224644,0.,0.773589321594954));
#40606=DIRECTION('',(0.,-0.819152044288992,0.573576436351046));
#40607=DIRECTION('',(0.,0.819152044288992,-0.573576436351046));
#40608=DIRECTION('center_axis',(0.,-0.974935082148256,-0.222489517947642));
#40609=DIRECTION('ref_axis',(0.,0.222489517947642,-0.974935082148255));
#40610=DIRECTION('',(-1.,0.,0.));
#40611=DIRECTION('',(1.,0.,0.));
#40612=DIRECTION('center_axis',(0.707106781186552,0.535996669889356,-0.461202309043997));
#40613=DIRECTION('ref_axis',(-0.546305769586282,0.,-0.837585820150234));
#40614=DIRECTION('',(0.,-0.652238560447812,-0.758013759944346));
#40615=DIRECTION('',(0.,0.652238560447812,0.758013759944346));
#40616=DIRECTION('center_axis',(0.707106781186547,-0.405579787672639,-0.579227965339569));
#40617=DIRECTION('ref_axis',(-0.633687274224642,0.,-0.773589321594955));
#40618=DIRECTION('',(0.,-0.819152044288992,0.573576436351046));
#40619=DIRECTION('',(0.,0.819152044288992,-0.573576436351046));
#40620=DIRECTION('center_axis',(0.707106781186546,-0.61671006435571,0.345931635619494));
#40621=DIRECTION('ref_axis',(0.439451044888514,0.,-0.898266541259549));
#40622=DIRECTION('',(0.,-0.489221210746995,-0.872159737063827));
#40623=DIRECTION('',(0.,0.489221210746995,0.872159737063827));
#40624=DIRECTION('center_axis',(1.,0.,0.));
#40625=DIRECTION('ref_axis',(0.,0.573576436351046,0.819152044288992));
#40626=DIRECTION('center_axis',(0.,-0.872159737063827,0.489221210746995));
#40627=DIRECTION('ref_axis',(0.,-0.489221210746995,-0.872159737063827));
#40628=DIRECTION('center_axis',(0.,-0.573576436351046,-0.819152044288992));
#40629=DIRECTION('ref_axis',(0.,0.819152044288992,-0.573576436351046));
#40630=DIRECTION('center_axis',(0.707106781186551,-0.644513225013302,0.290865437587466));
#40631=DIRECTION('ref_axis',(0.380418570543385,0.,-0.924814419862562));
#40632=DIRECTION('',(0.595596683047424,0.764592607463602,0.246298062832244));
#40633=DIRECTION('',(0.,0.411345846661781,0.911479343942639));
#40634=DIRECTION('',(0.,-0.411345846661781,-0.911479343942639));
#40635=DIRECTION('',(0.557191914001241,0.25460734049242,-0.790387419648751));
#40636=DIRECTION('center_axis',(1.,0.,0.));
#40637=DIRECTION('ref_axis',(0.,0.5,0.866025403784439));
#40638=DIRECTION('',(0.,-0.866025403784439,0.5));
#40639=DIRECTION('',(0.,-0.583691343548208,-0.81197562492164));
#40640=DIRECTION('center_axis',(0.707106781186545,-0.353553390593275,-0.612372435695796));
#40641=DIRECTION('ref_axis',(-0.654653670707979,0.,-0.755928946018453));
#40642=DIRECTION('',(0.557191914001241,-0.25460734049242,0.790387419648751));
#40643=DIRECTION('',(0.,0.866025403784439,-0.5));
#40644=DIRECTION('',(0.705516335778306,0.410810298986386,0.577478656052905));
#40645=DIRECTION('center_axis',(0.,-0.951833920629443,-0.306614069375792));
#40646=DIRECTION('ref_axis',(0.,0.306614069375792,-0.951833920629443));
#40647=DIRECTION('',(-1.,0.,0.));
#40648=DIRECTION('',(0.,0.306614069375792,-0.951833920629443));
#40649=DIRECTION('',(1.,0.,0.));
#40650=DIRECTION('center_axis',(0.561006631580401,0.174156090919492,-0.809284384699503));
#40651=DIRECTION('ref_axis',(-0.821843752318938,0.,-0.569712951208174));
#40652=DIRECTION('',(0.,-0.97761939013673,-0.210381387077584));
#40653=DIRECTION('',(-0.705516335778302,0.6119885485082,-0.357374756306017));
#40654=DIRECTION('center_axis',(-0.561006631580415,-0.787938881495563,-0.253818593389686));
#40655=DIRECTION('ref_axis',(-0.412208150462309,0.,0.911089699586403));
#40656=DIRECTION('',(0.705516335778296,-0.615489891886399,0.351310251680242));
#40657=DIRECTION('',(-0.705516335778305,0.294706036791931,0.644511483084939));
#40658=DIRECTION('center_axis',(-0.707106781186555,-0.644513225013298,0.290865437587464));
#40659=DIRECTION('ref_axis',(0.380418570543382,0.,0.924814419862564));
#40660=DIRECTION('',(0.,-0.411345846661781,-0.911479343942639));
#40661=DIRECTION('',(0.,0.411345846661781,0.911479343942639));
#40662=DIRECTION('center_axis',(-0.5610066315804,0.174156090919493,-0.809284384699504));
#40663=DIRECTION('ref_axis',(-0.82184375231894,0.,0.569712951208172));
#40664=DIRECTION('',(0.705516335778307,-0.410810298986385,-0.577478656052904));
#40665=DIRECTION('',(-0.705516335778303,-0.611988548508199,0.357374756306016));
#40666=DIRECTION('',(0.,0.97761939013673,0.210381387077584));
#40667=DIRECTION('center_axis',(-0.707106781186546,0.574153470540278,-0.412732107142826));
#40668=DIRECTION('ref_axis',(-0.504101701135472,0.,0.86364429883623));
#40669=DIRECTION('',(0.,-0.583691343548208,-0.81197562492164));
#40670=DIRECTION('',(0.,0.583691343548208,0.81197562492164));
#40671=DIRECTION('center_axis',(0.,0.210381387077584,-0.97761939013673));
#40672=DIRECTION('ref_axis',(-1.,0.,0.));
#40673=DIRECTION('',(-1.,0.,0.));
#40674=DIRECTION('',(1.,0.,0.));
#40675=DIRECTION('center_axis',(-0.707106781186544,-0.353553390593276,-0.612372435695798));
#40676=DIRECTION('ref_axis',(-0.654653670707981,0.,0.755928946018451));
#40677=DIRECTION('',(0.,-0.866025403784439,0.5));
#40678=DIRECTION('',(0.,0.866025403784439,-0.5));
#40679=DIRECTION('center_axis',(0.707106781186547,0.574153470540276,-0.412732107142825));
#40680=DIRECTION('ref_axis',(-0.50410170113547,0.,-0.863644298836231));
#40681=DIRECTION('',(0.,0.583691343548208,0.81197562492164));
#40682=DIRECTION('center_axis',(0.,-0.911479343942639,0.411345846661781));
#40683=DIRECTION('ref_axis',(0.,-0.411345846661781,-0.911479343942639));
#40684=DIRECTION('center_axis',(0.,-0.5,-0.866025403784439));
#40685=DIRECTION('ref_axis',(0.,0.866025403784439,-0.5));
#40686=DIRECTION('center_axis',(0.561006631580433,-0.762818788136164,-0.321526135468411));
#40687=DIRECTION('ref_axis',(-0.49724715095984,0.,-0.867608938901808));
#40688=DIRECTION('',(0.705516335778299,0.643766472946357,-0.296329931428078));
#40689=DIRECTION('',(0.,-0.388405102597364,0.921488728241605));
#40690=DIRECTION('',(-0.705516335778299,-0.23741171433011,-0.667744245837282));
#40691=DIRECTION('center_axis',(0.561006631580399,0.244027156056944,-0.791026109827972));
#40692=DIRECTION('ref_axis',(-0.815685591418258,0.,-0.578495476173018));
#40693=DIRECTION('',(0.705516335778309,0.358916460582513,0.611085652157592));
#40694=DIRECTION('',(0.,-0.955563307154869,-0.294785966455749));
#40695=DIRECTION('',(-0.705516335778307,0.640807009641837,-0.302676520965598));
#40696=DIRECTION('center_axis',(-0.56100663158041,-0.762818788136182,-0.321526135468408));
#40697=DIRECTION('ref_axis',(-0.497247150959853,0.,0.867608938901801));
#40698=DIRECTION('',(0.,0.388405102597364,-0.921488728241605));
#40699=DIRECTION('',(0.705516335778301,-0.643766472946344,0.296329931428102));
#40700=DIRECTION('',(-0.705516335778315,0.237411714330102,0.667744245837269));
#40701=DIRECTION('center_axis',(-0.707106781186556,-0.667411250860817,0.233585577946044));
#40702=DIRECTION('ref_axis',(0.313668483594035,0.,0.949532559947166));
#40703=DIRECTION('',(0.,-0.330339892306057,-0.943862042647771));
#40704=DIRECTION('',(0.,0.330339892306057,0.943862042647771));
#40705=DIRECTION('center_axis',(-0.561006631580381,0.244027156056947,-0.791026109827984));
#40706=DIRECTION('ref_axis',(-0.815685591418271,0.,0.578495476173));
#40707=DIRECTION('',(0.705516335778325,-0.358916460582507,-0.611085652157578));
#40708=DIRECTION('',(-0.705516335778308,-0.640807009641848,0.302676520965572));
#40709=DIRECTION('',(0.,0.955563307154869,0.294785966455749));
#40710=DIRECTION('center_axis',(-0.707106781186546,0.607940616597039,-0.361120764691834));
#40711=DIRECTION('ref_axis',(-0.454822071931222,0.,0.890582327965354));
#40712=DIRECTION('',(0.,-0.510701883081733,-0.859757865108992));
#40713=DIRECTION('',(0.,0.510701883081733,0.859757865108992));
#40714=DIRECTION('center_axis',(0.,0.294785966455749,-0.955563307154869));
#40715=DIRECTION('ref_axis',(-1.,0.,0.));
#40716=DIRECTION('',(-1.,0.,0.));
#40717=DIRECTION('',(1.,0.,0.));
#40718=DIRECTION('center_axis',(-0.707106781186538,-0.298836238730124,-0.640856382055797));
#40719=DIRECTION('ref_axis',(-0.671542934237828,0.,0.74096564527328));
#40720=DIRECTION('',(0.,-0.90630778703665,0.422618261740699));
#40721=DIRECTION('',(0.,0.90630778703665,-0.422618261740699));
#40722=DIRECTION('center_axis',(0.,-0.921488728241605,-0.388405102597364));
#40723=DIRECTION('ref_axis',(0.,0.388405102597364,-0.921488728241605));
#40724=DIRECTION('',(-1.,0.,0.));
#40725=DIRECTION('',(1.,0.,0.));
#40726=DIRECTION('center_axis',(0.707106781186547,0.607940616597037,-0.361120764691833));
#40727=DIRECTION('ref_axis',(-0.454822071931221,0.,-0.890582327965355));
#40728=DIRECTION('',(0.,-0.510701883081733,-0.859757865108992));
#40729=DIRECTION('',(0.,0.510701883081733,0.859757865108992));
#40730=DIRECTION('center_axis',(0.707106781186554,-0.298836238730117,-0.640856382055783));
#40731=DIRECTION('ref_axis',(-0.671542934237811,0.,-0.740965645273295));
#40732=DIRECTION('',(0.,-0.90630778703665,0.422618261740699));
#40733=DIRECTION('',(0.,0.90630778703665,-0.422618261740699));
#40734=DIRECTION('center_axis',(0.707106781186557,-0.667411250860816,0.233585577946044));
#40735=DIRECTION('ref_axis',(0.313668483594033,0.,-0.949532559947167));
#40736=DIRECTION('',(0.,-0.330339892306057,-0.943862042647771));
#40737=DIRECTION('',(0.,0.330339892306057,0.943862042647771));
#40738=DIRECTION('center_axis',(1.,0.,0.));
#40739=DIRECTION('ref_axis',(0.,0.422618261740699,0.90630778703665));
#40740=DIRECTION('center_axis',(0.,-0.943862042647771,0.330339892306057));
#40741=DIRECTION('ref_axis',(0.,-0.330339892306057,-0.943862042647771));
#40742=DIRECTION('center_axis',(0.,-0.422618261740699,-0.90630778703665));
#40743=DIRECTION('ref_axis',(0.,0.90630778703665,-0.422618261740699));
#40744=DIRECTION('center_axis',(0.561006631580418,0.312041027189173,-0.766747648626013));
#40745=DIRECTION('ref_axis',(-0.807044487383567,0.,-0.590490639539523));
#40746=DIRECTION('',(0.705516335778306,0.304291051193903,0.640041917465772));
#40747=DIRECTION('',(0.,-0.926234810420659,-0.376947046632555));
#40748=DIRECTION('',(-0.705516335778304,0.66474854250225,-0.245674734539573));
#40749=DIRECTION('center_axis',(0.,0.376947046632555,-0.926234810420659));
#40750=DIRECTION('ref_axis',(-1.,0.,0.));
#40751=DIRECTION('',(0.557191914001246,0.769130334536836,0.31301070184082));
#40752=DIRECTION('',(1.,0.,0.));
#40753=DIRECTION('',(-1.,0.,0.));
#40754=DIRECTION('',(-0.557191914001243,0.769130334536838,0.313010701840821));
#40755=DIRECTION('center_axis',(0.707106781186549,0.637100967476913,-0.306761075170856));
#40756=DIRECTION('ref_axis',(-0.397987666358442,0.,-0.917390765937047));
#40757=DIRECTION('',(0.,-0.433825672914778,-0.900996828806872));
#40758=DIRECTION('',(0.,0.433825672914778,0.900996828806872));
#40759=DIRECTION('center_axis',(0.561006631580401,-0.731893183196504,-0.386786669513441));
#40760=DIRECTION('ref_axis',(-0.567619122871708,0.,-0.823291279773054));
#40761=DIRECTION('',(0.70551633577831,0.667143602430344,-0.23909436146888));
#40762=DIRECTION('',(0.,-0.467240138462762,0.884130450221741));
#40763=DIRECTION('',(-0.705516335778305,-0.178310545369065,-0.685895071683811));
#40764=DIRECTION('center_axis',(0.,-0.884130450221741,-0.467240138462762));
#40765=DIRECTION('ref_axis',(0.,0.467240138462762,-0.884130450221741));
#40766=DIRECTION('',(0.557191914001245,0.387988617963615,-0.734167558056275));
#40767=DIRECTION('',(1.,0.,0.));
#40768=DIRECTION('',(-1.,0.,0.));
#40769=DIRECTION('',(-0.557191914001248,0.387988617963614,-0.734167558056273));
#40770=DIRECTION('center_axis',(0.707106781186551,-0.241844762647974,-0.664463024388671));
#40771=DIRECTION('ref_axis',(-0.684791078771732,0.,-0.728739444818686));
#40772=DIRECTION('',(0.,-0.939692620785908,0.342020143325669));
#40773=DIRECTION('',(0.,0.939692620785908,-0.342020143325669));
#40774=DIRECTION('center_axis',(0.70710678118654,-0.68522987409537,0.174527991013631));
#40775=DIRECTION('ref_axis',(0.239628661022762,0.,-0.97086461714105));
#40776=DIRECTION('',(0.,-0.246819851905204,-0.96906138128887));
#40777=DIRECTION('',(0.,0.246819851905204,0.96906138128887));
#40778=DIRECTION('center_axis',(-0.707106781186541,0.63710096747692,-0.30676107517086));
#40779=DIRECTION('ref_axis',(-0.397987666358449,0.,0.917390765937044));
#40780=DIRECTION('',(-0.595596683047422,-0.3027953921519,0.744029261275715));
#40781=DIRECTION('',(0.,0.433825672914778,0.900996828806872));
#40782=DIRECTION('',(0.,-0.433825672914778,-0.900996828806872));
#40783=DIRECTION('center_axis',(0.,-0.342020143325669,-0.939692620785908));
#40784=DIRECTION('ref_axis',(0.,0.939692620785908,-0.342020143325669));
#40785=DIRECTION('',(0.,-0.939692620785908,0.342020143325669));
#40786=DIRECTION('center_axis',(-0.70710678118655,-0.241844762647975,-0.664463024388673));
#40787=DIRECTION('ref_axis',(-0.684791078771734,0.,0.728739444818685));
#40788=DIRECTION('',(0.595596683047427,-0.710207517952258,-0.375326354772744));
#40789=DIRECTION('',(0.,0.939692620785908,-0.342020143325669));
#40790=DIRECTION('center_axis',(-0.707106781186539,-0.685229874095371,0.174527991013632));
#40791=DIRECTION('ref_axis',(0.239628661022763,0.,0.97086461714105));
#40792=DIRECTION('',(0.,0.246819851905204,0.96906138128887));
#40793=DIRECTION('',(0.,-0.246819851905204,-0.96906138128887));
#40794=DIRECTION('center_axis',(0.,-0.96906138128887,0.246819851905204));
#40795=DIRECTION('ref_axis',(0.,-0.246819851905204,-0.96906138128887));
#40796=DIRECTION('center_axis',(0.,0.900996828806872,-0.433825672914778));
#40797=DIRECTION('ref_axis',(0.,0.433825672914778,0.900996828806872));
#40798=DIRECTION('center_axis',(0.561006631580406,-0.695397429203504,-0.449103523455299));
#40799=DIRECTION('ref_axis',(-0.624948053917885,0.,-0.780666337114806));
#40800=DIRECTION('',(0.705516335778305,0.685443366267539,-0.18003913904976));
#40801=DIRECTION('',(0.,-0.542519194747163,0.84004340562312));
#40802=DIRECTION('',(-0.705516335778305,-0.117852325490949,-0.698825821880052));
#40803=DIRECTION('center_axis',(0.561006631580393,0.37768007768899,-0.736633774843144));
#40804=DIRECTION('ref_axis',(-0.795555689966286,0.,-0.605880470193806));
#40805=DIRECTION('',(0.705516335778306,0.2473498031698,0.664127077314135));
#40806=DIRECTION('',(0.,-0.889857107503274,-0.456239332177649));
#40807=DIRECTION('',(-0.705516335778306,0.683630937568096,-0.186803215041171));
#40808=DIRECTION('center_axis',(-0.561006631580404,-0.695397429203505,-0.4491035234553));
#40809=DIRECTION('ref_axis',(-0.624948053917886,0.,0.780666337114805));
#40810=DIRECTION('',(0.,0.542519194747163,-0.84004340562312));
#40811=DIRECTION('',(0.705516335778306,-0.685443366267538,0.180039139049759));
#40812=DIRECTION('',(-0.705516335778306,0.117852325490948,0.69882582188005));
#40813=DIRECTION('center_axis',(-0.707106781186546,-0.697833484234925,0.114142140686716));
#40814=DIRECTION('ref_axis',(0.159358523666365,0.,0.987220776186805));
#40815=DIRECTION('',(0.,-0.161421363397452,-0.986885577683101));
#40816=DIRECTION('',(0.,0.161421363397452,0.986885577683101));
#40817=DIRECTION('center_axis',(-0.561006631580394,0.37768007768899,-0.736633774843143));
#40818=DIRECTION('ref_axis',(-0.795555689966285,0.,0.605880470193806));
#40819=DIRECTION('',(0.705516335778308,-0.247349803169793,-0.664127077314134));
#40820=DIRECTION('',(-0.705516335778305,-0.683630937568098,0.18680321504117));
#40821=DIRECTION('',(0.,0.889857107503274,0.456239332177649));
#40822=DIRECTION('center_axis',(-0.707106781186547,0.66141259530221,-0.250066748640429));
#40823=DIRECTION('ref_axis',(-0.333412439312661,0.,0.942781069661234));
#40824=DIRECTION('',(0.,-0.353647787425838,-0.935378662600772));
#40825=DIRECTION('',(0.,0.353647787425838,0.935378662600772));
#40826=DIRECTION('center_axis',(0.,0.456239332177649,-0.889857107503274));
#40827=DIRECTION('ref_axis',(-1.,0.,0.));
#40828=DIRECTION('',(-1.,0.,0.));
#40829=DIRECTION('',(1.,0.,0.));
#40830=DIRECTION('center_axis',(-0.707106781186551,-0.183012701892219,-0.683012701892216));
#40831=DIRECTION('ref_axis',(-0.694746590606862,0.,0.719254596676407));
#40832=DIRECTION('',(0.,-0.965925826289068,0.258819045102521));
#40833=DIRECTION('',(0.,0.965925826289068,-0.258819045102521));
#40834=DIRECTION('center_axis',(0.,-0.84004340562312,-0.542519194747163));
#40835=DIRECTION('ref_axis',(-1.,0.,0.));
#40836=DIRECTION('',(-1.,0.,0.));
#40837=DIRECTION('',(1.,0.,0.));
#40838=DIRECTION('center_axis',(0.707106781186545,0.661412595302212,-0.25006674864043));
#40839=DIRECTION('ref_axis',(-0.333412439312663,0.,-0.942781069661234));
#40840=DIRECTION('',(0.,-0.353647787425838,-0.935378662600772));
#40841=DIRECTION('',(0.,0.353647787425838,0.935378662600772));
#40842=DIRECTION('center_axis',(0.707106781186552,-0.183012701892218,-0.683012701892215));
#40843=DIRECTION('ref_axis',(-0.694746590606861,0.,-0.719254596676409));
#40844=DIRECTION('',(0.,-0.965925826289068,0.258819045102521));
#40845=DIRECTION('',(0.,0.965925826289068,-0.258819045102521));
#40846=DIRECTION('center_axis',(0.707106781186548,-0.697833484234924,0.114142140686716));
#40847=DIRECTION('ref_axis',(0.159358523666364,0.,-0.987220776186805));
#40848=DIRECTION('',(0.,-0.161421363397452,-0.986885577683101));
#40849=DIRECTION('',(0.,0.161421363397452,0.986885577683101));
#40850=DIRECTION('center_axis',(1.,0.,0.));
#40851=DIRECTION('ref_axis',(0.,0.258819045102521,0.965925826289068));
#40852=DIRECTION('center_axis',(0.,-0.986885577683101,0.161421363397451));
#40853=DIRECTION('ref_axis',(0.,-0.161421363397452,-0.986885577683101));
#40854=DIRECTION('center_axis',(0.,-0.258819045102521,-0.965925826289068));
#40855=DIRECTION('ref_axis',(0.,0.965925826289068,-0.258819045102521));
#40856=DIRECTION('center_axis',(0.5610066315804,-0.65360928088183,-0.508002428407533));
#40857=DIRECTION('ref_axis',(-0.671222048820188,0.,-0.741256339721711));
#40858=DIRECTION('',(0.7055163357783,0.698526492205412,-0.119613710071894));
#40859=DIRECTION('',(0.,-0.613669352377477,0.78956312347564));
#40860=DIRECTION('',(-0.70551633577831,-0.0564971782546714,-0.706438085609211));
#40861=DIRECTION('center_axis',(0.561006631580382,0.440444754748134,-0.700913673242068));
#40862=DIRECTION('ref_axis',(-0.78071899035428,0.,-0.624882275392889));
#40863=DIRECTION('',(0.705516335778309,0.188526073789639,0.683157829093257));
#40864=DIRECTION('',(0.,-0.846707054687368,-0.532059360920041));
#40865=DIRECTION('',(-0.705516335778306,0.697310488411396,-0.126510010281449));
#40866=DIRECTION('center_axis',(-0.561006631580414,-0.653609280881823,-0.508002428407526));
#40867=DIRECTION('ref_axis',(-0.671222048820174,0.,0.741256339721724));
#40868=DIRECTION('',(0.,0.613669352377477,-0.78956312347564));
#40869=DIRECTION('',(0.705516335778301,-0.698526492205416,0.119613710071868));
#40870=DIRECTION('',(-0.705516335778299,0.0564971782546765,0.706438085609222));
#40871=DIRECTION('center_axis',(-0.707106781186551,-0.705126160196076,0.0528875997482672));
#40872=DIRECTION('ref_axis',(0.0745860273602096,0.,0.997214582987344));
#40873=DIRECTION('',(0.,-0.0747943608453598,-0.997198978933359));
#40874=DIRECTION('',(0.,0.0747943608453598,0.997198978933359));
#40875=DIRECTION('center_axis',(-0.561006631580395,0.44044475474813,-0.700913673242061));
#40876=DIRECTION('ref_axis',(-0.78071899035427,0.,0.624882275392901));
#40877=DIRECTION('',(0.705516335778298,-0.188526073789641,-0.683157829093268));
#40878=DIRECTION('',(-0.705516335778309,-0.697310488411389,0.126510010281474));
#40879=DIRECTION('',(0.,0.846707054687368,0.532059360920041));
#40880=DIRECTION('center_axis',(-0.707106781186541,0.680690473905417,-0.191469263158418));
#40881=DIRECTION('ref_axis',(-0.261366100937227,0.,0.965239742903736));
#40882=DIRECTION('',(0.,-0.270778428736216,-0.962641699975202));
#40883=DIRECTION('',(0.,0.270778428736216,0.962641699975202));
#40884=DIRECTION('center_axis',(0.,0.532059360920041,-0.846707054687368));
#40885=DIRECTION('ref_axis',(-1.,0.,0.));
#40886=DIRECTION('',(-1.,0.,0.));
#40887=DIRECTION('',(1.,0.,0.));
#40888=DIRECTION('center_axis',(-0.707106781186554,-0.122787803968972,-0.696364240320013));
#40889=DIRECTION('ref_axis',(-0.701673843159857,0.,0.712498293208676));
#40890=DIRECTION('',(0.,-0.984807753012208,0.173648177666931));
#40891=DIRECTION('',(0.,0.984807753012208,-0.173648177666931));
#40892=DIRECTION('center_axis',(0.,-0.78956312347564,-0.613669352377477));
#40893=DIRECTION('ref_axis',(-1.,0.,0.));
#40894=DIRECTION('',(-1.,0.,0.));
#40895=DIRECTION('',(1.,0.,0.));
#40896=DIRECTION('center_axis',(0.707106781186543,0.680690473905416,-0.191469263158418));
#40897=DIRECTION('ref_axis',(-0.261366100937226,0.,-0.965239742903737));
#40898=DIRECTION('',(0.,-0.270778428736216,-0.962641699975202));
#40899=DIRECTION('',(0.,0.270778428736216,0.962641699975202));
#40900=DIRECTION('center_axis',(0.707106781186542,-0.122787803968974,-0.696364240320024));
#40901=DIRECTION('ref_axis',(-0.701673843159868,0.,-0.712498293208665));
#40902=DIRECTION('',(0.,-0.984807753012208,0.173648177666931));
#40903=DIRECTION('',(0.,0.984807753012208,-0.173648177666931));
#40904=DIRECTION('center_axis',(0.707106781186553,-0.705126160196074,0.0528875997482671));
#40905=DIRECTION('ref_axis',(0.0745860273602093,0.,-0.997214582987344));
#40906=DIRECTION('',(0.,-0.0747943608453598,-0.997198978933359));
#40907=DIRECTION('',(0.,0.0747943608453598,0.997198978933359));
#40908=DIRECTION('center_axis',(1.,0.,0.));
#40909=DIRECTION('ref_axis',(0.,0.173648177666931,0.984807753012208));
#40910=DIRECTION('center_axis',(0.,-0.997198978933359,0.0747943608453598));
#40911=DIRECTION('ref_axis',(0.,-0.0747943608453598,-0.997198978933359));
#40912=DIRECTION('center_axis',(0.,-0.173648177666931,-0.984807753012208));
#40913=DIRECTION('ref_axis',(0.,0.984807753012208,-0.173648177666931));
#40914=DIRECTION('center_axis',(0.707106781186549,-0.707052400311325,-0.00876944775867129));
#40915=DIRECTION('ref_axis',(-0.0124009183210272,0.,-0.999923105656027));
#40916=DIRECTION('',(0.595596683047425,0.588866174870653,0.546352650982962));
#40917=DIRECTION('',(0.,-0.0124018719548353,0.999923093828728));
#40918=DIRECTION('',(0.,0.0124018719548353,-0.999923093828728));
#40919=DIRECTION('',(0.557191914001238,0.564784772718638,-0.608732561538146));
#40920=DIRECTION('center_axis',(1.,0.,0.));
#40921=DIRECTION('ref_axis',(0.,0.0871557427476582,0.996194698091746));
#40922=DIRECTION('',(0.,-0.996194698091746,0.0871557427476582));
#40923=DIRECTION('',(0.,-0.185848282703424,-0.982578452753869));
#40924=DIRECTION('center_axis',(0.707106781186545,-0.0616284167162196,-0.704416026402761));
#40925=DIRECTION('ref_axis',(-0.705757556807954,0.,-0.708453436019945));
#40926=DIRECTION('',(0.557191914001255,-0.564784772718631,0.608732561538138));
#40927=DIRECTION('',(0.,0.996194698091746,-0.0871557427476582));
#40928=DIRECTION('',(0.705516335778315,0.128267547152788,0.696989337290999));
#40929=DIRECTION('center_axis',(0.,-0.733073789207257,-0.680149115692518));
#40930=DIRECTION('ref_axis',(-1.,0.,0.));
#40931=DIRECTION('',(-1.,0.,0.));
#40932=DIRECTION('',(0.,0.680149115692518,-0.733073789207257));
#40933=DIRECTION('',(1.,0.,0.));
#40934=DIRECTION('center_axis',(0.561006631580394,0.499857381275784,-0.659859195364387));
#40935=DIRECTION('ref_axis',(-0.761867344215974,0.,-0.64773308531933));
#40936=DIRECTION('',(0.,-0.797113049929625,-0.603830096659557));
#40937=DIRECTION('',(-0.705516335778304,0.70568308539029,-0.0652539879547269));
#40938=DIRECTION('center_axis',(-0.561006631580409,-0.606846771272559,-0.563035128139331));
#40939=DIRECTION('ref_axis',(-0.708381704532385,0.,0.705829554980374));
#40940=DIRECTION('',(0.705516335778303,-0.706293409755775,0.0582779485356021));
#40941=DIRECTION('',(-0.705516335778301,-0.00528794662205795,0.70867392894792));
#40942=DIRECTION('center_axis',(-0.707106781186549,-0.707052400311325,-0.00876944775867129));
#40943=DIRECTION('ref_axis',(-0.0124009183210272,0.,0.999923105656027));
#40944=DIRECTION('',(0.,0.0124018719548353,-0.999923093828728));
#40945=DIRECTION('',(0.,-0.0124018719548353,0.999923093828728));
#40946=DIRECTION('center_axis',(-0.561006631580407,0.499857381275778,-0.65985919536438));
#40947=DIRECTION('ref_axis',(-0.761867344215964,0.,0.647733085319342));
#40948=DIRECTION('',(0.705516335778305,-0.128267547152786,-0.696989337291011));
#40949=DIRECTION('',(-0.705516335778306,-0.705683085390286,0.0652539879547519));
#40950=DIRECTION('',(0.,0.797113049929625,0.603830096659557));
#40951=DIRECTION('center_axis',(-0.707106781186546,0.694787886990048,-0.131414580971466));
#40952=DIRECTION('ref_axis',(-0.182719541232955,0.,0.983165077314903));
#40953=DIRECTION('',(0.,-0.185848282703424,-0.982578452753869));
#40954=DIRECTION('',(0.,0.185848282703424,0.982578452753869));
#40955=DIRECTION('center_axis',(0.,0.603830096659558,-0.797113049929625));
#40956=DIRECTION('ref_axis',(-1.,0.,0.));
#40957=DIRECTION('',(-1.,0.,0.));
#40958=DIRECTION('',(1.,0.,0.));
#40959=DIRECTION('center_axis',(-0.707106781186556,-0.0616284167162186,
-0.70441602640275));
#40960=DIRECTION('ref_axis',(-0.705757556807943,0.,0.708453436019956));
#40961=DIRECTION('',(0.,-0.996194698091746,0.0871557427476582));
#40962=DIRECTION('',(0.,0.996194698091746,-0.0871557427476582));
#40963=DIRECTION('center_axis',(0.707106781186546,0.694787886990048,-0.131414580971466));
#40964=DIRECTION('ref_axis',(-0.182719541232955,0.,-0.983165077314903));
#40965=DIRECTION('',(0.,0.185848282703424,0.982578452753869));
#40966=DIRECTION('center_axis',(0.,-0.999923093828728,-0.0124018719548353));
#40967=DIRECTION('ref_axis',(0.,0.0124018719548353,-0.999923093828728));
#40968=DIRECTION('center_axis',(0.,-0.0871557427476582,-0.996194698091746));
#40969=DIRECTION('ref_axis',(0.,0.996194698091746,-0.0871557427476582));
#40970=DIRECTION('center_axis',(0.561006631580416,-0.555465791309803,-0.613782790576088));
#40971=DIRECTION('ref_axis',(-0.738128342492238,0.,-0.674660321947023));
#40972=DIRECTION('',(0.705516335778304,0.708685007986272,0.00350134337823141));
#40973=DIRECTION('',(0.,-0.741452533551882,0.671005320760942));
#40974=DIRECTION('',(-0.705516335778299,0.0670328270320436,-0.705516335778311));
#40975=DIRECTION('center_axis',(0.561006631580416,0.555465791309803,-0.613782790576088));
#40976=DIRECTION('ref_axis',(-0.738128342492238,0.,-0.674660321947023));
#40977=DIRECTION('',(0.705516335778299,0.0670328270320439,0.705516335778311));
#40978=DIRECTION('',(0.,-0.741452533551882,-0.671005320760943));
#40979=DIRECTION('',(-0.705516335778305,0.708685007986272,-0.00350134337823141));
#40980=DIRECTION('center_axis',(-0.561006631580428,-0.555465791309797,-0.613782790576082));
#40981=DIRECTION('ref_axis',(-0.738128342492228,0.,0.674660321947035));
#40982=DIRECTION('',(0.,0.741452533551882,-0.671005320760942));
#40983=DIRECTION('',(0.705516335778307,-0.708685007986269,-0.00350134337825647));
#40984=DIRECTION('',(-0.705516335778288,-0.0670328270320448,0.705516335778322));
#40985=DIRECTION('center_axis',(-0.707106781186548,-0.703597544730292,-0.070359754473029));
#40986=DIRECTION('ref_axis',(-0.0990147542976672,0.,0.995085965347403));
#40987=DIRECTION('',(0.,0.0995037190209987,-0.995037190209989));
#40988=DIRECTION('',(0.,-0.0995037190209987,0.995037190209989));
#40989=DIRECTION('center_axis',(-0.561006631580428,0.555465791309797,-0.613782790576082));
#40990=DIRECTION('ref_axis',(-0.738128342492227,0.,0.674660321947035));
#40991=DIRECTION('',(0.705516335778288,-0.0670328270320442,-0.705516335778322));
#40992=DIRECTION('',(-0.705516335778307,-0.708685007986269,0.00350134337825648));
#40993=DIRECTION('',(0.,0.741452533551882,0.671005320760943));
#40994=DIRECTION('center_axis',(-0.707106781186548,0.703597544730292,-0.0703597544730292));
#40995=DIRECTION('ref_axis',(-0.0990147542976674,0.,0.995085965347403));
#40996=DIRECTION('',(0.,-0.0995037190209989,-0.995037190209989));
#40997=DIRECTION('',(0.,0.0995037190209989,0.995037190209989));
#40998=DIRECTION('center_axis',(0.,0.671005320760943,-0.741452533551882));
#40999=DIRECTION('ref_axis',(-1.,0.,0.));
#41000=DIRECTION('',(-1.,0.,0.));
#41001=DIRECTION('',(1.,0.,0.));
#41002=DIRECTION('center_axis',(-0.707106781186565,-8.65956056235472E-17,
-0.70710678118653));
#41003=DIRECTION('ref_axis',(-0.70710678118653,0.,0.707106781186565));
#41004=DIRECTION('',(0.,-1.,1.22464679914735E-16));
#41005=DIRECTION('',(0.,1.,-1.22464679914735E-16));
#41006=DIRECTION('center_axis',(0.,-0.671005320760942,-0.741452533551882));
#41007=DIRECTION('ref_axis',(-1.,0.,0.));
#41008=DIRECTION('',(-1.,0.,0.));
#41009=DIRECTION('',(1.,0.,0.));
#41010=DIRECTION('center_axis',(0.707106781186548,0.703597544730291,-0.0703597544730291));
#41011=DIRECTION('ref_axis',(-0.0990147542976671,0.,-0.995085965347403));
#41012=DIRECTION('',(0.,-0.0995037190209989,-0.995037190209989));
#41013=DIRECTION('',(0.,0.0995037190209989,0.995037190209989));
#41014=DIRECTION('center_axis',(0.707106781186554,-8.65956056235486E-17,
-0.707106781186541));
#41015=DIRECTION('ref_axis',(-0.707106781186541,0.,-0.707106781186554));
#41016=DIRECTION('',(0.,-1.,1.22464679914735E-16));
#41017=DIRECTION('',(0.,1.,-1.22464679914735E-16));
#41018=DIRECTION('center_axis',(0.707106781186549,-0.70359754473029,-0.0703597544730288));
#41019=DIRECTION('ref_axis',(-0.0990147542976667,0.,-0.995085965347403));
#41020=DIRECTION('',(0.,0.0995037190209987,-0.995037190209989));
#41021=DIRECTION('',(0.,-0.0995037190209987,0.995037190209989));
#41022=DIRECTION('center_axis',(1.,0.,0.));
#41023=DIRECTION('ref_axis',(0.,1.22464679914735E-16,1.));
#41024=DIRECTION('center_axis',(0.,-0.995037190209989,-0.0995037190209987));
#41025=DIRECTION('ref_axis',(0.,0.0995037190209987,-0.995037190209989));
#41026=DIRECTION('center_axis',(0.,-1.22464679914735E-16,-1.));
#41027=DIRECTION('ref_axis',(0.,1.,-1.22464679914735E-16));
#41028=DIRECTION('center_axis',(0.561006631580408,0.606846771272561,-0.56303512813933));
#41029=DIRECTION('ref_axis',(-0.708381704532385,0.,-0.705829554980374));
#41030=DIRECTION('',(0.7055163357783,0.00528794662205797,0.708673928947921));
#41031=DIRECTION('',(0.,-0.680149115692518,-0.733073789207257));
#41032=DIRECTION('',(-0.705516335778304,0.706293409755774,0.0582779485356025));
#41033=DIRECTION('center_axis',(0.,0.733073789207257,-0.680149115692518));
#41034=DIRECTION('ref_axis',(-1.,0.,0.));
#41035=DIRECTION('',(0.55719191400124,0.564784772718638,0.608732561538145));
#41036=DIRECTION('',(1.,0.,0.));
#41037=DIRECTION('',(-1.,0.,0.));
#41038=DIRECTION('',(-0.557191914001263,0.564784772718627,0.608732561538133));
#41039=DIRECTION('center_axis',(0.707106781186549,0.707052400311325,-0.00876944775867146));
#41040=DIRECTION('ref_axis',(-0.0124009183210275,0.,-0.999923105656027));
#41041=DIRECTION('',(0.,-0.0124018719548356,-0.999923093828728));
#41042=DIRECTION('',(0.,0.0124018719548356,0.999923093828728));
#41043=DIRECTION('center_axis',(0.561006631580409,-0.499857381275773,-0.659859195364382));
#41044=DIRECTION('ref_axis',(-0.761867344215964,0.,-0.647733085319342));
#41045=DIRECTION('',(0.705516335778303,0.705683085390289,0.0652539879547519));
#41046=DIRECTION('',(0.,-0.79711304992963,0.603830096659552));
#41047=DIRECTION('',(-0.705516335778302,0.128267547152795,-0.696989337291011));
#41048=DIRECTION('center_axis',(0.,-0.603830096659552,-0.79711304992963));
#41049=DIRECTION('ref_axis',(-1.,0.,0.));
#41050=DIRECTION('',(0.557191914001257,0.661909722954172,-0.501410699557107));
#41051=DIRECTION('',(1.,0.,0.));
#41052=DIRECTION('',(-1.,0.,0.));
#41053=DIRECTION('',(-0.557191914001246,0.661909722954178,-0.501410699557111));
#41054=DIRECTION('center_axis',(0.707106781186545,0.0616284167162194,-0.704416026402761));
#41055=DIRECTION('ref_axis',(-0.705757556807954,0.,-0.708453436019945));
#41056=DIRECTION('',(0.,-0.996194698091746,-0.0871557427476579));
#41057=DIRECTION('',(0.,0.996194698091746,0.0871557427476579));
#41058=DIRECTION('center_axis',(0.707106781186549,-0.694787886990045,-0.131414580971465));
#41059=DIRECTION('ref_axis',(-0.182719541232953,0.,-0.983165077314903));
#41060=DIRECTION('',(0.,0.185848282703424,-0.98257845275387));
#41061=DIRECTION('',(0.,-0.185848282703424,0.98257845275387));
#41062=DIRECTION('center_axis',(-0.707106781186548,0.707052400311326,-0.00876944775867148));
#41063=DIRECTION('ref_axis',(-0.0124009183210275,0.,0.999923105656027));
#41064=DIRECTION('',(-0.595596683047425,-0.58886617487065,0.546352650982966));
#41065=DIRECTION('',(0.,0.0124018719548356,0.999923093828728));
#41066=DIRECTION('',(0.,-0.0124018719548356,-0.999923093828728));
#41067=DIRECTION('center_axis',(0.,0.0871557427476579,-0.996194698091746));
#41068=DIRECTION('ref_axis',(0.,0.996194698091746,0.0871557427476579));
#41069=DIRECTION('',(0.,-0.996194698091746,-0.0871557427476579));
#41070=DIRECTION('center_axis',(-0.707106781186531,0.0616284167162207,-0.704416026402775));
#41071=DIRECTION('ref_axis',(-0.705757556807969,0.,0.708453436019931));
#41072=DIRECTION('',(0.59559668304743,-0.485046832292573,-0.640307864722775));
#41073=DIRECTION('',(0.,0.996194698091746,0.0871557427476579));
#41074=DIRECTION('center_axis',(-0.707106781186548,-0.694787886990046,-0.131414580971466));
#41075=DIRECTION('ref_axis',(-0.182719541232954,0.,0.983165077314903));
#41076=DIRECTION('',(0.,-0.185848282703424,0.98257845275387));
#41077=DIRECTION('',(0.,0.185848282703424,-0.98257845275387));
#41078=DIRECTION('center_axis',(0.,-0.98257845275387,-0.185848282703424));
#41079=DIRECTION('ref_axis',(0.,0.185848282703424,-0.98257845275387));
#41080=DIRECTION('center_axis',(0.,0.999923093828728,-0.0124018719548356));
#41081=DIRECTION('ref_axis',(0.,0.0124018719548356,0.999923093828728));
#41082=DIRECTION('center_axis',(0.561006631580393,-0.440444754748104,-0.700913673242079));
#41083=DIRECTION('ref_axis',(-0.780718990354279,0.,-0.62488227539289));
#41084=DIRECTION('',(0.705516335778308,0.697310488411385,0.1265100102815));
#41085=DIRECTION('',(0.,-0.846707054687388,0.532059360920009));
#41086=DIRECTION('',(-0.705516335778307,0.188526073789657,-0.683157829093255));
#41087=DIRECTION('center_axis',(0.561006631580402,0.653609280881817,-0.508002428407548));
#41088=DIRECTION('ref_axis',(-0.671222048820198,0.,-0.741256339721703));
#41089=DIRECTION('',(0.70551633577831,-0.0564971782546651,0.706438085609211));
#41090=DIRECTION('',(0.,-0.613669352377496,-0.789563123475625));
#41091=DIRECTION('',(-0.705516335778302,0.698526492205414,0.119613710071869));
#41092=DIRECTION('center_axis',(-0.56100663158039,-0.440444754748103,-0.700913673242082));
#41093=DIRECTION('ref_axis',(-0.780718990354282,0.,0.624882275392886));
#41094=DIRECTION('',(0.,0.846707054687388,-0.532059360920009));
#41095=DIRECTION('',(0.705516335778313,-0.697310488411381,-0.1265100102815));
#41096=DIRECTION('',(-0.705516335778307,-0.188526073789662,0.683157829093252));
#41097=DIRECTION('center_axis',(-0.707106781186538,-0.68069047390542,-0.191469263158418));
#41098=DIRECTION('ref_axis',(-0.261366100937229,0.,0.965239742903736));
#41099=DIRECTION('',(0.,0.270778428736215,-0.962641699975202));
#41100=DIRECTION('',(0.,-0.270778428736215,0.962641699975202));
#41101=DIRECTION('center_axis',(-0.561006631580396,0.65360928088182,-0.50800242840755));
#41102=DIRECTION('ref_axis',(-0.671222048820203,0.,0.741256339721698));
#41103=DIRECTION('',(0.705516335778312,0.0564971782546587,-0.70643808560921));
#41104=DIRECTION('',(-0.705516335778307,-0.69852649220541,-0.119613710071869));
#41105=DIRECTION('',(0.,0.613669352377496,0.789563123475625));
#41106=DIRECTION('center_axis',(-0.707106781186545,0.705126160196082,0.0528875997482672));
#41107=DIRECTION('ref_axis',(0.0745860273602103,0.,0.997214582987344));
#41108=DIRECTION('',(0.,0.0747943608453591,-0.997198978933359));
#41109=DIRECTION('',(0.,-0.0747943608453591,0.997198978933359));
#41110=DIRECTION('center_axis',(0.,0.789563123475625,-0.613669352377496));
#41111=DIRECTION('ref_axis',(-1.,0.,0.));
#41112=DIRECTION('',(-1.,0.,0.));
#41113=DIRECTION('',(1.,0.,0.));
#41114=DIRECTION('center_axis',(-0.707106781186541,0.122787803968974,-0.696364240320025));
#41115=DIRECTION('ref_axis',(-0.701673843159869,0.,0.712498293208664));
#41116=DIRECTION('',(0.,-0.984807753012208,-0.17364817766693));
#41117=DIRECTION('',(0.,0.984807753012208,0.17364817766693));
#41118=DIRECTION('center_axis',(0.,-0.532059360920009,-0.846707054687388));
#41119=DIRECTION('ref_axis',(-1.,0.,0.));
#41120=DIRECTION('',(-1.,0.,0.));
#41121=DIRECTION('',(1.,0.,0.));
#41122=DIRECTION('center_axis',(0.70710678118655,0.705126160196078,0.0528875997482669));
#41123=DIRECTION('ref_axis',(0.0745860273602093,0.,-0.997214582987344));
#41124=DIRECTION('',(0.,0.0747943608453591,-0.997198978933359));
#41125=DIRECTION('',(0.,-0.0747943608453591,0.997198978933359));
#41126=DIRECTION('center_axis',(0.707106781186543,0.122787803968973,-0.696364240320023));
#41127=DIRECTION('ref_axis',(-0.701673843159868,0.,-0.712498293208665));
#41128=DIRECTION('',(0.,-0.984807753012208,-0.17364817766693));
#41129=DIRECTION('',(0.,0.984807753012208,0.17364817766693));
#41130=DIRECTION('center_axis',(0.707106781186543,-0.680690473905416,-0.191469263158417));
#41131=DIRECTION('ref_axis',(-0.261366100937225,0.,-0.965239742903737));
#41132=DIRECTION('',(0.,0.270778428736215,-0.962641699975202));
#41133=DIRECTION('',(0.,-0.270778428736215,0.962641699975202));
#41134=DIRECTION('center_axis',(1.,0.,0.));
#41135=DIRECTION('ref_axis',(0.,-0.17364817766693,0.984807753012208));
#41136=DIRECTION('center_axis',(0.,-0.962641699975202,-0.270778428736215));
#41137=DIRECTION('ref_axis',(0.,0.270778428736215,-0.962641699975202));
#41138=DIRECTION('center_axis',(0.,0.17364817766693,-0.984807753012208));
#41139=DIRECTION('ref_axis',(0.,0.984807753012208,0.17364817766693));
#41140=DIRECTION('center_axis',(0.561006631580395,-0.37768007768897,-0.736633774843153));
#41141=DIRECTION('ref_axis',(-0.795555689966288,0.,-0.605880470193802));
#41142=DIRECTION('',(0.705516335778309,0.683630937568086,0.186803215041197));
#41143=DIRECTION('',(0.,-0.889857107503286,0.456239332177625));
#41144=DIRECTION('',(-0.705516335778301,0.247349803169823,-0.664127077314131));
#41145=DIRECTION('center_axis',(0.56100663158043,0.695397429203484,-0.449103523455299));
#41146=DIRECTION('ref_axis',(-0.624948053917868,0.,-0.78066633711482));
#41147=DIRECTION('',(0.705516335778292,-0.117852325490953,0.698825821880064));
#41148=DIRECTION('',(0.,-0.542519194747174,-0.840043405623113));
#41149=DIRECTION('',(-0.705516335778305,0.685443366267552,0.18003913904971));
#41150=DIRECTION('center_axis',(-0.561006631580394,-0.37768007768897,-0.736633774843153));
#41151=DIRECTION('ref_axis',(-0.795555689966289,0.,0.605880470193801));
#41152=DIRECTION('',(0.,0.889857107503286,-0.456239332177625));
#41153=DIRECTION('',(0.705516335778311,-0.683630937568085,-0.186803215041197));
#41154=DIRECTION('',(-0.705516335778303,-0.247349803169823,0.664127077314129));
#41155=DIRECTION('center_axis',(-0.707106781186544,-0.661412595302213,-0.25006674864043));
#41156=DIRECTION('ref_axis',(-0.333412439312664,0.,0.942781069661233));
#41157=DIRECTION('',(0.,0.353647787425838,-0.935378662600772));
#41158=DIRECTION('',(0.,-0.353647787425838,0.935378662600772));
#41159=DIRECTION('center_axis',(-0.561006631580425,0.695397429203487,-0.449103523455301));
#41160=DIRECTION('ref_axis',(-0.624948053917874,0.,0.780666337114815));
#41161=DIRECTION('',(0.705516335778293,0.117852325490952,-0.698825821880063));
#41162=DIRECTION('',(-0.70551633577831,-0.685443366267547,-0.18003913904971));
#41163=DIRECTION('',(0.,0.542519194747174,0.840043405623113));
#41164=DIRECTION('center_axis',(-0.707106781186546,0.697833484234925,0.114142140686716));
#41165=DIRECTION('ref_axis',(0.159358523666365,0.,0.987220776186805));
#41166=DIRECTION('',(0.,0.161421363397451,-0.986885577683101));
#41167=DIRECTION('',(0.,-0.161421363397451,0.986885577683101));
#41168=DIRECTION('center_axis',(0.,0.840043405623113,-0.542519194747174));
#41169=DIRECTION('ref_axis',(-1.,0.,0.));
#41170=DIRECTION('',(-1.,0.,0.));
#41171=DIRECTION('',(1.,0.,0.));
#41172=DIRECTION('center_axis',(-0.707106781186552,0.183012701892218,-0.683012701892215));
#41173=DIRECTION('ref_axis',(-0.694746590606862,0.,0.719254596676408));
#41174=DIRECTION('',(0.,-0.965925826289068,-0.258819045102521));
#41175=DIRECTION('',(0.,0.965925826289068,0.258819045102521));
#41176=DIRECTION('center_axis',(0.,-0.456239332177625,-0.889857107503286));
#41177=DIRECTION('ref_axis',(-1.,0.,0.));
#41178=DIRECTION('',(-1.,0.,0.));
#41179=DIRECTION('',(1.,0.,0.));
#41180=DIRECTION('center_axis',(0.707106781186551,0.697833484234921,0.114142140686715));
#41181=DIRECTION('ref_axis',(0.159358523666362,0.,-0.987220776186805));
#41182=DIRECTION('',(0.,0.161421363397451,-0.986885577683101));
#41183=DIRECTION('',(0.,-0.161421363397451,0.986885577683101));
#41184=DIRECTION('center_axis',(0.707106781186553,0.183012701892218,-0.683012701892214));
#41185=DIRECTION('ref_axis',(-0.69474659060686,0.,-0.719254596676409));
#41186=DIRECTION('',(0.,-0.965925826289068,-0.258819045102521));
#41187=DIRECTION('',(0.,0.965925826289068,0.258819045102521));
#41188=DIRECTION('center_axis',(0.707106781186545,-0.661412595302212,-0.25006674864043));
#41189=DIRECTION('ref_axis',(-0.333412439312663,0.,-0.942781069661234));
#41190=DIRECTION('',(0.,0.353647787425838,-0.935378662600772));
#41191=DIRECTION('',(0.,-0.353647787425838,0.935378662600772));
#41192=DIRECTION('center_axis',(1.,0.,0.));
#41193=DIRECTION('ref_axis',(0.,-0.258819045102521,0.965925826289068));
#41194=DIRECTION('center_axis',(0.,-0.935378662600772,-0.353647787425838));
#41195=DIRECTION('ref_axis',(0.,0.353647787425838,-0.935378662600772));
#41196=DIRECTION('center_axis',(0.,0.258819045102521,-0.965925826289068));
#41197=DIRECTION('ref_axis',(0.,0.965925826289068,0.258819045102521));
#41198=DIRECTION('center_axis',(0.707106781186549,-0.637100967476913,-0.306761075170856));
#41199=DIRECTION('ref_axis',(-0.397987666358442,0.,-0.917390765937047));
#41200=DIRECTION('',(0.595596683047422,0.302795392151909,0.744029261275711));
#41201=DIRECTION('',(0.,-0.433825672914778,0.900996828806872));
#41202=DIRECTION('',(0.,0.433825672914778,-0.900996828806872));
#41203=DIRECTION('',(0.557191914001242,0.769130334536841,-0.313010701840814));
#41204=DIRECTION('center_axis',(1.,0.,0.));
#41205=DIRECTION('ref_axis',(0.,-0.342020143325669,0.939692620785909));
#41206=DIRECTION('',(0.,-0.939692620785909,-0.342020143325669));
#41207=DIRECTION('',(0.,0.246819851905204,-0.96906138128887));
#41208=DIRECTION('center_axis',(0.707106781186551,0.241844762647974,-0.664463024388671));
#41209=DIRECTION('ref_axis',(-0.684791078771732,0.,-0.728739444818686));
#41210=DIRECTION('',(0.557191914001232,-0.769130334536847,0.313010701840817));
#41211=DIRECTION('',(0.,0.939692620785909,0.342020143325669));
#41212=DIRECTION('',(0.705516335778307,-0.178310545369053,0.685895071683813));
#41213=DIRECTION('center_axis',(0.,-0.376947046632547,-0.926234810420662));
#41214=DIRECTION('ref_axis',(-1.,0.,0.));
#41215=DIRECTION('',(-1.,0.,0.));
#41216=DIRECTION('',(0.,0.926234810420662,-0.376947046632547));
#41217=DIRECTION('',(1.,0.,0.));
#41218=DIRECTION('center_axis',(0.561006631580392,0.73189318319651,-0.386786669513444));
#41219=DIRECTION('ref_axis',(-0.567619122871716,0.,-0.823291279773048));
#41220=DIRECTION('',(0.,-0.467240138462762,-0.884130450221741));
#41221=DIRECTION('',(-0.705516335778315,0.667143602430337,0.239094361468882));
#41222=DIRECTION('center_axis',(-0.561006631580397,-0.312041027189172,-0.766747648626028));
#41223=DIRECTION('ref_axis',(-0.807044487383583,0.,0.590490639539502));
#41224=DIRECTION('',(0.705516335778304,-0.66474854250226,-0.245674734539547));
#41225=DIRECTION('',(-0.705516335778316,-0.304291051193919,0.640041917465754));
#41226=DIRECTION('center_axis',(-0.707106781186553,-0.637100967476909,-0.306761075170854));
#41227=DIRECTION('ref_axis',(-0.397987666358438,0.,0.917390765937049));
#41228=DIRECTION('',(0.,0.433825672914778,-0.900996828806872));
#41229=DIRECTION('',(0.,-0.433825672914778,0.900996828806872));
#41230=DIRECTION('center_axis',(-0.561006631580381,0.731893183196516,-0.386786669513448));
#41231=DIRECTION('ref_axis',(-0.567619122871728,0.,0.82329127977304));
#41232=DIRECTION('',(0.70551633577832,0.178310545369055,-0.685895071683798));
#41233=DIRECTION('',(-0.705516335778313,-0.667143602430331,-0.239094361468905));
#41234=DIRECTION('',(0.,0.467240138462762,0.884130450221741));
#41235=DIRECTION('center_axis',(-0.707106781186533,0.685229874095377,0.174527991013633));
#41236=DIRECTION('ref_axis',(0.239628661022767,0.,0.970864617141049));
#41237=DIRECTION('',(0.,0.246819851905204,-0.96906138128887));
#41238=DIRECTION('',(0.,-0.246819851905204,0.96906138128887));
#41239=DIRECTION('center_axis',(0.,0.884130450221741,-0.467240138462762));
#41240=DIRECTION('ref_axis',(0.,0.467240138462762,0.884130450221741));
#41241=DIRECTION('',(-1.,0.,0.));
#41242=DIRECTION('',(1.,0.,0.));
#41243=DIRECTION('center_axis',(-0.707106781186536,0.241844762647979,-0.664463024388686));
#41244=DIRECTION('ref_axis',(-0.684791078771748,0.,0.728739444818671));
#41245=DIRECTION('',(0.,-0.939692620785909,-0.342020143325669));
#41246=DIRECTION('',(0.,0.939692620785909,0.342020143325669));
#41247=DIRECTION('center_axis',(0.707106781186534,0.685229874095376,0.174527991013633));
#41248=DIRECTION('ref_axis',(0.239628661022766,0.,-0.970864617141049));
#41249=DIRECTION('',(0.,-0.246819851905204,0.96906138128887));
#41250=DIRECTION('center_axis',(0.,-0.900996828806872,-0.433825672914778));
#41251=DIRECTION('ref_axis',(0.,0.433825672914778,-0.900996828806872));
#41252=DIRECTION('center_axis',(0.,0.342020143325669,-0.939692620785908));
#41253=DIRECTION('ref_axis',(0.,0.939692620785909,0.342020143325669));
#41254=DIRECTION('center_axis',(0.561006631580397,-0.244027156056947,-0.791026109827972));
#41255=DIRECTION('ref_axis',(-0.815685591418259,0.,-0.578495476173017));
#41256=DIRECTION('',(0.705516335778307,0.640807009641837,0.302676520965598));
#41257=DIRECTION('',(0.,-0.955563307154868,0.294785966455752));
#41258=DIRECTION('',(-0.705516335778309,0.358916460582513,-0.611085652157592));
#41259=DIRECTION('center_axis',(0.561006631580416,0.762818788136174,-0.321526135468415));
#41260=DIRECTION('ref_axis',(-0.497247150959857,0.,-0.867608938901799));
#41261=DIRECTION('',(0.705516335778299,-0.23741171433011,0.667744245837282));
#41262=DIRECTION('',(0.,-0.388405102597364,-0.921488728241605));
#41263=DIRECTION('',(-0.705516335778294,0.643766472946353,0.2963299314281));
#41264=DIRECTION('center_axis',(-0.561006631580414,-0.244027156056941,-0.791026109827963));
#41265=DIRECTION('ref_axis',(-0.815685591418248,0.,0.578495476173032));
#41266=DIRECTION('',(0.,0.955563307154868,-0.294785966455752));
#41267=DIRECTION('',(0.705516335778309,-0.640807009641824,-0.302676520965623));
#41268=DIRECTION('',(-0.705516335778296,-0.358916460582518,0.611085652157604));
#41269=DIRECTION('center_axis',(-0.707106781186546,-0.607940616597039,-0.361120764691834));
#41270=DIRECTION('ref_axis',(-0.454822071931222,0.,0.890582327965354));
#41271=DIRECTION('',(0.,0.510701883081733,-0.859757865108992));
#41272=DIRECTION('',(0.,-0.510701883081733,0.859757865108992));
#41273=DIRECTION('center_axis',(-0.561006631580431,0.762818788136165,-0.321526135468411));
#41274=DIRECTION('ref_axis',(-0.497247150959842,0.,0.867608938901807));
#41275=DIRECTION('',(0.705516335778287,0.237411714330117,-0.667744245837293));
#41276=DIRECTION('',(-0.705516335778295,-0.643766472946363,-0.296329931428075));
#41277=DIRECTION('',(0.,0.388405102597364,0.921488728241605));
#41278=DIRECTION('center_axis',(-0.707106781186556,0.667411250860817,0.233585577946044));
#41279=DIRECTION('ref_axis',(0.313668483594034,0.,0.949532559947166));
#41280=DIRECTION('',(0.,0.330339892306057,-0.943862042647771));
#41281=DIRECTION('',(0.,-0.330339892306057,0.943862042647771));
#41282=DIRECTION('center_axis',(0.,0.921488728241605,-0.388405102597364));
#41283=DIRECTION('ref_axis',(0.,0.388405102597364,0.921488728241605));
#41284=DIRECTION('',(-1.,0.,0.));
#41285=DIRECTION('',(1.,0.,0.));
#41286=DIRECTION('center_axis',(-0.707106781186564,0.298836238730113,-0.640856382055774));
#41287=DIRECTION('ref_axis',(-0.671542934237801,0.,0.740965645273304));
#41288=DIRECTION('',(0.,-0.90630778703665,-0.422618261740699));
#41289=DIRECTION('',(0.,0.90630778703665,0.422618261740699));
#41290=DIRECTION('center_axis',(0.,-0.294785966455752,-0.955563307154868));
#41291=DIRECTION('ref_axis',(-1.,0.,0.));
#41292=DIRECTION('',(-1.,0.,0.));
#41293=DIRECTION('',(1.,0.,0.));
#41294=DIRECTION('center_axis',(0.707106781186557,0.667411250860816,0.233585577946044));
#41295=DIRECTION('ref_axis',(0.313668483594033,0.,-0.949532559947167));
#41296=DIRECTION('',(0.,0.330339892306057,-0.943862042647771));
#41297=DIRECTION('',(0.,-0.330339892306057,0.943862042647771));
#41298=DIRECTION('center_axis',(0.707106781186551,0.298836238730118,-0.640856382055785));
#41299=DIRECTION('ref_axis',(-0.671542934237814,0.,-0.740965645273293));
#41300=DIRECTION('',(0.,-0.90630778703665,-0.422618261740699));
#41301=DIRECTION('',(0.,0.90630778703665,0.422618261740699));
#41302=DIRECTION('center_axis',(0.707106781186547,-0.607940616597037,-0.361120764691833));
#41303=DIRECTION('ref_axis',(-0.454822071931221,0.,-0.890582327965355));
#41304=DIRECTION('',(0.,0.510701883081733,-0.859757865108992));
#41305=DIRECTION('',(0.,-0.510701883081733,0.859757865108992));
#41306=DIRECTION('center_axis',(1.,0.,0.));
#41307=DIRECTION('ref_axis',(0.,-0.422618261740699,0.90630778703665));
#41308=DIRECTION('center_axis',(0.,-0.859757865108992,-0.510701883081733));
#41309=DIRECTION('ref_axis',(0.,0.510701883081733,-0.859757865108992));
#41310=DIRECTION('center_axis',(0.,0.422618261740699,-0.90630778703665));
#41311=DIRECTION('ref_axis',(0.,0.90630778703665,0.422618261740699));
#41312=DIRECTION('center_axis',(0.561006631580407,0.787938881495568,-0.253818593389688));
#41313=DIRECTION('ref_axis',(-0.412208150462316,0.,-0.9110896995864));
#41314=DIRECTION('',(0.705516335778306,-0.29470603679192,0.644511483084942));
#41315=DIRECTION('',(0.,-0.306614069375781,-0.951833920629446));
#41316=DIRECTION('',(-0.7055163357783,0.615489891886393,0.351310251680245));
#41317=DIRECTION('center_axis',(0.,0.951833920629447,-0.306614069375781));
#41318=DIRECTION('ref_axis',(0.,0.306614069375781,0.951833920629446));
#41319=DIRECTION('',(0.557191914001238,0.254607340492412,0.790387419648756));
#41320=DIRECTION('',(1.,0.,0.));
#41321=DIRECTION('',(-1.,0.,0.));
#41322=DIRECTION('',(-0.557191914001261,0.254607340492407,0.790387419648741));
#41323=DIRECTION('center_axis',(0.707106781186551,0.644513225013302,0.290865437587465));
#41324=DIRECTION('ref_axis',(0.380418570543385,0.,-0.924814419862562));
#41325=DIRECTION('',(0.,0.41134584666178,-0.911479343942639));
#41326=DIRECTION('',(0.,-0.41134584666178,0.911479343942639));
#41327=DIRECTION('center_axis',(0.561006631580406,-0.174156090919475,-0.809284384699504));
#41328=DIRECTION('ref_axis',(-0.821843752318937,0.,-0.569712951208177));
#41329=DIRECTION('',(0.705516335778312,0.611988548508171,0.357374756306047));
#41330=DIRECTION('',(0.,-0.977619390136734,0.210381387077564));
#41331=DIRECTION('',(-0.705516335778298,0.410810298986407,-0.577478656052899));
#41332=DIRECTION('center_axis',(0.,-0.210381387077564,-0.977619390136734));
#41333=DIRECTION('ref_axis',(-1.,0.,0.));
#41334=DIRECTION('',(0.557191914001257,0.811799254493649,-0.174697284967946));
#41335=DIRECTION('',(1.,0.,0.));
#41336=DIRECTION('',(-1.,0.,0.));
#41337=DIRECTION('',(-0.557191914001251,0.811799254493653,-0.174697284967946));
#41338=DIRECTION('center_axis',(0.707106781186549,0.353553390593273,-0.612372435695794));
#41339=DIRECTION('ref_axis',(-0.654653670707976,0.,-0.755928946018455));
#41340=DIRECTION('',(0.,-0.866025403784439,-0.5));
#41341=DIRECTION('',(0.,0.866025403784439,0.5));
#41342=DIRECTION('center_axis',(0.707106781186542,-0.574153470540281,-0.412732107142828));
#41343=DIRECTION('ref_axis',(-0.504101701135475,0.,-0.863644298836228));
#41344=DIRECTION('',(0.,0.583691343548208,-0.81197562492164));
#41345=DIRECTION('',(0.,-0.583691343548208,0.81197562492164));
#41346=DIRECTION('center_axis',(-0.707106781186549,0.644513225013304,0.290865437587466));
#41347=DIRECTION('ref_axis',(0.380418570543387,0.,0.924814419862562));
#41348=DIRECTION('',(-0.595596683047435,-0.764592607463601,0.246298062832224));
#41349=DIRECTION('',(0.,-0.41134584666178,0.911479343942639));
#41350=DIRECTION('',(0.,0.41134584666178,-0.911479343942639));
#41351=DIRECTION('center_axis',(0.,0.5,-0.866025403784439));
#41352=DIRECTION('ref_axis',(0.,0.866025403784439,0.5));
#41353=DIRECTION('',(0.,-0.866025403784439,-0.5));
#41354=DIRECTION('center_axis',(-0.707106781186533,0.353553390593281,-0.612372435695807));
#41355=DIRECTION('ref_axis',(-0.654653670707993,0.,0.755928946018441));
#41356=DIRECTION('',(0.595596683047433,-0.168995924416179,-0.785305653025379));
#41357=DIRECTION('',(0.,0.866025403784439,0.5));
#41358=DIRECTION('center_axis',(-0.707106781186541,-0.574153470540282,-0.412732107142829));
#41359=DIRECTION('ref_axis',(-0.504101701135477,0.,0.863644298836227));
#41360=DIRECTION('',(0.,-0.583691343548208,0.81197562492164));
#41361=DIRECTION('',(0.,0.583691343548208,-0.81197562492164));
#41362=DIRECTION('center_axis',(0.,-0.81197562492164,-0.583691343548208));
#41363=DIRECTION('ref_axis',(0.,0.583691343548208,-0.81197562492164));
#41364=DIRECTION('center_axis',(0.,0.911479343942639,0.41134584666178));
#41365=DIRECTION('ref_axis',(0.,-0.41134584666178,0.911479343942639));
#41366=DIRECTION('center_axis',(0.561006631580388,-0.1029595927718,-0.821383516744214));
#41367=DIRECTION('ref_axis',(-0.825772049781974,0.,-0.564004008672702));
#41368=DIRECTION('',(0.705516335778307,0.578512484991612,0.409353153962177));
#41369=DIRECTION('',(0.,-0.992235199256928,0.124375678311978));
#41370=DIRECTION('',(-0.705516335778309,0.459577622960955,-0.539476698684482));
#41371=DIRECTION('center_axis',(0.561006631580405,0.807062284196269,-0.184179338555412));
#41372=DIRECTION('ref_axis',(-0.311921838389586,0.,-0.95010776585378));
#41373=DIRECTION('',(0.705516335778315,-0.349757468365408,0.616373598779637));
#41374=DIRECTION('',(0.,-0.22248951794762,-0.974935082148261));
#41375=DIRECTION('',(-0.7055163357783,0.582529061106229,0.403616888790171));
#41376=DIRECTION('center_axis',(-0.561006631580387,-0.102959592771799,-0.821383516744215));
#41377=DIRECTION('ref_axis',(-0.825772049781975,0.,0.5640040086727));
#41378=DIRECTION('',(0.,0.992235199256928,-0.124375678311978));
#41379=DIRECTION('',(0.705516335778308,-0.578512484991611,-0.409353153962176));
#41380=DIRECTION('',(-0.70551633577831,-0.459577622960954,0.539476698684481));
#41381=DIRECTION('center_axis',(-0.707106781186546,-0.535996669889361,-0.461202309044001));
#41382=DIRECTION('ref_axis',(-0.546305769586289,0.,0.83758582015023));
#41383=DIRECTION('',(0.,0.652238560447812,-0.758013759944347));
#41384=DIRECTION('',(0.,-0.652238560447812,0.758013759944347));
#41385=DIRECTION('center_axis',(-0.561006631580403,0.80706228419627,-0.184179338555412));
#41386=DIRECTION('ref_axis',(-0.311921838389587,0.,0.95010776585378));
#41387=DIRECTION('',(0.705516335778317,0.349757468365407,-0.616373598779635));
#41388=DIRECTION('',(-0.705516335778301,-0.582529061106227,-0.40361688879017));
#41389=DIRECTION('',(0.,0.22248951794762,0.974935082148261));
#41390=DIRECTION('center_axis',(-0.707106781186545,0.616710064355711,0.345931635619494));
#41391=DIRECTION('ref_axis',(0.439451044888515,0.,0.898266541259549));
#41392=DIRECTION('',(0.,0.489221210746995,-0.872159737063827));
#41393=DIRECTION('',(0.,-0.489221210746995,0.872159737063827));
#41394=DIRECTION('center_axis',(0.,0.974935082148261,-0.22248951794762));
#41395=DIRECTION('ref_axis',(0.,0.22248951794762,0.974935082148261));
#41396=DIRECTION('',(-1.,0.,0.));
#41397=DIRECTION('',(1.,0.,0.));
#41398=DIRECTION('center_axis',(-0.707106781186546,0.40557978767264,-0.579227965339571));
#41399=DIRECTION('ref_axis',(-0.633687274224644,0.,0.773589321594954));
#41400=DIRECTION('',(0.,-0.819152044288992,-0.573576436351046));
#41401=DIRECTION('',(0.,0.819152044288992,0.573576436351046));
#41402=DIRECTION('center_axis',(0.,-0.124375678311978,-0.992235199256928));
#41403=DIRECTION('ref_axis',(-1.,0.,0.));
#41404=DIRECTION('',(-1.,0.,0.));
#41405=DIRECTION('',(1.,0.,0.));
#41406=DIRECTION('center_axis',(0.707106781186546,0.61671006435571,0.345931635619494));
#41407=DIRECTION('ref_axis',(0.439451044888513,0.,-0.898266541259549));
#41408=DIRECTION('',(0.,0.489221210746995,-0.872159737063827));
#41409=DIRECTION('',(0.,-0.489221210746995,0.872159737063827));
#41410=DIRECTION('center_axis',(0.707106781186547,0.405579787672639,-0.57922796533957));
#41411=DIRECTION('ref_axis',(-0.633687274224642,0.,-0.773589321594955));
#41412=DIRECTION('',(0.,-0.819152044288992,-0.573576436351046));
#41413=DIRECTION('',(0.,0.819152044288992,0.573576436351046));
#41414=DIRECTION('center_axis',(0.707106781186547,-0.53599666988936,-0.461202309044));
#41415=DIRECTION('ref_axis',(-0.546305769586287,0.,-0.837585820150231));
#41416=DIRECTION('',(0.,0.652238560447812,-0.758013759944347));
#41417=DIRECTION('',(0.,-0.652238560447812,0.758013759944347));
#41418=DIRECTION('center_axis',(1.,0.,0.));
#41419=DIRECTION('ref_axis',(0.,-0.573576436351046,0.819152044288992));
#41420=DIRECTION('center_axis',(0.,-0.758013759944347,-0.652238560447812));
#41421=DIRECTION('ref_axis',(0.,0.652238560447812,-0.758013759944347));
#41422=DIRECTION('center_axis',(0.,0.573576436351046,-0.819152044288992));
#41423=DIRECTION('ref_axis',(0.,0.819152044288992,0.573576436351046));
#41424=DIRECTION('center_axis',(0.56100663158041,-0.0309795099544078,-0.827231424261547));
#41425=DIRECTION('ref_axis',(-0.827628669643383,0.,-0.561276032968025));
#41426=DIRECTION('',(0.705516335778304,0.540633592148827,0.458216126942529));
#41427=DIRECTION('',(0.,-0.999299499382783,0.037423395534326));
#41428=DIRECTION('',(-0.705516335778297,0.50484728372422,-0.497368997894162));
#41429=DIRECTION('center_axis',(0.561006631580422,0.820043455596693,-0.113138367744206));
#41430=DIRECTION('ref_axis',(-0.197690230426216,0.,-0.980264542250728));
#41431=DIRECTION('',(0.70551633577829,-0.402147034415294,0.583544739211107));
#41432=DIRECTION('',(0.,-0.136671686945037,-0.990616399010029));
#41433=DIRECTION('',(-0.705516335778305,0.545134832430407,0.452851757665825));
#41434=DIRECTION('center_axis',(-0.561006631580388,-0.0309795099544084,
-0.827231424261562));
#41435=DIRECTION('ref_axis',(-0.827628669643398,0.,0.561276032968003));
#41436=DIRECTION('',(0.,0.999299499382783,-0.037423395534326));
#41437=DIRECTION('',(0.705516335778314,-0.540633592148832,-0.458216126942508));
#41438=DIRECTION('',(-0.705516335778307,-0.504847283724225,0.497368997894142));
#41439=DIRECTION('center_axis',(-0.70710678118654,-0.493760610936952,-0.506162482891787));
#41440=DIRECTION('ref_axis',(-0.582064997116551,0.,0.813142262541868));
#41441=DIRECTION('',(0.,0.715821848069997,-0.698282952552655));
#41442=DIRECTION('',(0.,-0.715821848069997,0.698282952552655));
#41443=DIRECTION('center_axis',(-0.561006631580398,0.820043455596709,-0.113138367744208));
#41444=DIRECTION('ref_axis',(-0.197690230426228,0.,0.980264542250726));
#41445=DIRECTION('',(0.70551633577832,0.402147034415284,-0.583544739211079));
#41446=DIRECTION('',(-0.705516335778308,-0.545134832430382,-0.45285175766585));
#41447=DIRECTION('',(0.,0.136671686945037,0.990616399010029));
#41448=DIRECTION('center_axis',(-0.70710678118654,0.584213367728653,0.398365085025227));
#41449=DIRECTION('ref_axis',(0.490839120629142,0.,0.871250226777595));
#41450=DIRECTION('',(0.,0.563373306018581,-0.826202467961513));
#41451=DIRECTION('',(0.,-0.563373306018581,0.826202467961513));
#41452=DIRECTION('center_axis',(0.,0.990616399010029,-0.136671686945037));
#41453=DIRECTION('ref_axis',(0.,0.136671686945037,0.990616399010029));
#41454=DIRECTION('',(-1.,0.,0.));
#41455=DIRECTION('',(1.,0.,0.));
#41456=DIRECTION('center_axis',(-0.70710678118653,0.454519477672055,-0.541675220419715));
#41457=DIRECTION('ref_axis',(-0.608120402411362,0.,0.793844806099431));
#41458=DIRECTION('',(0.,-0.766044443118978,-0.642787609686539));
#41459=DIRECTION('',(0.,0.766044443118978,0.642787609686539));
#41460=DIRECTION('center_axis',(0.,-0.037423395534326,-0.999299499382783));
#41461=DIRECTION('ref_axis',(-1.,0.,0.));
#41462=DIRECTION('',(-1.,0.,0.));
#41463=DIRECTION('',(1.,0.,0.));
#41464=DIRECTION('center_axis',(0.707106781186542,0.584213367728652,0.398365085025226));
#41465=DIRECTION('ref_axis',(0.490839120629141,0.,-0.871250226777596));
#41466=DIRECTION('',(0.,0.563373306018581,-0.826202467961513));
#41467=DIRECTION('',(0.,-0.563373306018581,0.826202467961513));
#41468=DIRECTION('center_axis',(0.707106781186559,0.454519477672036,-0.541675220419693));
#41469=DIRECTION('ref_axis',(-0.60812040241133,0.,-0.793844806099455));
#41470=DIRECTION('',(0.,-0.766044443118978,-0.642787609686539));
#41471=DIRECTION('',(0.,0.766044443118978,0.642787609686539));
#41472=DIRECTION('center_axis',(0.707106781186551,-0.493760610936944,-0.50616248289178));
#41473=DIRECTION('ref_axis',(-0.58206499711654,0.,-0.813142262541876));
#41474=DIRECTION('',(0.,0.715821848069997,-0.698282952552655));
#41475=DIRECTION('',(0.,-0.715821848069997,0.698282952552655));
#41476=DIRECTION('center_axis',(1.,0.,0.));
#41477=DIRECTION('ref_axis',(0.,-0.642787609686539,0.766044443118978));
#41478=DIRECTION('center_axis',(0.,-0.698282952552655,-0.715821848069998));
#41479=DIRECTION('ref_axis',(0.,0.715821848069997,-0.698282952552655));
#41480=DIRECTION('center_axis',(0.,0.642787609686539,-0.766044443118978));
#41481=DIRECTION('ref_axis',(0.,0.766044443118978,0.642787609686539));
#41482=DIRECTION('center_axis',(0.707106781186551,-0.447766735594493,-0.547270454615491));
#41483=DIRECTION('ref_axis',(-0.612056372482119,0.,-0.790814135498367));
#41484=DIRECTION('',(0.595596683047422,-0.0400145312984589,0.802286375571637));
#41485=DIRECTION('',(0.,-0.773957299203321,0.633237790257263));
#41486=DIRECTION('',(0.,0.773957299203321,-0.633237790257263));
#41487=DIRECTION('',(0.557191914001248,0.829352850155039,0.0413644885298826));
#41488=DIRECTION('center_axis',(1.,0.,0.));
#41489=DIRECTION('ref_axis',(0.,-0.707106781186547,0.707106781186548));
#41490=DIRECTION('',(0.,-0.707106781186548,-0.707106781186547));
#41491=DIRECTION('',(0.,0.633237790257263,-0.773957299203321));
#41492=DIRECTION('center_axis',(0.707106781186548,0.5,-0.5));
#41493=DIRECTION('ref_axis',(-0.577350269189625,0.,-0.816496580927726));
#41494=DIRECTION('',(0.55719191400122,-0.829352850155059,-0.0413644885298627));
#41495=DIRECTION('',(0.,0.707106781186548,0.707106781186547));
#41496=DIRECTION('',(0.705516335778303,-0.451476018710246,0.546274751823203));
#41497=DIRECTION('center_axis',(0.,0.0498137018801831,-0.998758526924798));
#41498=DIRECTION('ref_axis',(-1.,0.,0.));
#41499=DIRECTION('',(-1.,0.,0.));
#41500=DIRECTION('',(0.,0.998758526924798,0.0498137018801831));
#41501=DIRECTION('',(1.,0.,0.));
#41502=DIRECTION('center_axis',(0.561006631580394,0.826783601144283,-0.041236345639636));
#41503=DIRECTION('ref_axis',(-0.0733064378127065,0.,-0.997309463594531));
#41504=DIRECTION('',(0.,-0.049813701880158,-0.998758526924799));
#41505=DIRECTION('',(-0.705516335778304,0.503591798518316,0.498640151226356));
#41506=DIRECTION('center_axis',(-0.561006631580403,0.0412363456396555,-0.826783601144276));
#41507=DIRECTION('ref_axis',(-0.82748744528631,0.,0.561484218739526));
#41508=DIRECTION('',(0.705516335778297,-0.498640151226348,-0.503591798518334));
#41509=DIRECTION('',(-0.705516335778305,-0.546274751823202,0.451476018710245));
#41510=DIRECTION('center_axis',(-0.70710678118655,-0.447766735594494,-0.547270454615492));
#41511=DIRECTION('ref_axis',(-0.61205637248212,0.,0.790814135498366));
#41512=DIRECTION('',(0.,0.773957299203321,-0.633237790257263));
#41513=DIRECTION('',(0.,-0.773957299203321,0.633237790257263));
#41514=DIRECTION('center_axis',(-0.561006631580412,0.826783601144271,-0.0412363456396355));
#41515=DIRECTION('ref_axis',(-0.0733064378127032,0.,0.997309463594532));
#41516=DIRECTION('',(0.705516335778307,0.451476018710271,-0.546274751823178));
#41517=DIRECTION('',(-0.705516335778288,-0.503591798518327,-0.498640151226367));
#41518=DIRECTION('',(0.,0.049813701880158,0.998758526924799));
#41519=DIRECTION('center_axis',(-0.707106781186558,0.547270454615486,0.447766735594489));
#41520=DIRECTION('ref_axis',(0.534994468449976,0.,0.84485556086702));
#41521=DIRECTION('',(0.,0.633237790257263,-0.773957299203321));
#41522=DIRECTION('',(0.,-0.633237790257263,0.773957299203321));
#41523=DIRECTION('center_axis',(0.,0.998758526924799,-0.049813701880158));
#41524=DIRECTION('ref_axis',(0.,0.049813701880158,0.998758526924799));
#41525=DIRECTION('',(-1.,0.,0.));
#41526=DIRECTION('',(1.,0.,0.));
#41527=DIRECTION('center_axis',(-0.707106781186547,0.500000000000001,-0.500000000000001));
#41528=DIRECTION('ref_axis',(-0.577350269189627,0.,0.816496580927725));
#41529=DIRECTION('',(0.,-0.707106781186548,-0.707106781186547));
#41530=DIRECTION('',(0.,0.707106781186548,0.707106781186547));
#41531=DIRECTION('center_axis',(0.707106781186551,0.547270454615491,0.447766735594493));
#41532=DIRECTION('ref_axis',(0.534994468449983,0.,-0.844855560867016));
#41533=DIRECTION('',(0.,-0.633237790257263,0.773957299203321));
#41534=DIRECTION('center_axis',(0.,-0.633237790257263,-0.773957299203321));
#41535=DIRECTION('ref_axis',(0.,0.773957299203321,-0.633237790257263));
#41536=DIRECTION('center_axis',(0.,0.707106781186547,-0.707106781186548));
#41537=DIRECTION('ref_axis',(0.,0.707106781186548,0.707106781186547));
#41538=DIRECTION('center_axis',(0.561006631580392,0.113138367744223,-0.820043455596711));
#41539=DIRECTION('ref_axis',(-0.825342782028782,0.,-0.564631997103415));
#41540=DIRECTION('',(0.705516335778306,0.452851757665851,0.545134832430383));
#41541=DIRECTION('',(0.,-0.990616399010027,-0.136671686945054));
#41542=DIRECTION('',(-0.705516335778304,0.583544739211119,-0.402147034415252));
#41543=DIRECTION('center_axis',(0.5610066315804,0.827231424261552,0.0309795099544278));
#41544=DIRECTION('ref_axis',(0.0551372865287725,0.,-0.998478782766186));
#41545=DIRECTION('',(0.705516335778306,-0.497368997894168,0.504847283724201));
#41546=DIRECTION('',(0.,0.0374233955343499,-0.999299499382783));
#41547=DIRECTION('',(-0.705516335778302,0.458216126942503,0.540633592148851));
#41548=DIRECTION('center_axis',(-0.56100663158039,0.113138367744223,-0.820043455596712));
#41549=DIRECTION('ref_axis',(-0.825342782028783,0.,0.564631997103413));
#41550=DIRECTION('',(0.,0.990616399010027,0.136671686945054));
#41551=DIRECTION('',(0.705516335778308,-0.45285175766585,-0.545134832430382));
#41552=DIRECTION('',(-0.705516335778306,-0.583544739211118,0.402147034415251));
#41553=DIRECTION('center_axis',(-0.707106781186547,-0.398365085025223,-0.584213367728647));
#41554=DIRECTION('ref_axis',(-0.636934375125931,0.,0.770918025332746));
#41555=DIRECTION('',(0.,0.826202467961513,-0.563373306018581));
#41556=DIRECTION('',(0.,-0.826202467961513,0.563373306018581));
#41557=DIRECTION('center_axis',(-0.561006631580419,0.82723142426154,0.0309795099544274));
#41558=DIRECTION('ref_axis',(0.0551372865287699,0.,0.998478782766186));
#41559=DIRECTION('',(0.705516335778298,0.497368997894186,-0.504847283724194));
#41560=DIRECTION('',(-0.705516335778296,-0.458216126942521,-0.540633592148843));
#41561=DIRECTION('',(0.,-0.0374233955343499,0.999299499382783));
#41562=DIRECTION('center_axis',(-0.707106781186558,0.506162482891774,0.493760610936939));
#41563=DIRECTION('ref_axis',(0.572517134274658,0.,0.819892755768663));
#41564=DIRECTION('',(0.,0.698282952552655,-0.715821848069998));
#41565=DIRECTION('',(0.,-0.698282952552655,0.715821848069998));
#41566=DIRECTION('center_axis',(0.,0.999299499382783,0.0374233955343499));
#41567=DIRECTION('ref_axis',(0.,-0.0374233955343499,0.999299499382783));
#41568=DIRECTION('',(-1.,0.,0.));
#41569=DIRECTION('',(1.,0.,0.));
#41570=DIRECTION('center_axis',(-0.707106781186558,0.541675220419694,-0.454519477672037));
#41571=DIRECTION('ref_axis',(-0.540716203060926,0.,0.841205080671399));
#41572=DIRECTION('',(0.,-0.642787609686539,-0.766044443118978));
#41573=DIRECTION('',(0.,0.642787609686539,0.766044443118978));
#41574=DIRECTION('center_axis',(0.,0.136671686945054,-0.990616399010027));
#41575=DIRECTION('ref_axis',(-1.,0.,0.));
#41576=DIRECTION('',(-1.,0.,0.));
#41577=DIRECTION('',(1.,0.,0.));
#41578=DIRECTION('center_axis',(0.70710678118656,0.506162482891773,0.493760610936938));
#41579=DIRECTION('ref_axis',(0.572517134274656,0.,-0.819892755768665));
#41580=DIRECTION('',(0.,0.698282952552655,-0.715821848069998));
#41581=DIRECTION('',(0.,-0.698282952552655,0.715821848069998));
#41582=DIRECTION('center_axis',(0.70710678118655,0.5416752204197,-0.454519477672042));
#41583=DIRECTION('ref_axis',(-0.540716203060935,0.,-0.841205080671394));
#41584=DIRECTION('',(0.,-0.642787609686539,-0.766044443118978));
#41585=DIRECTION('',(0.,0.642787609686539,0.766044443118978));
#41586=DIRECTION('center_axis',(0.707106781186549,-0.398365085025222,-0.584213367728646));
#41587=DIRECTION('ref_axis',(-0.636934375125929,0.,-0.770918025332747));
#41588=DIRECTION('',(0.,0.826202467961513,-0.563373306018581));
#41589=DIRECTION('',(0.,-0.826202467961513,0.563373306018581));
#41590=DIRECTION('center_axis',(1.,0.,0.));
#41591=DIRECTION('ref_axis',(0.,-0.766044443118978,0.642787609686539));
#41592=DIRECTION('center_axis',(0.,-0.563373306018581,-0.826202467961513));
#41593=DIRECTION('ref_axis',(0.,0.826202467961513,-0.563373306018581));
#41594=DIRECTION('center_axis',(0.,0.766044443118978,-0.642787609686539));
#41595=DIRECTION('ref_axis',(0.,0.642787609686539,0.766044443118978));
#41596=DIRECTION('center_axis',(0.56100663158042,0.82138351674419,0.102959592771817));
#41597=DIRECTION('ref_axis',(0.180511696561749,0.,-0.98357283787445));
#41598=DIRECTION('',(0.705516335778302,-0.539476698684527,0.459577622960913));
#41599=DIRECTION('',(0.,0.124375678312001,-0.992235199256925));
#41600=DIRECTION('',(-0.705516335778294,0.409353153962195,0.578512484991614));
#41601=DIRECTION('center_axis',(0.,0.992235199256925,0.124375678312001));
#41602=DIRECTION('ref_axis',(0.,-0.124375678312001,0.992235199256925));
#41603=DIRECTION('',(0.55719191400124,-0.103279542068723,0.823935984868794));
#41604=DIRECTION('',(1.,0.,0.));
#41605=DIRECTION('',(-1.,0.,0.));
#41606=DIRECTION('',(-0.557191914001254,-0.103279542068721,0.823935984868785));
#41607=DIRECTION('center_axis',(0.707106781186552,0.461202309043997,0.535996669889356));
#41608=DIRECTION('ref_axis',(0.604079438549187,0.,-0.796924106751765));
#41609=DIRECTION('',(0.,0.758013759944346,-0.652238560447812));
#41610=DIRECTION('',(0.,-0.758013759944346,0.652238560447812));
#41611=DIRECTION('center_axis',(0.56100663158041,0.18417933855543,-0.807062284196261));
#41612=DIRECTION('ref_axis',(-0.821109284001916,0.,-0.570771008133613));
#41613=DIRECTION('',(0.705516335778302,0.403616888790147,0.582529061106243));
#41614=DIRECTION('',(0.,-0.974935082148255,-0.222489517947642));
#41615=DIRECTION('',(-0.705516335778307,0.616373598779655,-0.349757468365392));
#41616=DIRECTION('center_axis',(0.,0.222489517947642,-0.974935082148256));
#41617=DIRECTION('ref_axis',(-1.,0.,0.));
#41618=DIRECTION('',(0.557191914001234,0.809570248762125,0.184751680075913));
#41619=DIRECTION('',(1.,0.,0.));
#41620=DIRECTION('',(-1.,0.,0.));
#41621=DIRECTION('',(-0.557191914001256,0.809570248762111,0.184751680075909));
#41622=DIRECTION('center_axis',(0.707106781186547,0.579227965339569,-0.405579787672639));
#41623=DIRECTION('ref_axis',(-0.497542812164523,0.,-0.867439421552547));
#41624=DIRECTION('',(0.,-0.573576436351046,-0.819152044288992));
#41625=DIRECTION('',(0.,0.573576436351046,0.819152044288992));
#41626=DIRECTION('center_axis',(0.707106781186546,-0.345931635619494,-0.61671006435571));
#41627=DIRECTION('ref_axis',(-0.657291420225581,0.,-0.753636509796227));
#41628=DIRECTION('',(0.,0.872159737063827,-0.489221210746995));
#41629=DIRECTION('',(0.,-0.872159737063827,0.489221210746995));
#41630=DIRECTION('center_axis',(-0.707106781186541,0.461202309044004,0.535996669889364));
#41631=DIRECTION('ref_axis',(0.604079438549199,0.,0.796924106751756));
#41632=DIRECTION('',(-0.595596683047437,-0.797046293239175,-0.0999089464291446));
#41633=DIRECTION('',(0.,-0.758013759944346,0.652238560447812));
#41634=DIRECTION('',(0.,0.758013759944346,-0.652238560447812));
#41635=DIRECTION('center_axis',(0.,0.819152044288992,-0.573576436351046));
#41636=DIRECTION('ref_axis',(0.,0.573576436351046,0.819152044288992));
#41637=DIRECTION('',(0.,-0.573576436351046,-0.819152044288992));
#41638=DIRECTION('center_axis',(-0.707106781186546,0.579227965339571,-0.40557978767264));
#41639=DIRECTION('ref_axis',(-0.497542812164525,0.,0.867439421552546));
#41640=DIRECTION('',(0.595596683047429,0.178722187740901,-0.783149392358831));
#41641=DIRECTION('',(0.,0.573576436351046,0.819152044288992));
#41642=DIRECTION('center_axis',(-0.707106781186545,-0.345931635619495,-0.616710064355711));
#41643=DIRECTION('ref_axis',(-0.657291420225582,0.,0.753636509796226));
#41644=DIRECTION('',(0.,-0.872159737063827,0.489221210746995));
#41645=DIRECTION('',(0.,0.872159737063827,-0.489221210746995));
#41646=DIRECTION('center_axis',(0.,-0.489221210746995,-0.872159737063827));
#41647=DIRECTION('ref_axis',(0.,0.872159737063827,-0.489221210746995));
#41648=DIRECTION('center_axis',(0.,0.652238560447812,0.758013759944346));
#41649=DIRECTION('ref_axis',(0.,-0.758013759944346,0.652238560447812));
#41650=DIRECTION('center_axis',(0.561006631580402,0.253818593389698,-0.787938881495568));
#41651=DIRECTION('ref_axis',(-0.814616058663784,0.,-0.580000583592019));
#41652=DIRECTION('',(0.7055163357783,0.351310251680245,0.615489891886393));
#41653=DIRECTION('',(0.,-0.951833920629443,-0.306614069375792));
#41654=DIRECTION('',(-0.705516335778309,0.644511483084945,-0.294706036791908));
#41655=DIRECTION('center_axis',(0.561006631580397,0.809284384699514,0.174156090919455));
#41656=DIRECTION('ref_axis',(0.2964777621296,0.,-0.955039756535101));
#41657=DIRECTION('',(0.705516335778309,-0.577478656052882,0.410810298986413));
#41658=DIRECTION('',(0.,0.210381387077539,-0.97761939013674));
#41659=DIRECTION('',(-0.705516335778306,0.357374756306044,0.611988548508179));
#41660=DIRECTION('center_axis',(-0.561006631580411,0.253818593389687,-0.787938881495565));
#41661=DIRECTION('ref_axis',(-0.814616058663778,0.,0.580000583592027));
#41662=DIRECTION('',(0.,0.951833920629443,0.306614069375792));
#41663=DIRECTION('',(0.705516335778308,-0.351310251680223,-0.615489891886397));
#41664=DIRECTION('',(-0.705516335778296,-0.644511483084956,0.294706036791914));
#41665=DIRECTION('center_axis',(-0.707106781186549,-0.290865437587467,-0.644513225013303));
#41666=DIRECTION('ref_axis',(-0.673638686438956,0.,0.739060836557315));
#41667=DIRECTION('',(0.,0.911479343942638,-0.411345846661781));
#41668=DIRECTION('',(0.,-0.911479343942638,0.411345846661781));
#41669=DIRECTION('center_axis',(-0.561006631580409,0.809284384699507,0.174156090919453));
#41670=DIRECTION('ref_axis',(0.296477762129592,0.,0.955039756535103));
#41671=DIRECTION('',(0.705516335778289,0.577478656052889,-0.410810298986437));
#41672=DIRECTION('',(-0.705516335778318,-0.357374756306074,-0.611988548508149));
#41673=DIRECTION('',(0.,-0.210381387077539,0.97761939013674));
#41674=DIRECTION('center_axis',(-0.707106781186536,0.412732107142832,0.574153470540286));
#41675=DIRECTION('ref_axis',(0.630347388214446,0.,0.776313190774978));
#41676=DIRECTION('',(0.,0.811975624921639,-0.583691343548209));
#41677=DIRECTION('',(0.,-0.811975624921639,0.583691343548209));
#41678=DIRECTION('center_axis',(0.,0.97761939013674,0.210381387077539));
#41679=DIRECTION('ref_axis',(0.,-0.210381387077539,0.97761939013674));
#41680=DIRECTION('',(-1.,0.,0.));
#41681=DIRECTION('',(1.,0.,0.));
#41682=DIRECTION('center_axis',(-0.707106781186558,0.612372435695785,-0.353553390593269));
#41683=DIRECTION('ref_axis',(-0.447213595499948,0.,0.894427190999921));
#41684=DIRECTION('',(0.,-0.5,-0.866025403784438));
#41685=DIRECTION('',(0.,0.5,0.866025403784438));
#41686=DIRECTION('center_axis',(0.,0.306614069375792,-0.951833920629443));
#41687=DIRECTION('ref_axis',(-1.,0.,0.));
#41688=DIRECTION('',(-1.,0.,0.));
#41689=DIRECTION('',(1.,0.,0.));
#41690=DIRECTION('center_axis',(0.707106781186547,0.412732107142825,0.574153470540276));
#41691=DIRECTION('ref_axis',(0.630347388214433,0.,-0.776313190774988));
#41692=DIRECTION('',(0.,0.811975624921639,-0.583691343548209));
#41693=DIRECTION('',(0.,-0.811975624921639,0.583691343548209));
#41694=DIRECTION('center_axis',(0.707106781186545,0.612372435695796,-0.353553390593275));
#41695=DIRECTION('ref_axis',(-0.44721359549996,0.,-0.894427190999915));
#41696=DIRECTION('',(0.,-0.5,-0.866025403784438));
#41697=DIRECTION('',(0.,0.5,0.866025403784438));
#41698=DIRECTION('center_axis',(0.707106781186551,-0.290865437587466,-0.644513225013302));
#41699=DIRECTION('ref_axis',(-0.673638686438954,0.,-0.739060836557317));
#41700=DIRECTION('',(0.,0.911479343942638,-0.411345846661781));
#41701=DIRECTION('',(0.,-0.911479343942638,0.411345846661781));
#41702=DIRECTION('center_axis',(1.,0.,0.));
#41703=DIRECTION('ref_axis',(0.,-0.866025403784438,0.5));
#41704=DIRECTION('center_axis',(0.,-0.411345846661781,-0.911479343942638));
#41705=DIRECTION('ref_axis',(0.,0.911479343942638,-0.411345846661781));
#41706=DIRECTION('center_axis',(0.,0.866025403784438,-0.5));
#41707=DIRECTION('ref_axis',(0.,0.5,0.866025403784438));
#41708=DIRECTION('center_axis',(0.561006631580419,0.321526135468423,-0.762818788136169));
#41709=DIRECTION('ref_axis',(-0.805595332751383,0.,-0.592466167683176));
#41710=DIRECTION('',(0.705516335778299,0.296329931428078,0.643766472946357));
#41711=DIRECTION('',(0.,-0.921488728241601,-0.388405102597375));
#41712=DIRECTION('',(-0.705516335778303,0.667744245837286,-0.237411714330086));
#41713=DIRECTION('center_axis',(0.561006631580396,0.791026109827976,0.244027156056938));
#41714=DIRECTION('ref_axis',(0.398879012810069,0.,-0.917003562228449));
#41715=DIRECTION('',(0.705516335778303,-0.611085652157587,0.358916460582535));
#41716=DIRECTION('',(0.,0.294785966455742,-0.955563307154871));
#41717=DIRECTION('',(-0.705516335778307,0.302676520965598,0.640807009641837));
#41718=DIRECTION('center_axis',(-0.561006631580408,0.321526135468426,-0.762818788136176));
#41719=DIRECTION('ref_axis',(-0.805595332751391,0.,0.592466167683165));
#41720=DIRECTION('',(0.,0.921488728241601,0.388405102597375));
#41721=DIRECTION('',(0.705516335778306,-0.296329931428079,-0.643766472946349));
#41722=DIRECTION('',(-0.705516335778307,-0.667744245837287,0.237411714330074));
#41723=DIRECTION('center_axis',(-0.70710678118655,-0.233585577946047,-0.667411250860823));
#41724=DIRECTION('ref_axis',(-0.686399640790371,0.,0.727224541062009));
#41725=DIRECTION('',(0.,0.943862042647771,-0.330339892306058));
#41726=DIRECTION('',(0.,-0.943862042647771,0.330339892306058));
#41727=DIRECTION('center_axis',(-0.561006631580394,0.791026109827977,0.244027156056939));
#41728=DIRECTION('ref_axis',(0.39887901281007,0.,0.917003562228448));
#41729=DIRECTION('',(0.705516335778304,0.611085652157585,-0.358916460582534));
#41730=DIRECTION('',(-0.705516335778308,-0.302676520965597,-0.640807009641836));
#41731=DIRECTION('',(0.,-0.294785966455742,0.955563307154871));
#41732=DIRECTION('center_axis',(-0.707106781186546,0.361120764691834,0.607940616597038));
#41733=DIRECTION('ref_axis',(0.651933718094184,0.,0.758275957163283));
#41734=DIRECTION('',(0.,0.859757865108992,-0.510701883081734));
#41735=DIRECTION('',(0.,-0.859757865108992,0.510701883081734));
#41736=DIRECTION('center_axis',(0.,0.955563307154871,0.294785966455742));
#41737=DIRECTION('ref_axis',(0.,-0.294785966455742,0.955563307154871));
#41738=DIRECTION('',(-1.,0.,0.));
#41739=DIRECTION('',(1.,0.,0.));
#41740=DIRECTION('center_axis',(-0.707106781186552,0.640856382055784,-0.298836238730118));
#41741=DIRECTION('ref_axis',(-0.389281620635021,0.,0.921118787038768));
#41742=DIRECTION('',(0.,-0.4226182617407,-0.90630778703665));
#41743=DIRECTION('',(0.,0.4226182617407,0.90630778703665));
#41744=DIRECTION('center_axis',(0.,0.388405102597375,-0.921488728241601));
#41745=DIRECTION('ref_axis',(-1.,0.,0.));
#41746=DIRECTION('',(-1.,0.,0.));
#41747=DIRECTION('',(1.,0.,0.));
#41748=DIRECTION('center_axis',(0.707106781186547,0.361120764691833,0.607940616597037));
#41749=DIRECTION('ref_axis',(0.651933718094183,0.,-0.758275957163284));
#41750=DIRECTION('',(0.,0.859757865108992,-0.510701883081734));
#41751=DIRECTION('',(0.,-0.859757865108992,0.510701883081734));
#41752=DIRECTION('center_axis',(0.707106781186554,0.640856382055783,-0.298836238730118));
#41753=DIRECTION('ref_axis',(-0.389281620635019,0.,-0.921118787038769));
#41754=DIRECTION('',(0.,-0.4226182617407,-0.90630778703665));
#41755=DIRECTION('',(0.,0.4226182617407,0.90630778703665));
#41756=DIRECTION('center_axis',(0.707106781186551,-0.233585577946046,-0.667411250860821));
#41757=DIRECTION('ref_axis',(-0.686399640790369,0.,-0.727224541062011));
#41758=DIRECTION('',(0.,0.943862042647771,-0.330339892306058));
#41759=DIRECTION('',(0.,-0.943862042647771,0.330339892306058));
#41760=DIRECTION('center_axis',(1.,0.,0.));
#41761=DIRECTION('ref_axis',(0.,-0.90630778703665,0.4226182617407));
#41762=DIRECTION('center_axis',(0.,-0.330339892306058,-0.943862042647771));
#41763=DIRECTION('ref_axis',(0.,0.943862042647771,-0.330339892306058));
#41764=DIRECTION('center_axis',(0.,0.90630778703665,-0.4226182617407));
#41765=DIRECTION('ref_axis',(0.,0.4226182617407,0.90630778703665));
#41766=DIRECTION('center_axis',(0.707106781186546,-0.17452799101363,-0.685229874095364));
#41767=DIRECTION('ref_axis',(-0.695910561235545,0.,-0.718128463967853));
#41768=DIRECTION('',(0.595596683047423,-0.375326354772754,0.710207517952256));
#41769=DIRECTION('',(0.,-0.96906138128887,0.246819851905205));
#41770=DIRECTION('',(0.,0.96906138128887,-0.246819851905205));
#41771=DIRECTION('',(0.55719191400124,0.734167558056277,0.387988617963616));
#41772=DIRECTION('center_axis',(1.,0.,0.));
#41773=DIRECTION('ref_axis',(0.,-0.939692620785908,0.342020143325669));
#41774=DIRECTION('',(0.,-0.342020143325669,-0.939692620785908));
#41775=DIRECTION('',(0.,0.900996828806872,-0.433825672914779));
#41776=DIRECTION('center_axis',(0.707106781186551,0.664463024388671,-0.241844762647975));
#41777=DIRECTION('ref_axis',(-0.323615577118182,0.,-0.946188648339466));
#41778=DIRECTION('',(0.557191914001246,-0.734167558056274,-0.387988617963615));
#41779=DIRECTION('',(0.,0.342020143325669,0.939692620785908));
#41780=DIRECTION('',(0.705516335778303,-0.64004191746577,0.304291051193915));
#41781=DIRECTION('center_axis',(0.,0.467240138462762,-0.884130450221741));
#41782=DIRECTION('ref_axis',(-1.,0.,0.));
#41783=DIRECTION('',(-1.,0.,0.));
#41784=DIRECTION('',(0.,0.884130450221741,0.467240138462762));
#41785=DIRECTION('',(1.,0.,0.));
#41786=DIRECTION('center_axis',(0.561006631580418,0.766747648626013,0.312041027189173));
#41787=DIRECTION('ref_axis',(0.486084108127403,0.,-0.873912032086747));
#41788=DIRECTION('',(0.,0.376947046632555,-0.926234810420659));
#41789=DIRECTION('',(-0.705516335778304,0.245674734539573,0.66474854250225));
#41790=DIRECTION('center_axis',(-0.561006631580399,0.386786669513442,-0.731893183196506));
#41791=DIRECTION('ref_axis',(-0.793664727118316,0.,0.608355406755138));
#41792=DIRECTION('',(0.705516335778311,-0.239094361468879,-0.667143602430342));
#41793=DIRECTION('',(-0.705516335778307,-0.68589507168381,0.178310545369064));
#41794=DIRECTION('center_axis',(-0.707106781186545,-0.17452799101363,-0.685229874095365));
#41795=DIRECTION('ref_axis',(-0.695910561235547,0.,0.718128463967852));
#41796=DIRECTION('',(0.,0.96906138128887,-0.246819851905205));
#41797=DIRECTION('',(0.,-0.96906138128887,0.246819851905205));
#41798=DIRECTION('center_axis',(-0.561006631580416,0.766747648626014,0.312041027189174));
#41799=DIRECTION('ref_axis',(0.486084108127405,0.,0.873912032086746));
#41800=DIRECTION('',(0.705516335778304,0.640041917465768,-0.304291051193914));
#41801=DIRECTION('',(-0.705516335778305,-0.245674734539572,-0.664748542502249));
#41802=DIRECTION('',(0.,-0.376947046632555,0.926234810420659));
#41803=DIRECTION('center_axis',(-0.707106781186547,0.306761075170857,0.637100967476914));
#41804=DIRECTION('ref_axis',(0.669373784875801,0.,0.742925794491647));
#41805=DIRECTION('',(0.,0.900996828806872,-0.433825672914779));
#41806=DIRECTION('',(0.,-0.900996828806872,0.433825672914779));
#41807=DIRECTION('center_axis',(0.,0.926234810420659,0.376947046632555));
#41808=DIRECTION('ref_axis',(0.,-0.376947046632555,0.926234810420659));
#41809=DIRECTION('',(-1.,0.,0.));
#41810=DIRECTION('',(1.,0.,0.));
#41811=DIRECTION('center_axis',(-0.707106781186549,0.664463024388673,-0.241844762647975));
#41812=DIRECTION('ref_axis',(-0.323615577118184,0.,0.946188648339466));
#41813=DIRECTION('',(0.,-0.342020143325669,-0.939692620785908));
#41814=DIRECTION('',(0.,0.342020143325669,0.939692620785908));
#41815=DIRECTION('center_axis',(0.707106781186549,0.306761075170857,0.637100967476913));
#41816=DIRECTION('ref_axis',(0.669373784875799,0.,-0.742925794491649));
#41817=DIRECTION('',(0.,-0.900996828806872,0.433825672914779));
#41818=DIRECTION('center_axis',(0.,-0.246819851905205,-0.96906138128887));
#41819=DIRECTION('ref_axis',(0.,0.96906138128887,-0.246819851905205));
#41820=DIRECTION('center_axis',(0.,0.939692620785908,-0.342020143325669));
#41821=DIRECTION('ref_axis',(0.,0.342020143325669,0.939692620785908));
#41822=DIRECTION('center_axis',(0.561006631580399,0.449103523455305,-0.695397429203505));
#41823=DIRECTION('ref_axis',(-0.778302413620336,0.,-0.627889602520029));
#41824=DIRECTION('',(0.705516335778308,0.18003913904976,0.685443366267536));
#41825=DIRECTION('',(0.,-0.840043405623117,-0.542519194747167));
#41826=DIRECTION('',(-0.705516335778306,0.698825821880053,-0.117852325490936));
#41827=DIRECTION('center_axis',(0.561006631580396,0.736633774843142,0.37768007768899));
#41828=DIRECTION('ref_axis',(0.558457227212258,0.,-0.829533317820566));
#41829=DIRECTION('',(0.705516335778306,-0.664127077314135,0.2473498031698));
#41830=DIRECTION('',(0.,0.456239332177649,-0.889857107503274));
#41831=DIRECTION('',(-0.705516335778303,0.186803215041171,0.683630937568099));
#41832=DIRECTION('center_axis',(-0.561006631580406,0.449103523455303,-0.695397429203502));
#41833=DIRECTION('ref_axis',(-0.77830241362033,0.,0.627889602520036));
#41834=DIRECTION('',(0.,0.840043405623117,0.542519194747167));
#41835=DIRECTION('',(0.705516335778303,-0.180039139049758,-0.685443366267541));
#41836=DIRECTION('',(-0.705516335778306,-0.69882582188005,0.117852325490948));
#41837=DIRECTION('center_axis',(-0.70710678118655,-0.114142140686715,-0.697833484234922));
#41838=DIRECTION('ref_axis',(-0.702424227635741,0.,0.711758529580316));
#41839=DIRECTION('',(0.,0.986885577683101,-0.161421363397451));
#41840=DIRECTION('',(0.,-0.986885577683101,0.161421363397451));
#41841=DIRECTION('center_axis',(-0.561006631580396,0.736633774843142,0.377680077688989));
#41842=DIRECTION('ref_axis',(0.558457227212258,0.,0.829533317820566));
#41843=DIRECTION('',(0.705516335778308,0.664127077314134,-0.247349803169793));
#41844=DIRECTION('',(-0.705516335778302,-0.186803215041169,-0.683630937568101));
#41845=DIRECTION('',(0.,-0.456239332177649,0.889857107503274));
#41846=DIRECTION('center_axis',(-0.707106781186547,0.250066748640429,0.661412595302211));
#41847=DIRECTION('ref_axis',(0.683116152038586,0.,0.730309744439985));
#41848=DIRECTION('',(0.,0.935378662600772,-0.353647787425838));
#41849=DIRECTION('',(0.,-0.935378662600772,0.353647787425838));
#41850=DIRECTION('center_axis',(0.,0.889857107503274,0.456239332177649));
#41851=DIRECTION('ref_axis',(0.,-0.456239332177649,0.889857107503274));
#41852=DIRECTION('',(-1.,0.,0.));
#41853=DIRECTION('',(1.,0.,0.));
#41854=DIRECTION('center_axis',(-0.707106781186551,0.683012701892216,-0.183012701892218));
#41855=DIRECTION('ref_axis',(-0.250562807085729,0.,0.968100345886375));
#41856=DIRECTION('',(0.,-0.258819045102521,-0.965925826289068));
#41857=DIRECTION('',(0.,0.258819045102521,0.965925826289068));
#41858=DIRECTION('center_axis',(0.,0.542519194747167,-0.840043405623117));
#41859=DIRECTION('ref_axis',(-1.,0.,0.));
#41860=DIRECTION('',(-1.,0.,0.));
#41861=DIRECTION('',(1.,0.,0.));
#41862=DIRECTION('center_axis',(0.707106781186545,0.25006674864043,0.661412595302212));
#41863=DIRECTION('ref_axis',(0.683116152038587,0.,-0.730309744439983));
#41864=DIRECTION('',(0.,0.935378662600772,-0.353647787425838));
#41865=DIRECTION('',(0.,-0.935378662600772,0.353647787425838));
#41866=DIRECTION('center_axis',(0.707106781186552,0.683012701892215,-0.183012701892218));
#41867=DIRECTION('ref_axis',(-0.250562807085728,0.,-0.968100345886376));
#41868=DIRECTION('',(0.,-0.258819045102521,-0.965925826289068));
#41869=DIRECTION('',(0.,0.258819045102521,0.965925826289068));
#41870=DIRECTION('center_axis',(0.707106781186545,-0.114142140686716,-0.697833484234927));
#41871=DIRECTION('ref_axis',(-0.702424227635745,0.,-0.711758529580311));
#41872=DIRECTION('',(0.,0.986885577683101,-0.161421363397451));
#41873=DIRECTION('',(0.,-0.986885577683101,0.161421363397451));
#41874=DIRECTION('center_axis',(1.,0.,0.));
#41875=DIRECTION('ref_axis',(0.,-0.965925826289068,0.258819045102521));
#41876=DIRECTION('center_axis',(0.,-0.161421363397451,-0.986885577683101));
#41877=DIRECTION('ref_axis',(0.,0.986885577683101,-0.161421363397451));
#41878=DIRECTION('center_axis',(0.,0.965925826289068,-0.258819045102521));
#41879=DIRECTION('ref_axis',(0.,0.258819045102521,0.965925826289068));
#41880=DIRECTION('center_axis',(0.56100663158039,0.700913673242072,0.44044475474812));
#41881=DIRECTION('ref_axis',(0.617521420133027,0.,-0.786554064052109));
#41882=DIRECTION('',(0.70551633577831,-0.683157829093258,0.188526073789633));
#41883=DIRECTION('',(0.,0.532059360920026,-0.846707054687377));
#41884=DIRECTION('',(-0.705516335778307,0.126510010281474,0.697310488411391));
#41885=DIRECTION('center_axis',(0.,0.846707054687377,0.532059360920026));
#41886=DIRECTION('ref_axis',(1.,0.,0.));
#41887=DIRECTION('',(0.557191914001242,-0.44181344692932,0.703091778563841));
#41888=DIRECTION('',(1.,0.,0.));
#41889=DIRECTION('',(-1.,0.,0.));
#41890=DIRECTION('',(-0.557191914001257,-0.441813446929314,0.703091778563833));
#41891=DIRECTION('center_axis',(0.707106781186546,0.191469263158417,0.680690473905413));
#41892=DIRECTION('ref_axis',(0.6935215873247,0.,-0.72043584580074));
#41893=DIRECTION('',(0.,0.962641699975202,-0.270778428736215));
#41894=DIRECTION('',(0.,-0.962641699975202,0.270778428736215));
#41895=DIRECTION('center_axis',(0.561006631580394,0.508002428407532,-0.653609280881836));
#41896=DIRECTION('ref_axis',(-0.758814655754538,0.,-0.651306623804888));
#41897=DIRECTION('',(0.705516335778306,0.119613710071895,0.698526492205406));
#41898=DIRECTION('',(0.,-0.789563123475643,-0.613669352377473));
#41899=DIRECTION('',(-0.70551633577831,0.706438085609211,-0.0564971782546651));
#41900=DIRECTION('center_axis',(0.,0.613669352377473,-0.789563123475643));
#41901=DIRECTION('ref_axis',(-1.,0.,0.));
#41902=DIRECTION('',(0.557191914001254,0.655640386718963,0.509581057609707));
#41903=DIRECTION('',(1.,0.,0.));
#41904=DIRECTION('',(-1.,0.,0.));
#41905=DIRECTION('',(-0.557191914001241,0.65564038671897,0.509581057609713));
#41906=DIRECTION('center_axis',(0.707106781186543,0.696364240320024,-0.122787803968974));
#41907=DIRECTION('ref_axis',(-0.171087869746038,0.,-0.985255774317392));
#41908=DIRECTION('',(0.,-0.17364817766693,-0.984807753012208));
#41909=DIRECTION('',(0.,0.17364817766693,0.984807753012208));
#41910=DIRECTION('center_axis',(0.707106781186546,-0.0528875997482673,-0.705126160196081));
#41911=DIRECTION('ref_axis',(-0.706114387365562,0.,-0.708097784176279));
#41912=DIRECTION('',(0.,0.997198978933359,-0.0747943608453594));
#41913=DIRECTION('',(0.,-0.997198978933359,0.0747943608453594));
#41914=DIRECTION('center_axis',(-0.707106781186541,0.191469263158418,0.680690473905417));
#41915=DIRECTION('ref_axis',(0.693521587324705,0.,0.720435845800736));
#41916=DIRECTION('',(-0.595596683047434,-0.680145916919126,-0.427394575118983));
#41917=DIRECTION('',(0.,-0.962641699975202,0.270778428736215));
#41918=DIRECTION('',(0.,0.962641699975202,-0.270778428736215));
#41919=DIRECTION('center_axis',(0.,0.984807753012208,-0.17364817766693));
#41920=DIRECTION('ref_axis',(0.,0.17364817766693,0.984807753012208));
#41921=DIRECTION('',(0.,-0.17364817766693,-0.984807753012208));
#41922=DIRECTION('center_axis',(-0.707106781186541,0.696364240320026,-0.122787803968974));
#41923=DIRECTION('ref_axis',(-0.171087869746039,0.,0.985255774317391));
#41924=DIRECTION('',(0.595596683047432,0.492950545347766,-0.634243132390283));
#41925=DIRECTION('',(0.,0.17364817766693,0.984807753012208));
#41926=DIRECTION('center_axis',(-0.707106781186545,-0.0528875997482674,
-0.705126160196082));
#41927=DIRECTION('ref_axis',(-0.706114387365564,0.,0.708097784176278));
#41928=DIRECTION('',(0.,-0.997198978933359,0.0747943608453594));
#41929=DIRECTION('',(0.,0.997198978933359,-0.0747943608453594));
#41930=DIRECTION('center_axis',(0.,-0.0747943608453594,-0.997198978933359));
#41931=DIRECTION('ref_axis',(0.,0.997198978933359,-0.0747943608453594));
#41932=DIRECTION('center_axis',(0.,0.270778428736215,0.962641699975202));
#41933=DIRECTION('ref_axis',(0.,-0.962641699975202,0.270778428736215));
#41934=DIRECTION('center_axis',(0.561006631580398,0.563035128139334,-0.606846771272567));
#41935=DIRECTION('ref_axis',(-0.734296425103062,0.,-0.678828962317359));
#41936=DIRECTION('',(0.705516335778301,0.0582779485356274,0.706293409755774));
#41937=DIRECTION('',(0.,-0.733073789207258,-0.680149115692517));
#41938=DIRECTION('',(-0.705516335778312,0.708673928947909,0.00528794662205492));
#41939=DIRECTION('center_axis',(0.561006631580394,0.659859195364387,0.499857381275784));
#41940=DIRECTION('ref_axis',(0.665244232298934,0.,-0.746625817523746));
#41941=DIRECTION('',(0.705516335778315,-0.696989337290999,0.128267547152788));
#41942=DIRECTION('',(0.,0.603830096659557,-0.797113049929625));
#41943=DIRECTION('',(-0.705516335778304,0.0652539879547269,0.70568308539029));
#41944=DIRECTION('center_axis',(-0.561006631580408,0.56303512813933,-0.606846771272562));
#41945=DIRECTION('ref_axis',(-0.734296425103054,0.,0.678828962317369));
#41946=DIRECTION('',(0.,0.733073789207258,0.680149115692517));
#41947=DIRECTION('',(0.705516335778306,-0.0582779485356024,-0.706293409755772));
#41948=DIRECTION('',(-0.705516335778301,-0.70867392894792,-0.00528794662205795));
#41949=DIRECTION('center_axis',(-0.707106781186548,0.00876944775867127,
-0.707052400311326));
#41950=DIRECTION('ref_axis',(-0.707079589180542,0.,0.707133972146916));
#41951=DIRECTION('',(0.,0.999923093828728,0.0124018719548352));
#41952=DIRECTION('',(0.,-0.999923093828728,-0.0124018719548352));
#41953=DIRECTION('center_axis',(-0.561006631580406,0.659859195364381,0.499857381275779));
#41954=DIRECTION('ref_axis',(0.665244232298923,0.,0.746625817523755));
#41955=DIRECTION('',(0.705516335778304,0.696989337291011,-0.128267547152789));
#41956=DIRECTION('',(-0.705516335778308,-0.065253987954752,-0.705683085390284));
#41957=DIRECTION('',(0.,-0.603830096659557,0.797113049929625));
#41958=DIRECTION('center_axis',(-0.707106781186545,0.131414580971466,0.694787886990049));
#41959=DIRECTION('ref_axis',(0.700866150214856,0.,0.713292814686232));
#41960=DIRECTION('',(0.,0.982578452753869,-0.185848282703424));
#41961=DIRECTION('',(0.,-0.982578452753869,0.185848282703424));
#41962=DIRECTION('center_axis',(0.,0.797113049929625,0.603830096659558));
#41963=DIRECTION('ref_axis',(1.,0.,0.));
#41964=DIRECTION('',(-1.,0.,0.));
#41965=DIRECTION('',(1.,0.,0.));
#41966=DIRECTION('center_axis',(-0.707106781186556,0.70441602640275,-0.0616284167162187));
#41967=DIRECTION('ref_axis',(-0.0868265938642456,0.,0.996223440096615));
#41968=DIRECTION('',(0.,-0.0871557427476582,-0.996194698091746));
#41969=DIRECTION('',(0.,0.0871557427476582,0.996194698091746));
#41970=DIRECTION('center_axis',(0.,0.680149115692517,-0.733073789207258));
#41971=DIRECTION('ref_axis',(-1.,0.,0.));
#41972=DIRECTION('',(-1.,0.,0.));
#41973=DIRECTION('',(1.,0.,0.));
#41974=DIRECTION('center_axis',(0.707106781186546,0.131414580971466,0.694787886990048));
#41975=DIRECTION('ref_axis',(0.700866150214854,0.,-0.713292814686234));
#41976=DIRECTION('',(0.,0.982578452753869,-0.185848282703424));
#41977=DIRECTION('',(0.,-0.982578452753869,0.185848282703424));
#41978=DIRECTION('center_axis',(0.707106781186545,0.704416026402761,-0.0616284167162196));
#41979=DIRECTION('ref_axis',(-0.0868265938642483,0.,-0.996223440096615));
#41980=DIRECTION('',(0.,-0.0871557427476582,-0.996194698091746));
#41981=DIRECTION('',(0.,0.0871557427476582,0.996194698091746));
#41982=DIRECTION('center_axis',(0.707106781186549,0.00876944775867125,-0.707052400311324));
#41983=DIRECTION('ref_axis',(-0.70707958918054,0.,-0.707133972146918));
#41984=DIRECTION('',(0.,0.999923093828728,0.0124018719548352));
#41985=DIRECTION('',(0.,-0.999923093828728,-0.0124018719548352));
#41986=DIRECTION('center_axis',(1.,0.,0.));
#41987=DIRECTION('ref_axis',(0.,-0.996194698091746,0.0871557427476582));
#41988=DIRECTION('center_axis',(0.,0.0124018719548352,-0.999923093828728));
#41989=DIRECTION('ref_axis',(0.,0.999923093828728,0.0124018719548352));
#41990=DIRECTION('center_axis',(0.,0.996194698091746,-0.0871557427476582));
#41991=DIRECTION('ref_axis',(0.,0.0871557427476582,0.996194698091746));
#41992=DIRECTION('center_axis',(0.561006631580416,0.613782790576088,-0.555465791309803));
#41993=DIRECTION('ref_axis',(-0.703588880269148,0.,-0.710607266752604));
#41994=DIRECTION('',(0.705516335778304,-0.00350134337823141,0.708685007986272));
#41995=DIRECTION('',(0.,-0.671005320760942,-0.741452533551882));
#41996=DIRECTION('',(-0.705516335778299,0.705516335778311,0.0670328270320439));
#41997=DIRECTION('center_axis',(0.561006631580416,0.613782790576088,0.555465791309803));
#41998=DIRECTION('ref_axis',(0.703588880269148,0.,-0.710607266752604));
#41999=DIRECTION('',(0.705516335778299,-0.705516335778311,0.0670328270320437));
#42000=DIRECTION('',(0.,0.671005320760943,-0.741452533551882));
#42001=DIRECTION('',(-0.705516335778305,0.00350134337823141,0.708685007986272));
#42002=DIRECTION('center_axis',(-0.561006631580414,0.613782790576089,-0.555465791309803));
#42003=DIRECTION('ref_axis',(-0.703588880269149,0.,0.710607266752603));
#42004=DIRECTION('',(0.,0.671005320760942,0.741452533551882));
#42005=DIRECTION('',(0.705516335778306,0.0035013433782314,-0.708685007986271));
#42006=DIRECTION('',(-0.7055163357783,-0.70551633577831,-0.067032827032044));
#42007=DIRECTION('center_axis',(-0.707106781186547,0.070359754473029,-0.703597544730292));
#42008=DIRECTION('ref_axis',(-0.705345615858598,0.,0.708863570928183));
#42009=DIRECTION('',(0.,0.995037190209989,0.0995037190209986));
#42010=DIRECTION('',(0.,-0.995037190209989,-0.0995037190209986));
#42011=DIRECTION('center_axis',(-0.561006631580415,0.613782790576088,0.555465791309804));
#42012=DIRECTION('ref_axis',(0.703588880269149,0.,0.710607266752603));
#42013=DIRECTION('',(0.7055163357783,0.70551633577831,-0.0670328270320424));
#42014=DIRECTION('',(-0.705516335778306,-0.0035013433782314,-0.708685007986271));
#42015=DIRECTION('',(0.,-0.671005320760943,0.741452533551882));
#42016=DIRECTION('center_axis',(-0.707106781186548,0.0703597544730292,0.703597544730292));
#42017=DIRECTION('ref_axis',(0.705345615858598,0.,0.708863570928183));
#42018=DIRECTION('',(0.,0.995037190209989,-0.099503719020999));
#42019=DIRECTION('',(0.,-0.995037190209989,0.099503719020999));
#42020=DIRECTION('center_axis',(0.,0.741452533551882,0.671005320760943));
#42021=DIRECTION('ref_axis',(1.,0.,0.));
#42022=DIRECTION('',(-1.,0.,0.));
#42023=DIRECTION('',(1.,0.,0.));
#42024=DIRECTION('center_axis',(-0.707106781186552,0.707106781186543,-1.29893408435323E-16));
#42025=DIRECTION('ref_axis',(-1.83697019872101E-16,0.,1.));
#42026=DIRECTION('',(0.,-1.83697019872103E-16,-1.));
#42027=DIRECTION('',(0.,1.83697019872103E-16,1.));
#42028=DIRECTION('center_axis',(0.,0.741452533551882,-0.671005320760942));
#42029=DIRECTION('ref_axis',(-1.,0.,0.));
#42030=DIRECTION('',(-1.,0.,0.));
#42031=DIRECTION('',(1.,0.,0.));
#42032=DIRECTION('center_axis',(0.707106781186548,0.0703597544730291,0.703597544730291));
#42033=DIRECTION('ref_axis',(0.705345615858597,0.,-0.708863570928184));
#42034=DIRECTION('',(0.,0.995037190209989,-0.099503719020999));
#42035=DIRECTION('',(0.,-0.995037190209989,0.099503719020999));
#42036=DIRECTION('center_axis',(0.707106781186554,0.707106781186541,-1.29893408435323E-16));
#42037=DIRECTION('ref_axis',(-1.836970198721E-16,0.,-1.));
#42038=DIRECTION('',(0.,-1.83697019872103E-16,-1.));
#42039=DIRECTION('',(0.,1.83697019872103E-16,1.));
#42040=DIRECTION('center_axis',(0.707106781186549,0.0703597544730288,-0.70359754473029));
#42041=DIRECTION('ref_axis',(-0.705345615858597,0.,-0.708863570928184));
#42042=DIRECTION('',(0.,0.995037190209989,0.0995037190209986));
#42043=DIRECTION('',(0.,-0.995037190209989,-0.0995037190209986));
#42044=DIRECTION('center_axis',(1.,0.,0.));
#42045=DIRECTION('ref_axis',(0.,-1.,1.83697019872103E-16));
#42046=DIRECTION('center_axis',(0.,0.0995037190209986,-0.995037190209989));
#42047=DIRECTION('ref_axis',(0.,0.995037190209989,0.0995037190209986));
#42048=DIRECTION('center_axis',(0.,1.,-1.83697019872103E-16));
#42049=DIRECTION('ref_axis',(0.,1.83697019872103E-16,1.));
#42050=DIRECTION('center_axis',(0.707106781186548,0.131414580971466,-0.694787886990046));
#42051=DIRECTION('ref_axis',(-0.700866150214853,0.,-0.713292814686235));
#42052=DIRECTION('',(0.595596683047426,-0.640307864722779,0.485046832292573));
#42053=DIRECTION('',(0.,-0.98257845275387,-0.185848282703424));
#42054=DIRECTION('',(0.,0.98257845275387,0.185848282703424));
#42055=DIRECTION('',(0.557191914001245,0.501410699557114,0.661909722954177));
#42056=DIRECTION('center_axis',(1.,0.,0.));
#42057=DIRECTION('ref_axis',(0.,-0.996194698091746,-0.0871557427476579));
#42058=DIRECTION('',(0.,0.0871557427476579,-0.996194698091746));
#42059=DIRECTION('',(0.,0.999923093828728,-0.0124018719548356));
#42060=DIRECTION('center_axis',(0.707106781186545,0.704416026402761,0.0616284167162194));
#42061=DIRECTION('ref_axis',(0.0868265938642479,0.,-0.996223440096615));
#42062=DIRECTION('',(0.557191914001243,-0.501410699557115,-0.661909722954177));
#42063=DIRECTION('',(0.,-0.0871557427476579,0.996194698091746));
#42064=DIRECTION('',(0.7055163357783,-0.708673928947921,0.00528794662205797));
#42065=DIRECTION('center_axis',(0.,0.797113049929628,-0.603830096659555));
#42066=DIRECTION('ref_axis',(-1.,0.,0.));
#42067=DIRECTION('',(-1.,0.,0.));
#42068=DIRECTION('',(0.,0.603830096659555,0.797113049929628));
#42069=DIRECTION('',(1.,0.,0.));
#42070=DIRECTION('center_axis',(0.561006631580408,0.56303512813933,0.606846771272561));
#42071=DIRECTION('ref_axis',(0.734296425103052,0.,-0.67882896231737));
#42072=DIRECTION('',(0.,0.733073789207257,-0.680149115692518));
#42073=DIRECTION('',(-0.705516335778304,-0.0582779485356025,0.706293409755774));
#42074=DIRECTION('center_axis',(-0.561006631580394,0.659859195364389,-0.499857381275781));
#42075=DIRECTION('ref_axis',(-0.665244232298933,0.,0.746625817523747));
#42076=DIRECTION('',(0.705516335778303,0.0652539879547265,-0.705683085390291));
#42077=DIRECTION('',(-0.705516335778317,-0.696989337290998,-0.128267547152788));
#42078=DIRECTION('center_axis',(-0.707106781186548,0.131414580971466,-0.694787886990046));
#42079=DIRECTION('ref_axis',(-0.700866150214853,0.,0.713292814686235));
#42080=DIRECTION('',(0.,0.98257845275387,0.185848282703424));
#42081=DIRECTION('',(0.,-0.98257845275387,-0.185848282703424));
#42082=DIRECTION('center_axis',(-0.561006631580393,0.563035128139338,0.606846771272568));
#42083=DIRECTION('ref_axis',(0.734296425103066,0.,0.678828962317356));
#42084=DIRECTION('',(0.705516335778314,0.708673928947907,-0.00528794662205805));
#42085=DIRECTION('',(-0.705516335778305,0.0582779485356274,-0.706293409755771));
#42086=DIRECTION('',(0.,-0.733073789207257,0.680149115692518));
#42087=DIRECTION('center_axis',(-0.707106781186548,0.00876944775867152,
0.707052400311326));
#42088=DIRECTION('ref_axis',(0.707079589180542,0.,0.707133972146916));
#42089=DIRECTION('',(0.,0.999923093828728,-0.0124018719548356));
#42090=DIRECTION('',(0.,-0.999923093828728,0.0124018719548356));
#42091=DIRECTION('center_axis',(0.,0.680149115692518,0.733073789207257));
#42092=DIRECTION('ref_axis',(1.,0.,0.));
#42093=DIRECTION('',(-1.,0.,0.));
#42094=DIRECTION('',(1.,0.,0.));
#42095=DIRECTION('center_axis',(-0.707106781186531,0.704416026402775,0.0616284167162206));
#42096=DIRECTION('ref_axis',(0.0868265938642514,0.,0.996223440096614));
#42097=DIRECTION('',(0.,0.0871557427476579,-0.996194698091746));
#42098=DIRECTION('',(0.,-0.0871557427476579,0.996194698091746));
#42099=DIRECTION('center_axis',(0.707106781186549,0.0087694477586715,0.707052400311324));
#42100=DIRECTION('ref_axis',(0.70707958918054,0.,-0.707133972146918));
#42101=DIRECTION('',(0.,-0.999923093828728,0.0124018719548356));
#42102=DIRECTION('center_axis',(0.,0.185848282703424,-0.98257845275387));
#42103=DIRECTION('ref_axis',(0.,0.98257845275387,0.185848282703424));
#42104=DIRECTION('center_axis',(0.,0.996194698091746,0.0871557427476579));
#42105=DIRECTION('ref_axis',(0.,-0.0871557427476579,0.996194698091746));
#42106=DIRECTION('center_axis',(0.561006631580397,0.700913673242075,-0.440444754748105));
#42107=DIRECTION('ref_axis',(-0.61752142013301,0.,-0.786554064052123));
#42108=DIRECTION('',(0.705516335778305,-0.126510010281499,0.697310488411388));
#42109=DIRECTION('',(0.,-0.532059360920012,-0.846707054687386));
#42110=DIRECTION('',(-0.705516335778308,0.683157829093256,0.188526073789645));
#42111=DIRECTION('center_axis',(0.561006631580402,0.508002428407548,0.653609280881817));
#42112=DIRECTION('ref_axis',(0.758814655754524,0.,-0.651306623804904));
#42113=DIRECTION('',(0.70551633577831,-0.706438085609211,-0.0564971782546651));
#42114=DIRECTION('',(0.,0.789563123475625,-0.613669352377496));
#42115=DIRECTION('',(-0.705516335778302,-0.119613710071869,0.698526492205414));
#42116=DIRECTION('center_axis',(-0.561006631580396,0.700913673242077,-0.440444754748103));
#42117=DIRECTION('ref_axis',(-0.617521420133008,0.,0.786554064052124));
#42118=DIRECTION('',(0.,0.532059360920012,0.846707054687386));
#42119=DIRECTION('',(0.705516335778306,0.126510010281499,-0.697310488411387));
#42120=DIRECTION('',(-0.70551633577831,-0.683157829093255,-0.188526073789644));
#42121=DIRECTION('center_axis',(-0.707106781186544,0.191469263158417,-0.680690473905414));
#42122=DIRECTION('ref_axis',(-0.693521587324702,0.,0.720435845800739));
#42123=DIRECTION('',(0.,0.962641699975202,0.270778428736215));
#42124=DIRECTION('',(0.,-0.962641699975202,-0.270778428736215));
#42125=DIRECTION('center_axis',(-0.561006631580396,0.50800242840755,0.65360928088182));
#42126=DIRECTION('ref_axis',(0.758814655754529,0.,0.651306623804899));
#42127=DIRECTION('',(0.705516335778312,0.70643808560921,0.0564971782546587));
#42128=DIRECTION('',(-0.705516335778307,0.119613710071869,-0.69852649220541));
#42129=DIRECTION('',(0.,-0.789563123475625,0.613669352377496));
#42130=DIRECTION('center_axis',(-0.707106781186545,-0.0528875997482672,
0.705126160196082));
#42131=DIRECTION('ref_axis',(0.706114387365564,0.,0.708097784176278));
#42132=DIRECTION('',(0.,0.997198978933359,0.0747943608453591));
#42133=DIRECTION('',(0.,-0.997198978933359,-0.0747943608453591));
#42134=DIRECTION('center_axis',(0.,0.613669352377496,0.789563123475625));
#42135=DIRECTION('ref_axis',(1.,0.,0.));
#42136=DIRECTION('',(-1.,0.,0.));
#42137=DIRECTION('',(1.,0.,0.));
#42138=DIRECTION('center_axis',(-0.707106781186541,0.696364240320025,0.122787803968974));
#42139=DIRECTION('ref_axis',(0.171087869746038,0.,0.985255774317391));
#42140=DIRECTION('',(0.,0.17364817766693,-0.984807753012208));
#42141=DIRECTION('',(0.,-0.17364817766693,0.984807753012208));
#42142=DIRECTION('center_axis',(0.,0.846707054687386,-0.532059360920012));
#42143=DIRECTION('ref_axis',(-1.,0.,0.));
#42144=DIRECTION('',(-1.,0.,0.));
#42145=DIRECTION('',(1.,0.,0.));
#42146=DIRECTION('center_axis',(0.707106781186549,-0.0528875997482668,0.705126160196077));
#42147=DIRECTION('ref_axis',(0.706114387365559,0.,-0.708097784176282));
#42148=DIRECTION('',(0.,0.997198978933359,0.0747943608453591));
#42149=DIRECTION('',(0.,-0.997198978933359,-0.0747943608453591));
#42150=DIRECTION('center_axis',(0.707106781186543,0.696364240320023,0.122787803968973));
#42151=DIRECTION('ref_axis',(0.171087869746037,0.,-0.985255774317392));
#42152=DIRECTION('',(0.,0.17364817766693,-0.984807753012208));
#42153=DIRECTION('',(0.,-0.17364817766693,0.984807753012208));
#42154=DIRECTION('center_axis',(0.707106781186546,0.191469263158416,-0.680690473905413));
#42155=DIRECTION('ref_axis',(-0.6935215873247,0.,-0.72043584580074));
#42156=DIRECTION('',(0.,0.962641699975202,0.270778428736215));
#42157=DIRECTION('',(0.,-0.962641699975202,-0.270778428736215));
#42158=DIRECTION('center_axis',(1.,0.,0.));
#42159=DIRECTION('ref_axis',(0.,-0.984807753012208,-0.17364817766693));
#42160=DIRECTION('center_axis',(0.,0.270778428736215,-0.962641699975202));
#42161=DIRECTION('ref_axis',(0.,0.962641699975202,0.270778428736215));
#42162=DIRECTION('center_axis',(0.,0.984807753012208,0.17364817766693));
#42163=DIRECTION('ref_axis',(0.,-0.17364817766693,0.984807753012208));
#42164=DIRECTION('center_axis',(0.561006631580423,0.449103523455315,0.69539742920348));
#42165=DIRECTION('ref_axis',(0.778302413620312,0.,-0.627889602520059));
#42166=DIRECTION('',(0.705516335778304,-0.698825821880051,-0.117852325490961));
#42167=DIRECTION('',(0.,0.840043405623103,-0.542519194747189));
#42168=DIRECTION('',(-0.705516335778305,-0.18003913904971,0.685443366267552));
#42169=DIRECTION('center_axis',(0.,0.542519194747189,0.840043405623103));
#42170=DIRECTION('ref_axis',(1.,0.,0.));
#42171=DIRECTION('',(0.557191914001254,-0.697558392670345,0.450499122958952));
#42172=DIRECTION('',(1.,0.,0.));
#42173=DIRECTION('',(-1.,0.,0.));
#42174=DIRECTION('',(-0.557191914001225,-0.697558392670361,0.450499122958962));
#42175=DIRECTION('center_axis',(0.707106781186551,-0.114142140686715,0.697833484234921));
#42176=DIRECTION('ref_axis',(0.702424227635739,0.,-0.711758529580317));
#42177=DIRECTION('',(0.,0.986885577683101,0.161421363397451));
#42178=DIRECTION('',(0.,-0.986885577683101,-0.161421363397451));
#42179=DIRECTION('center_axis',(0.561006631580397,0.736633774843151,-0.377680077688971));
#42180=DIRECTION('ref_axis',(-0.558457227212239,0.,-0.829533317820579));
#42181=DIRECTION('',(0.705516335778306,-0.186803215041196,0.68363093756809));
#42182=DIRECTION('',(0.,-0.456239332177628,-0.889857107503285));
#42183=DIRECTION('',(-0.705516335778302,0.664127077314132,0.247349803169817));
#42184=DIRECTION('center_axis',(0.,0.889857107503285,-0.456239332177628));
#42185=DIRECTION('ref_axis',(0.,0.456239332177628,0.889857107503285));
#42186=DIRECTION('',(0.557191914001234,0.378853727196106,0.738922881200238));
#42187=DIRECTION('',(1.,0.,0.));
#42188=DIRECTION('',(-1.,0.,0.));
#42189=DIRECTION('',(-0.557191914001251,0.3788537271961,0.738922881200227));
#42190=DIRECTION('center_axis',(0.707106781186553,0.683012701892214,0.183012701892218));
#42191=DIRECTION('ref_axis',(0.250562807085727,0.,-0.968100345886376));
#42192=DIRECTION('',(0.,0.25881904510252,-0.965925826289068));
#42193=DIRECTION('',(0.,-0.25881904510252,0.965925826289068));
#42194=DIRECTION('center_axis',(0.707106781186545,0.250066748640429,-0.661412595302212));
#42195=DIRECTION('ref_axis',(-0.683116152038588,0.,-0.730309744439983));
#42196=DIRECTION('',(0.,0.935378662600772,0.353647787425838));
#42197=DIRECTION('',(0.,-0.935378662600772,-0.353647787425838));
#42198=DIRECTION('center_axis',(-0.70710678118655,-0.114142140686715,0.697833484234922));
#42199=DIRECTION('ref_axis',(0.702424227635741,0.,0.711758529580316));
#42200=DIRECTION('',(-0.595596683047418,-0.435796788410821,-0.674793116705948));
#42201=DIRECTION('',(0.,-0.986885577683101,-0.161421363397451));
#42202=DIRECTION('',(0.,0.986885577683101,0.161421363397451));
#42203=DIRECTION('center_axis',(0.,0.965925826289068,0.25881904510252));
#42204=DIRECTION('ref_axis',(0.,-0.25881904510252,0.965925826289068));
#42205=DIRECTION('',(0.,0.25881904510252,-0.965925826289068));
#42206=DIRECTION('center_axis',(-0.707106781186552,0.683012701892215,0.183012701892218));
#42207=DIRECTION('ref_axis',(0.250562807085728,0.,0.968100345886376));
#42208=DIRECTION('',(0.595596683047428,0.714807648004415,-0.366489587160805));
#42209=DIRECTION('',(0.,-0.25881904510252,0.965925826289068));
#42210=DIRECTION('center_axis',(-0.707106781186544,0.25006674864043,-0.661412595302213));
#42211=DIRECTION('ref_axis',(-0.683116152038589,0.,0.730309744439982));
#42212=DIRECTION('',(0.,-0.935378662600772,-0.353647787425838));
#42213=DIRECTION('',(0.,0.935378662600772,0.353647787425838));
#42214=DIRECTION('center_axis',(0.,0.353647787425838,-0.935378662600772));
#42215=DIRECTION('ref_axis',(0.,0.935378662600772,0.353647787425838));
#42216=DIRECTION('center_axis',(0.,-0.161421363397451,0.986885577683101));
#42217=DIRECTION('ref_axis',(0.,-0.986885577683101,-0.161421363397451));
#42218=DIRECTION('center_axis',(0.561006631580414,0.766747648626018,-0.312041027189167));
#42219=DIRECTION('ref_axis',(-0.486084108127399,0.,-0.873912032086749));
#42220=DIRECTION('',(0.705516335778304,-0.245674734539573,0.66474854250225));
#42221=DIRECTION('',(0.,-0.376947046632547,-0.926234810420662));
#42222=DIRECTION('',(-0.7055163357783,0.640041917465767,0.304291051193926));
#42223=DIRECTION('center_axis',(0.561006631580401,0.386786669513441,0.731893183196505));
#42224=DIRECTION('ref_axis',(0.793664727118314,0.,-0.60835540675514));
#42225=DIRECTION('',(0.705516335778305,-0.685895071683811,-0.178310545369065));
#42226=DIRECTION('',(0.,0.884130450221741,-0.467240138462762));
#42227=DIRECTION('',(-0.70551633577831,-0.23909436146888,0.667143602430344));
#42228=DIRECTION('center_axis',(-0.561006631580397,0.766747648626028,-0.312041027189172));
#42229=DIRECTION('ref_axis',(-0.486084108127415,0.,0.87391203208674));
#42230=DIRECTION('',(0.,0.376947046632547,0.926234810420662));
#42231=DIRECTION('',(0.705516335778304,0.245674734539547,-0.66474854250226));
#42232=DIRECTION('',(-0.705516335778316,-0.640041917465754,-0.304291051193919));
#42233=DIRECTION('center_axis',(-0.707106781186547,0.306761075170857,-0.637100967476915));
#42234=DIRECTION('ref_axis',(-0.669373784875801,0.,0.742925794491647));
#42235=DIRECTION('',(0.,0.900996828806872,0.433825672914778));
#42236=DIRECTION('',(0.,-0.900996828806872,-0.433825672914778));
#42237=DIRECTION('center_axis',(-0.561006631580399,0.386786669513442,0.731893183196506));
#42238=DIRECTION('ref_axis',(0.793664727118316,0.,0.608355406755138));
#42239=DIRECTION('',(0.705516335778319,0.685895071683797,0.178310545369067));
#42240=DIRECTION('',(-0.705516335778301,0.239094361468901,-0.667143602430345));
#42241=DIRECTION('',(0.,-0.884130450221741,0.467240138462762));
#42242=DIRECTION('center_axis',(-0.707106781186545,-0.17452799101363,0.685229874095366));
#42243=DIRECTION('ref_axis',(0.695910561235547,0.,0.718128463967852));
#42244=DIRECTION('',(0.,0.96906138128887,0.246819851905204));
#42245=DIRECTION('',(0.,-0.96906138128887,-0.246819851905204));
#42246=DIRECTION('center_axis',(0.,0.467240138462762,0.884130450221741));
#42247=DIRECTION('ref_axis',(1.,0.,0.));
#42248=DIRECTION('',(-1.,0.,0.));
#42249=DIRECTION('',(1.,0.,0.));
#42250=DIRECTION('center_axis',(-0.707106781186536,0.664463024388686,0.241844762647979));
#42251=DIRECTION('ref_axis',(0.323615577118194,0.,0.946188648339462));
#42252=DIRECTION('',(0.,0.342020143325668,-0.939692620785909));
#42253=DIRECTION('',(0.,-0.342020143325668,0.939692620785909));
#42254=DIRECTION('center_axis',(0.,0.926234810420662,-0.376947046632547));
#42255=DIRECTION('ref_axis',(0.,0.376947046632547,0.926234810420662));
#42256=DIRECTION('',(-1.,0.,0.));
#42257=DIRECTION('',(1.,0.,0.));
#42258=DIRECTION('center_axis',(0.70710678118654,-0.174527991013631,0.68522987409537));
#42259=DIRECTION('ref_axis',(0.695910561235552,0.,-0.718128463967847));
#42260=DIRECTION('',(0.,0.96906138128887,0.246819851905204));
#42261=DIRECTION('',(0.,-0.96906138128887,-0.246819851905204));
#42262=DIRECTION('center_axis',(0.707106781186551,0.664463024388672,0.241844762647974));
#42263=DIRECTION('ref_axis',(0.323615577118181,0.,-0.946188648339466));
#42264=DIRECTION('',(0.,0.342020143325668,-0.939692620785909));
#42265=DIRECTION('',(0.,-0.342020143325668,0.939692620785909));
#42266=DIRECTION('center_axis',(0.707106781186549,0.306761075170856,-0.637100967476913));
#42267=DIRECTION('ref_axis',(-0.669373784875799,0.,-0.742925794491649));
#42268=DIRECTION('',(0.,0.900996828806872,0.433825672914778));
#42269=DIRECTION('',(0.,-0.900996828806872,-0.433825672914778));
#42270=DIRECTION('center_axis',(1.,0.,0.));
#42271=DIRECTION('ref_axis',(0.,-0.939692620785909,-0.342020143325668));
#42272=DIRECTION('center_axis',(0.,0.433825672914778,-0.900996828806872));
#42273=DIRECTION('ref_axis',(0.,0.900996828806872,0.433825672914778));
#42274=DIRECTION('center_axis',(0.,0.939692620785909,0.342020143325668));
#42275=DIRECTION('ref_axis',(0.,-0.342020143325668,0.939692620785909));
#42276=DIRECTION('center_axis',(0.561006631580415,0.791026109827961,-0.24402715605694));
#42277=DIRECTION('ref_axis',(-0.398879012810059,0.,-0.917003562228453));
#42278=DIRECTION('',(0.705516335778313,-0.302676520965626,0.640807009641818));
#42279=DIRECTION('',(0.,-0.294785966455749,-0.955563307154869));
#42280=DIRECTION('',(-0.705516335778295,0.611085652157605,0.358916460582518));
#42281=DIRECTION('center_axis',(0.561006631580423,0.321526135468429,0.762818788136163));
#42282=DIRECTION('ref_axis',(0.805595332751379,0.,-0.592466167683181));
#42283=DIRECTION('',(0.705516335778303,-0.667744245837286,-0.237411714330086));
#42284=DIRECTION('',(0.,0.921488728241597,-0.388405102597383));
#42285=DIRECTION('',(-0.705516335778304,-0.296329931428055,0.643766472946362));
#42286=DIRECTION('center_axis',(-0.561006631580412,0.791026109827963,-0.244027156056944));
#42287=DIRECTION('ref_axis',(-0.398879012810066,0.,0.91700356222845));
#42288=DIRECTION('',(0.,0.294785966455749,0.955563307154869));
#42289=DIRECTION('',(0.705516335778314,0.302676520965625,-0.640807009641816));
#42290=DIRECTION('',(-0.705516335778296,-0.611085652157604,-0.358916460582518));
#42291=DIRECTION('center_axis',(-0.70710678118654,0.361120764691836,-0.607940616597043));
#42292=DIRECTION('ref_axis',(-0.65193371809419,0.,0.758275957163278));
#42293=DIRECTION('',(0.,0.859757865108992,0.510701883081733));
#42294=DIRECTION('',(0.,-0.859757865108992,-0.510701883081733));
#42295=DIRECTION('center_axis',(-0.561006631580421,0.321526135468429,0.762818788136165));
#42296=DIRECTION('ref_axis',(0.80559533275138,0.,0.592466167683179));
#42297=DIRECTION('',(0.705516335778305,0.667744245837285,0.237411714330086));
#42298=DIRECTION('',(-0.705516335778306,0.296329931428054,-0.643766472946361));
#42299=DIRECTION('',(0.,-0.921488728241597,0.388405102597383));
#42300=DIRECTION('center_axis',(-0.70710678118655,-0.233585577946046,0.667411250860823));
#42301=DIRECTION('ref_axis',(0.686399640790371,0.,0.727224541062009));
#42302=DIRECTION('',(0.,0.943862042647771,0.330339892306057));
#42303=DIRECTION('',(0.,-0.943862042647771,-0.330339892306057));
#42304=DIRECTION('center_axis',(0.,0.388405102597383,0.921488728241597));
#42305=DIRECTION('ref_axis',(1.,0.,0.));
#42306=DIRECTION('',(-1.,0.,0.));
#42307=DIRECTION('',(1.,0.,0.));
#42308=DIRECTION('center_axis',(-0.707106781186552,0.640856382055784,0.298836238730117));
#42309=DIRECTION('ref_axis',(0.38928162063502,0.,0.921118787038769));
#42310=DIRECTION('',(0.,0.422618261740699,-0.90630778703665));
#42311=DIRECTION('',(0.,-0.422618261740699,0.90630778703665));
#42312=DIRECTION('center_axis',(0.,0.955563307154869,-0.294785966455749));
#42313=DIRECTION('ref_axis',(0.,0.294785966455749,0.955563307154869));
#42314=DIRECTION('',(-1.,0.,0.));
#42315=DIRECTION('',(1.,0.,0.));
#42316=DIRECTION('center_axis',(0.707106781186551,-0.233585577946045,0.667411250860822));
#42317=DIRECTION('ref_axis',(0.68639964079037,0.,-0.72722454106201));
#42318=DIRECTION('',(0.,0.943862042647771,0.330339892306057));
#42319=DIRECTION('',(0.,-0.943862042647771,-0.330339892306057));
#42320=DIRECTION('center_axis',(0.707106781186554,0.640856382055783,0.298836238730117));
#42321=DIRECTION('ref_axis',(0.389281620635018,0.,-0.921118787038769));
#42322=DIRECTION('',(0.,0.422618261740699,-0.90630778703665));
#42323=DIRECTION('',(0.,-0.422618261740699,0.90630778703665));
#42324=DIRECTION('center_axis',(0.707106781186542,0.361120764691835,-0.607940616597042));
#42325=DIRECTION('ref_axis',(-0.651933718094189,0.,-0.758275957163279));
#42326=DIRECTION('',(0.,0.859757865108992,0.510701883081733));
#42327=DIRECTION('',(0.,-0.859757865108992,-0.510701883081733));
#42328=DIRECTION('center_axis',(1.,0.,0.));
#42329=DIRECTION('ref_axis',(0.,-0.90630778703665,-0.422618261740699));
#42330=DIRECTION('center_axis',(0.,0.510701883081733,-0.859757865108992));
#42331=DIRECTION('ref_axis',(0.,0.859757865108992,0.510701883081733));
#42332=DIRECTION('center_axis',(0.,0.90630778703665,0.422618261740699));
#42333=DIRECTION('ref_axis',(0.,-0.422618261740699,0.90630778703665));
#42334=DIRECTION('center_axis',(0.707106781186547,0.412732107142825,-0.574153470540276));
#42335=DIRECTION('ref_axis',(-0.630347388214433,0.,-0.776313190774988));
#42336=DIRECTION('',(0.595596683047424,-0.785305653025387,0.168995924416173));
#42337=DIRECTION('',(0.,-0.81197562492164,-0.583691343548209));
#42338=DIRECTION('',(0.,0.81197562492164,0.583691343548209));
#42339=DIRECTION('',(0.557191914001233,0.17469728496797,0.81179925449366));
#42340=DIRECTION('center_axis',(1.,0.,0.));
#42341=DIRECTION('ref_axis',(0.,-0.866025403784439,-0.5));
#42342=DIRECTION('',(0.,0.5,-0.866025403784438));
#42343=DIRECTION('',(0.,0.911479343942638,0.411345846661781));
#42344=DIRECTION('center_axis',(0.707106781186549,0.612372435695794,0.353553390593273));
#42345=DIRECTION('ref_axis',(0.447213595499957,0.,-0.894427190999916));
#42346=DIRECTION('',(0.557191914001247,-0.174697284967968,-0.811799254493651));
#42347=DIRECTION('',(0.,-0.5,0.866025403784439));
#42348=DIRECTION('',(0.705516335778306,-0.644511483084942,-0.29470603679192));
#42349=DIRECTION('center_axis',(0.,0.977619390136729,-0.210381387077589));
#42350=DIRECTION('ref_axis',(0.,0.210381387077589,0.977619390136729));
#42351=DIRECTION('',(-1.,0.,0.));
#42352=DIRECTION('',(0.,0.210381387077589,0.977619390136729));
#42353=DIRECTION('',(1.,0.,0.));
#42354=DIRECTION('center_axis',(0.561006631580424,0.253818593389699,0.787938881495552));
#42355=DIRECTION('ref_axis',(0.814616058663767,0.,-0.580000583592042));
#42356=DIRECTION('',(0.,0.951833920629441,-0.306614069375799));
#42357=DIRECTION('',(-0.705516335778296,-0.351310251680218,0.615489891886414));
#42358=DIRECTION('center_axis',(-0.561006631580398,0.809284384699505,-0.174156090919495));
#42359=DIRECTION('ref_axis',(-0.296477762129661,0.,0.955039756535082));
#42360=DIRECTION('',(0.705516335778309,0.357374756306019,-0.611988548508191));
#42361=DIRECTION('',(-0.705516335778307,-0.577478656052904,-0.410810298986385));
#42362=DIRECTION('center_axis',(-0.707106781186546,0.412732107142826,-0.574153470540278));
#42363=DIRECTION('ref_axis',(-0.630347388214435,0.,0.776313190774987));
#42364=DIRECTION('',(0.,0.81197562492164,0.583691343548209));
#42365=DIRECTION('',(0.,-0.81197562492164,-0.583691343548209));
#42366=DIRECTION('center_axis',(-0.561006631580422,0.253818593389699,0.787938881495553));
#42367=DIRECTION('ref_axis',(0.814616058663768,0.,0.580000583592041));
#42368=DIRECTION('',(0.705516335778308,0.644511483084941,0.294706036791919));
#42369=DIRECTION('',(-0.705516335778297,0.351310251680217,-0.615489891886412));
#42370=DIRECTION('',(0.,-0.951833920629441,0.306614069375799));
#42371=DIRECTION('center_axis',(-0.707106781186555,-0.290865437587464,0.644513225013298));
#42372=DIRECTION('ref_axis',(0.67363868643895,0.,0.739060836557321));
#42373=DIRECTION('',(0.,0.911479343942638,0.411345846661781));
#42374=DIRECTION('',(0.,-0.911479343942638,-0.411345846661781));
#42375=DIRECTION('center_axis',(0.,0.306614069375799,0.951833920629441));
#42376=DIRECTION('ref_axis',(1.,0.,0.));
#42377=DIRECTION('',(-1.,0.,0.));
#42378=DIRECTION('',(1.,0.,0.));
#42379=DIRECTION('center_axis',(-0.707106781186547,0.612372435695795,0.353553390593274));
#42380=DIRECTION('ref_axis',(0.447213595499958,0.,0.894427190999916));
#42381=DIRECTION('',(0.,0.5,-0.866025403784439));
#42382=DIRECTION('',(0.,-0.5,0.866025403784439));
#42383=DIRECTION('center_axis',(0.707106781186557,-0.290865437587463,0.644513225013297));
#42384=DIRECTION('ref_axis',(0.673638686438948,0.,-0.739060836557322));
#42385=DIRECTION('',(0.,-0.911479343942638,-0.411345846661781));
#42386=DIRECTION('center_axis',(0.,0.583691343548209,-0.81197562492164));
#42387=DIRECTION('ref_axis',(0.,0.81197562492164,0.583691343548209));
#42388=DIRECTION('center_axis',(0.,0.866025403784439,0.5));
#42389=DIRECTION('ref_axis',(0.,-0.5,0.866025403784439));
#42390=DIRECTION('center_axis',(0.561006631580409,0.8213835167442,-0.1029595927718));
#42391=DIRECTION('ref_axis',(-0.180511696561723,0.,-0.983572837874455));
#42392=DIRECTION('',(0.705516335778304,-0.409353153962201,0.578512484991598));
#42393=DIRECTION('',(0.,-0.124375678311979,-0.992235199256928));
#42394=DIRECTION('',(-0.705516335778303,0.539476698684503,0.459577622960939));
#42395=DIRECTION('center_axis',(0.561006631580412,0.184179338555415,0.807062284196263));
#42396=DIRECTION('ref_axis',(0.821109284001915,0.,-0.570771008133614));
#42397=DIRECTION('',(0.705516335778304,-0.616373598779652,-0.349757468365403));
#42398=DIRECTION('',(0.,0.97493508214826,-0.222489517947625));
#42399=DIRECTION('',(-0.705516335778314,-0.403616888790129,0.582529061106241));
#42400=DIRECTION('center_axis',(-0.561006631580389,0.821383516744213,-0.1029595927718));
#42401=DIRECTION('ref_axis',(-0.18051169656173,0.,0.983572837874453));
#42402=DIRECTION('',(0.,0.124375678311979,0.992235199256928));
#42403=DIRECTION('',(0.705516335778303,0.409353153962173,-0.578512484991619));
#42404=DIRECTION('',(-0.705516335778318,-0.539476698684487,-0.459577622960934));
#42405=DIRECTION('center_axis',(-0.707106781186546,0.461202309044001,-0.535996669889361));
#42406=DIRECTION('ref_axis',(-0.604079438549194,0.,0.79692410675176));
#42407=DIRECTION('',(0.,0.758013759944347,0.652238560447812));
#42408=DIRECTION('',(0.,-0.758013759944347,-0.652238560447812));
#42409=DIRECTION('center_axis',(-0.561006631580396,0.184179338555417,0.807062284196274));
#42410=DIRECTION('ref_axis',(0.821109284001927,0.,0.570771008133598));
#42411=DIRECTION('',(0.70551633577832,0.616373598779638,0.349757468365396));
#42412=DIRECTION('',(-0.705516335778313,0.403616888790152,-0.582529061106225));
#42413=DIRECTION('',(0.,-0.97493508214826,0.222489517947625));
#42414=DIRECTION('center_axis',(-0.707106781186539,-0.345931635619497,0.616710064355716));
#42415=DIRECTION('ref_axis',(0.657291420225588,0.,0.753636509796221));
#42416=DIRECTION('',(0.,0.872159737063827,0.489221210746995));
#42417=DIRECTION('',(0.,-0.872159737063827,-0.489221210746995));
#42418=DIRECTION('center_axis',(0.,0.222489517947625,0.97493508214826));
#42419=DIRECTION('ref_axis',(1.,0.,0.));
#42420=DIRECTION('',(-1.,0.,0.));
#42421=DIRECTION('',(1.,0.,0.));
#42422=DIRECTION('center_axis',(-0.707106781186532,0.579227965339582,0.405579787672648));
#42423=DIRECTION('ref_axis',(0.49754281216454,0.,0.867439421552538));
#42424=DIRECTION('',(0.,0.573576436351046,-0.819152044288992));
#42425=DIRECTION('',(0.,-0.573576436351046,0.819152044288992));
#42426=DIRECTION('center_axis',(0.,0.992235199256928,-0.124375678311979));
#42427=DIRECTION('ref_axis',(0.,0.124375678311979,0.992235199256928));
#42428=DIRECTION('',(-1.,0.,0.));
#42429=DIRECTION('',(1.,0.,0.));
#42430=DIRECTION('center_axis',(0.707106781186546,-0.345931635619494,0.61671006435571));
#42431=DIRECTION('ref_axis',(0.657291420225581,0.,-0.753636509796227));
#42432=DIRECTION('',(0.,0.872159737063827,0.489221210746995));
#42433=DIRECTION('',(0.,-0.872159737063827,-0.489221210746995));
#42434=DIRECTION('center_axis',(0.707106781186547,0.579227965339569,0.405579787672639));
#42435=DIRECTION('ref_axis',(0.497542812164523,0.,-0.867439421552547));
#42436=DIRECTION('',(0.,0.573576436351046,-0.819152044288992));
#42437=DIRECTION('',(0.,-0.573576436351046,0.819152044288992));
#42438=DIRECTION('center_axis',(0.707106781186547,0.461202309044,-0.53599666988936));
#42439=DIRECTION('ref_axis',(-0.604079438549193,0.,-0.796924106751761));
#42440=DIRECTION('',(0.,0.758013759944347,0.652238560447812));
#42441=DIRECTION('',(0.,-0.758013759944347,-0.652238560447812));
#42442=DIRECTION('center_axis',(1.,0.,0.));
#42443=DIRECTION('ref_axis',(0.,-0.819152044288992,-0.573576436351046));
#42444=DIRECTION('center_axis',(0.,0.652238560447812,-0.758013759944347));
#42445=DIRECTION('ref_axis',(0.,0.758013759944347,0.652238560447812));
#42446=DIRECTION('center_axis',(0.,0.819152044288992,0.573576436351046));
#42447=DIRECTION('ref_axis',(0.,-0.573576436351046,0.819152044288992));
#42448=DIRECTION('center_axis',(0.561006631580388,0.113138367744187,0.820043455596719));
#42449=DIRECTION('ref_axis',(0.825342782028786,0.,-0.564631997103409));
#42450=DIRECTION('',(0.705516335778318,-0.58354473921108,-0.402147034415285));
#42451=DIRECTION('',(0.,0.990616399010033,-0.136671686945011));
#42452=DIRECTION('',(-0.705516335778308,-0.452851757665877,0.545134832430359));
#42453=DIRECTION('center_axis',(0.,0.136671686945011,0.990616399010033));
#42454=DIRECTION('ref_axis',(1.,0.,0.));
#42455=DIRECTION('',(0.557191914001244,-0.822591759450536,0.113489947817864));
#42456=DIRECTION('',(1.,0.,0.));
#42457=DIRECTION('',(-1.,0.,0.));
#42458=DIRECTION('',(-0.557191914001257,-0.822591759450527,0.113489947817863));
#42459=DIRECTION('center_axis',(0.707106781186542,-0.398365085025226,0.584213367728652));
#42460=DIRECTION('ref_axis',(0.636934375125937,0.,-0.770918025332741));
#42461=DIRECTION('',(0.,0.826202467961513,0.563373306018581));
#42462=DIRECTION('',(0.,-0.826202467961513,-0.563373306018581));
#42463=DIRECTION('center_axis',(0.561006631580411,0.827231424261544,-0.0309795099544489));
#42464=DIRECTION('ref_axis',(-0.0551372865288087,0.,-0.998478782766184));
#42465=DIRECTION('',(0.705516335778302,-0.458216126942503,0.540633592148851));
#42466=DIRECTION('',(0.,-0.0374233955343756,-0.999299499382781));
#42467=DIRECTION('',(-0.705516335778315,0.497368997894199,0.504847283724158));
#42468=DIRECTION('center_axis',(0.,0.999299499382782,-0.0374233955343756));
#42469=DIRECTION('ref_axis',(0.,0.0374233955343756,0.999299499382781));
#42470=DIRECTION('',(0.557191914001262,0.0310757794924442,0.829802064892916));
#42471=DIRECTION('',(1.,0.,0.));
#42472=DIRECTION('',(-1.,0.,0.));
#42473=DIRECTION('',(-0.55719191400123,0.031075779492445,0.829802064892937));
#42474=DIRECTION('center_axis',(0.707106781186541,0.541675220419707,0.454519477672047));
#42475=DIRECTION('ref_axis',(0.540716203060943,0.,-0.841205080671388));
#42476=DIRECTION('',(0.,0.642787609686539,-0.766044443118978));
#42477=DIRECTION('',(0.,-0.642787609686539,0.766044443118978));
#42478=DIRECTION('center_axis',(0.707106781186551,0.50616248289178,-0.493760610936944));
#42479=DIRECTION('ref_axis',(-0.572517134274666,0.,-0.819892755768658));
#42480=DIRECTION('',(0.,0.698282952552655,0.715821848069997));
#42481=DIRECTION('',(0.,-0.698282952552655,-0.715821848069997));
#42482=DIRECTION('center_axis',(-0.70710678118654,-0.398365085025227,0.584213367728653));
#42483=DIRECTION('ref_axis',(0.636934375125939,0.,0.770918025332739));
#42484=DIRECTION('',(-0.595596683047433,-0.109786128885423,-0.795745937499683));
#42485=DIRECTION('',(0.,-0.826202467961513,-0.563373306018581));
#42486=DIRECTION('',(0.,0.826202467961513,0.563373306018581));
#42487=DIRECTION('center_axis',(0.,0.766044443118978,0.642787609686539));
#42488=DIRECTION('ref_axis',(0.,-0.642787609686539,0.766044443118978));
#42489=DIRECTION('',(0.,0.642787609686539,-0.766044443118978));
#42490=DIRECTION('center_axis',(-0.70710678118654,0.541675220419708,0.454519477672048));
#42491=DIRECTION('ref_axis',(0.540716203060945,0.,0.841205080671387));
#42492=DIRECTION('',(0.595596683047426,0.802720929891721,-0.0300616010331307));
#42493=DIRECTION('',(0.,-0.642787609686539,0.766044443118978));
#42494=DIRECTION('center_axis',(-0.707106781186549,0.506162482891781,-0.493760610936946));
#42495=DIRECTION('ref_axis',(-0.572517134274668,0.,0.819892755768657));
#42496=DIRECTION('',(0.,-0.698282952552655,-0.715821848069997));
#42497=DIRECTION('',(0.,0.698282952552655,0.715821848069997));
#42498=DIRECTION('center_axis',(0.,0.715821848069997,-0.698282952552655));
#42499=DIRECTION('ref_axis',(0.,0.698282952552655,0.715821848069997));
#42500=DIRECTION('center_axis',(0.,-0.563373306018581,0.826202467961513));
#42501=DIRECTION('ref_axis',(0.,-0.826202467961513,-0.563373306018581));
#42502=DIRECTION('center_axis',(0.561006631580404,0.826783601144275,0.0412363456396565));
#42503=DIRECTION('ref_axis',(0.0733064378127414,0.,-0.997309463594529));
#42504=DIRECTION('',(0.705516335778296,-0.503591798518335,0.498640151226349));
#42505=DIRECTION('',(0.,0.0498137018801831,-0.998758526924798));
#42506=DIRECTION('',(-0.705516335778313,0.451476018710252,0.546274751823186));
#42507=DIRECTION('center_axis',(0.561006631580394,0.041236345639636,0.826783601144283));
#42508=DIRECTION('ref_axis',(0.827487445286316,0.,-0.561484218739517));
#42509=DIRECTION('',(0.705516335778303,-0.546274751823203,-0.451476018710246));
#42510=DIRECTION('',(0.,0.998758526924799,-0.049813701880158));
#42511=DIRECTION('',(-0.705516335778304,-0.498640151226356,0.503591798518316));
#42512=DIRECTION('center_axis',(-0.561006631580402,0.826783601144276,0.0412363456396566));
#42513=DIRECTION('ref_axis',(0.0733064378127418,0.,0.997309463594529));
#42514=DIRECTION('',(0.,-0.0498137018801831,0.998758526924798));
#42515=DIRECTION('',(0.705516335778297,0.503591798518334,-0.498640151226348));
#42516=DIRECTION('',(-0.705516335778315,-0.451476018710251,-0.546274751823184));
#42517=DIRECTION('center_axis',(-0.70710678118655,0.547270454615492,-0.447766735594494));
#42518=DIRECTION('ref_axis',(-0.534994468449985,0.,0.844855560867015));
#42519=DIRECTION('',(0.,0.633237790257263,0.773957299203321));
#42520=DIRECTION('',(0.,-0.633237790257263,-0.773957299203321));
#42521=DIRECTION('center_axis',(-0.561006631580393,0.0412363456396361,0.826783601144284));
#42522=DIRECTION('ref_axis',(0.827487445286317,0.,0.561484218739515));
#42523=DIRECTION('',(0.705516335778305,0.546274751823202,0.451476018710245));
#42524=DIRECTION('',(-0.705516335778306,0.498640151226354,-0.503591798518315));
#42525=DIRECTION('',(0.,-0.998758526924799,0.049813701880158));
#42526=DIRECTION('center_axis',(-0.70710678118655,-0.447766735594494,0.547270454615492));
#42527=DIRECTION('ref_axis',(0.61205637248212,0.,0.790814135498366));
#42528=DIRECTION('',(0.,0.773957299203321,0.633237790257263));
#42529=DIRECTION('',(0.,-0.773957299203321,-0.633237790257263));
#42530=DIRECTION('center_axis',(0.,0.049813701880158,0.998758526924799));
#42531=DIRECTION('ref_axis',(1.,0.,0.));
#42532=DIRECTION('',(-1.,0.,0.));
#42533=DIRECTION('',(1.,0.,0.));
#42534=DIRECTION('center_axis',(-0.707106781186538,0.500000000000007,0.500000000000007));
#42535=DIRECTION('ref_axis',(0.577350269189637,0.,0.816496580927719));
#42536=DIRECTION('',(0.,0.707106781186547,-0.707106781186548));
#42537=DIRECTION('',(0.,-0.707106781186547,0.707106781186548));
#42538=DIRECTION('center_axis',(0.,0.998758526924798,0.0498137018801831));
#42539=DIRECTION('ref_axis',(0.,-0.0498137018801831,0.998758526924798));
#42540=DIRECTION('',(-1.,0.,0.));
#42541=DIRECTION('',(1.,0.,0.));
#42542=DIRECTION('center_axis',(0.707106781186551,-0.447766735594493,0.547270454615491));
#42543=DIRECTION('ref_axis',(0.612056372482119,0.,-0.790814135498367));
#42544=DIRECTION('',(0.,0.773957299203321,0.633237790257263));
#42545=DIRECTION('',(0.,-0.773957299203321,-0.633237790257263));
#42546=DIRECTION('center_axis',(0.707106781186539,0.500000000000006,0.500000000000006));
#42547=DIRECTION('ref_axis',(0.577350269189635,0.,-0.81649658092772));
#42548=DIRECTION('',(0.,0.707106781186547,-0.707106781186548));
#42549=DIRECTION('',(0.,-0.707106781186547,0.707106781186548));
#42550=DIRECTION('center_axis',(0.707106781186551,0.547270454615491,-0.447766735594493));
#42551=DIRECTION('ref_axis',(-0.534994468449984,0.,-0.844855560867016));
#42552=DIRECTION('',(0.,0.633237790257263,0.773957299203321));
#42553=DIRECTION('',(0.,-0.633237790257263,-0.773957299203321));
#42554=DIRECTION('center_axis',(1.,0.,0.));
#42555=DIRECTION('ref_axis',(0.,-0.707106781186548,-0.707106781186547));
#42556=DIRECTION('center_axis',(0.,0.773957299203321,-0.633237790257263));
#42557=DIRECTION('ref_axis',(0.,0.633237790257263,0.773957299203321));
#42558=DIRECTION('center_axis',(0.,0.707106781186548,0.707106781186547));
#42559=DIRECTION('ref_axis',(0.,-0.707106781186547,0.707106781186548));
#42560=DIRECTION('center_axis',(0.561006631580392,0.820043455596711,0.113138367744223));
#42561=DIRECTION('ref_axis',(0.197690230426254,0.,-0.98026454225072));
#42562=DIRECTION('',(0.705516335778306,-0.545134832430383,0.452851757665851));
#42563=DIRECTION('',(0.,0.136671686945054,-0.990616399010027));
#42564=DIRECTION('',(-0.705516335778304,0.402147034415252,0.583544739211119));
#42565=DIRECTION('center_axis',(0.561006631580441,-0.0309795099544276,0.827231424261525));
#42566=DIRECTION('ref_axis',(0.827628669643362,0.,-0.561276032968057));
#42567=DIRECTION('',(0.705516335778297,-0.50484728372417,-0.497368997894212));
#42568=DIRECTION('',(0.,0.999299499382783,0.0374233955343508));
#42569=DIRECTION('',(-0.705516335778286,-0.540633592148838,0.458216126942542));
#42570=DIRECTION('center_axis',(-0.561006631580388,0.820043455596714,0.113138367744223));
#42571=DIRECTION('ref_axis',(0.197690230426256,0.,0.98026454225072));
#42572=DIRECTION('',(0.,-0.136671686945054,0.990616399010027));
#42573=DIRECTION('',(0.7055163357783,0.545134832430375,-0.45285175766587));
#42574=DIRECTION('',(-0.705516335778316,-0.402147034415257,-0.583544739211101));
#42575=DIRECTION('center_axis',(-0.707106781186557,0.584213367728639,-0.398365085025217));
#42576=DIRECTION('ref_axis',(-0.490839120629124,0.,0.871250226777605));
#42577=DIRECTION('',(0.,0.563373306018581,0.826202467961512));
#42578=DIRECTION('',(0.,-0.563373306018581,-0.826202467961512));
#42579=DIRECTION('center_axis',(-0.561006631580419,-0.0309795099544281,
0.82723142426154));
#42580=DIRECTION('ref_axis',(0.827628669643377,0.,0.561276032968035));
#42581=DIRECTION('',(0.705516335778307,0.504847283724175,0.497368997894192));
#42582=DIRECTION('',(-0.705516335778296,0.540633592148843,-0.458216126942521));
#42583=DIRECTION('',(0.,-0.999299499382783,-0.0374233955343508));
#42584=DIRECTION('center_axis',(-0.707106781186558,-0.493760610936939,0.506162482891775));
#42585=DIRECTION('ref_axis',(0.582064997116532,0.,0.813142262541882));
#42586=DIRECTION('',(0.,0.715821848069998,0.698282952552655));
#42587=DIRECTION('',(0.,-0.715821848069998,-0.698282952552655));
#42588=DIRECTION('center_axis',(0.,-0.0374233955343508,0.999299499382783));
#42589=DIRECTION('ref_axis',(1.,0.,0.));
#42590=DIRECTION('',(-1.,0.,0.));
#42591=DIRECTION('',(1.,0.,0.));
#42592=DIRECTION('center_axis',(-0.707106781186548,0.454519477672044,0.541675220419701));
#42593=DIRECTION('ref_axis',(0.608120402411342,0.,0.793844806099446));
#42594=DIRECTION('',(0.,0.766044443118978,-0.64278760968654));
#42595=DIRECTION('',(0.,-0.766044443118978,0.64278760968654));
#42596=DIRECTION('center_axis',(0.,0.990616399010027,0.136671686945054));
#42597=DIRECTION('ref_axis',(0.,-0.136671686945054,0.990616399010027));
#42598=DIRECTION('',(-1.,0.,0.));
#42599=DIRECTION('',(1.,0.,0.));
#42600=DIRECTION('center_axis',(0.70710678118656,-0.493760610936938,0.506162482891773));
#42601=DIRECTION('ref_axis',(0.58206499711653,0.,-0.813142262541883));
#42602=DIRECTION('',(0.,0.715821848069998,0.698282952552655));
#42603=DIRECTION('',(0.,-0.715821848069998,-0.698282952552655));
#42604=DIRECTION('center_axis',(0.707106781186559,0.454519477672036,0.541675220419693));
#42605=DIRECTION('ref_axis',(0.60812040241133,0.,-0.793844806099455));
#42606=DIRECTION('',(0.,0.766044443118978,-0.64278760968654));
#42607=DIRECTION('',(0.,-0.766044443118978,0.64278760968654));
#42608=DIRECTION('center_axis',(0.707106781186542,0.584213367728652,-0.398365085025226));
#42609=DIRECTION('ref_axis',(-0.490839120629141,0.,-0.871250226777595));
#42610=DIRECTION('',(0.,0.563373306018581,0.826202467961512));
#42611=DIRECTION('',(0.,-0.563373306018581,-0.826202467961512));
#42612=DIRECTION('center_axis',(1.,0.,0.));
#42613=DIRECTION('ref_axis',(0.,-0.64278760968654,-0.766044443118978));
#42614=DIRECTION('center_axis',(0.,0.826202467961512,-0.563373306018581));
#42615=DIRECTION('ref_axis',(0.,0.563373306018581,0.826202467961512));
#42616=DIRECTION('center_axis',(0.,0.64278760968654,0.766044443118978));
#42617=DIRECTION('ref_axis',(0.,-0.766044443118978,0.64278760968654));
#42618=DIRECTION('center_axis',(0.707106781186552,0.616710064355705,-0.345931635619491));
#42619=DIRECTION('ref_axis',(-0.439451044888509,0.,-0.898266541259552));
#42620=DIRECTION('',(0.595596683047423,-0.783149392358838,-0.178722187740891));
#42621=DIRECTION('',(0.,-0.489221210746995,-0.872159737063827));
#42622=DIRECTION('',(0.,0.489221210746995,0.872159737063827));
#42623=DIRECTION('',(0.557191914001246,-0.184751680075907,0.809570248762118));
#42624=DIRECTION('center_axis',(1.,0.,0.));
#42625=DIRECTION('ref_axis',(0.,-0.573576436351046,-0.819152044288992));
#42626=DIRECTION('',(0.,0.819152044288992,-0.573576436351046));
#42627=DIRECTION('',(0.,0.652238560447812,0.758013759944346));
#42628=DIRECTION('center_axis',(0.707106781186547,0.405579787672639,0.579227965339569));
#42629=DIRECTION('ref_axis',(0.633687274224642,0.,-0.773589321594955));
#42630=DIRECTION('',(0.557191914001238,0.184751680075908,-0.809570248762123));
#42631=DIRECTION('',(0.,-0.819152044288992,0.573576436351046));
#42632=DIRECTION('',(0.705516335778303,-0.459577622960939,-0.539476698684503));
#42633=DIRECTION('center_axis',(0.,0.974935082148257,0.222489517947637));
#42634=DIRECTION('ref_axis',(0.,-0.222489517947637,0.974935082148257));
#42635=DIRECTION('',(-1.,0.,0.));
#42636=DIRECTION('',(0.,-0.222489517947637,0.974935082148257));
#42637=DIRECTION('',(1.,0.,0.));
#42638=DIRECTION('center_axis',(0.561006631580418,-0.10295959277178,0.821383516744196));
#42639=DIRECTION('ref_axis',(0.825772049781954,0.,-0.564004008672731));
#42640=DIRECTION('',(0.,0.992235199256931,0.124375678311957));
#42641=DIRECTION('',(-0.705516335778302,-0.578512484991583,0.409353153962224));
#42642=DIRECTION('center_axis',(-0.561006631580406,0.807062284196265,0.184179338555426));
#42643=DIRECTION('ref_axis',(0.311921838389608,0.,0.950107765853773));
#42644=DIRECTION('',(0.705516335778296,0.582529061106236,-0.403616888790167));
#42645=DIRECTION('',(-0.705516335778309,-0.349757468365391,-0.616373598779654));
#42646=DIRECTION('center_axis',(-0.70710678118655,0.616710064355706,-0.345931635619492));
#42647=DIRECTION('ref_axis',(-0.43945104488851,0.,0.898266541259551));
#42648=DIRECTION('',(0.,0.489221210746995,0.872159737063827));
#42649=DIRECTION('',(0.,-0.489221210746995,-0.872159737063827));
#42650=DIRECTION('center_axis',(-0.561006631580395,-0.102959592771782,0.821383516744211));
#42651=DIRECTION('ref_axis',(0.82577204978197,0.,0.564004008672708));
#42652=DIRECTION('',(0.70551633577831,0.459577622960954,0.539476698684481));
#42653=DIRECTION('',(-0.705516335778316,0.57851248499158,-0.409353153962206));
#42654=DIRECTION('',(0.,-0.992235199256931,-0.124375678311957));
#42655=DIRECTION('center_axis',(-0.707106781186541,-0.535996669889364,0.461202309044004));
#42656=DIRECTION('ref_axis',(0.546305769586294,0.,0.837585820150226));
#42657=DIRECTION('',(0.,0.652238560447812,0.758013759944346));
#42658=DIRECTION('',(0.,-0.652238560447812,-0.758013759944346));
#42659=DIRECTION('center_axis',(0.,-0.124375678311957,0.992235199256931));
#42660=DIRECTION('ref_axis',(1.,0.,0.));
#42661=DIRECTION('',(-1.,0.,0.));
#42662=DIRECTION('',(1.,0.,0.));
#42663=DIRECTION('center_axis',(-0.707106781186546,0.40557978767264,0.579227965339571));
#42664=DIRECTION('ref_axis',(0.633687274224644,0.,0.773589321594954));
#42665=DIRECTION('',(0.,0.819152044288992,-0.573576436351046));
#42666=DIRECTION('',(0.,-0.819152044288992,0.573576436351046));
#42667=DIRECTION('center_axis',(0.707106781186552,-0.535996669889356,0.461202309043997));
#42668=DIRECTION('ref_axis',(0.546305769586282,0.,-0.837585820150234));
#42669=DIRECTION('',(0.,-0.652238560447812,-0.758013759944346));
#42670=DIRECTION('center_axis',(0.,0.872159737063827,-0.489221210746995));
#42671=DIRECTION('ref_axis',(0.,0.489221210746995,0.872159737063827));
#42672=DIRECTION('center_axis',(0.,0.573576436351046,0.819152044288992));
#42673=DIRECTION('ref_axis',(0.,-0.819152044288992,0.573576436351046));
#42674=DIRECTION('center_axis',(0.561006631580402,0.787938881495568,0.253818593389698));
#42675=DIRECTION('ref_axis',(0.412208150462332,0.,-0.911089699586393));
#42676=DIRECTION('',(0.7055163357783,-0.615489891886393,0.351310251680245));
#42677=DIRECTION('',(0.,0.306614069375792,-0.951833920629443));
#42678=DIRECTION('',(-0.705516335778309,0.294706036791908,0.644511483084945));
#42679=DIRECTION('center_axis',(0.561006631580397,-0.174156090919455,0.809284384699514));
#42680=DIRECTION('ref_axis',(0.821843752318944,0.,-0.569712951208166));
#42681=DIRECTION('',(0.705516335778309,-0.410810298986413,-0.577478656052882));
#42682=DIRECTION('',(0.,0.97761939013674,0.210381387077539));
#42683=DIRECTION('',(-0.705516335778306,-0.611988548508179,0.357374756306044));
#42684=DIRECTION('center_axis',(-0.561006631580411,0.787938881495565,0.253818593389687));
#42685=DIRECTION('ref_axis',(0.412208150462312,0.,0.911089699586402));
#42686=DIRECTION('',(0.,-0.306614069375792,0.951833920629443));
#42687=DIRECTION('',(0.705516335778308,0.615489891886397,-0.351310251680223));
#42688=DIRECTION('',(-0.705516335778296,-0.294706036791914,-0.644511483084956));
#42689=DIRECTION('center_axis',(-0.707106781186549,0.644513225013303,-0.290865437587467));
#42690=DIRECTION('ref_axis',(-0.380418570543387,0.,0.924814419862561));
#42691=DIRECTION('',(0.,0.411345846661781,0.911479343942638));
#42692=DIRECTION('',(0.,-0.411345846661781,-0.911479343942638));
#42693=DIRECTION('center_axis',(-0.561006631580409,-0.174156090919453,0.809284384699506));
#42694=DIRECTION('ref_axis',(0.821843752318936,0.,0.569712951208178));
#42695=DIRECTION('',(0.705516335778289,0.410810298986437,0.577478656052889));
#42696=DIRECTION('',(-0.705516335778318,0.611988548508149,-0.357374756306074));
#42697=DIRECTION('',(0.,-0.97761939013674,-0.210381387077539));
#42698=DIRECTION('center_axis',(-0.707106781186536,-0.574153470540286,0.412732107142832));
#42699=DIRECTION('ref_axis',(0.504101701135483,0.,0.863644298836224));
#42700=DIRECTION('',(0.,0.583691343548209,0.811975624921639));
#42701=DIRECTION('',(0.,-0.583691343548209,-0.811975624921639));
#42702=DIRECTION('center_axis',(0.,-0.210381387077539,0.97761939013674));
#42703=DIRECTION('ref_axis',(1.,0.,0.));
#42704=DIRECTION('',(-1.,0.,0.));
#42705=DIRECTION('',(1.,0.,0.));
#42706=DIRECTION('center_axis',(-0.707106781186558,0.353553390593269,0.612372435695785));
#42707=DIRECTION('ref_axis',(0.654653670707966,0.,0.755928946018464));
#42708=DIRECTION('',(0.,0.866025403784438,-0.5));
#42709=DIRECTION('',(0.,-0.866025403784438,0.5));
#42710=DIRECTION('center_axis',(0.,0.951833920629443,0.306614069375792));
#42711=DIRECTION('ref_axis',(0.,-0.306614069375792,0.951833920629443));
#42712=DIRECTION('',(-1.,0.,0.));
#42713=DIRECTION('',(1.,0.,0.));
#42714=DIRECTION('center_axis',(0.707106781186547,-0.574153470540276,0.412732107142825));
#42715=DIRECTION('ref_axis',(0.504101701135471,0.,-0.863644298836231));
#42716=DIRECTION('',(0.,0.583691343548209,0.811975624921639));
#42717=DIRECTION('',(0.,-0.583691343548209,-0.811975624921639));
#42718=DIRECTION('center_axis',(0.707106781186545,0.353553390593275,0.612372435695796));
#42719=DIRECTION('ref_axis',(0.654653670707979,0.,-0.755928946018453));
#42720=DIRECTION('',(0.,0.866025403784438,-0.5));
#42721=DIRECTION('',(0.,-0.866025403784438,0.5));
#42722=DIRECTION('center_axis',(0.707106781186551,0.644513225013302,-0.290865437587466));
#42723=DIRECTION('ref_axis',(-0.380418570543386,0.,-0.924814419862562));
#42724=DIRECTION('',(0.,0.411345846661781,0.911479343942638));
#42725=DIRECTION('',(0.,-0.411345846661781,-0.911479343942638));
#42726=DIRECTION('center_axis',(1.,0.,0.));
#42727=DIRECTION('ref_axis',(0.,-0.5,-0.866025403784438));
#42728=DIRECTION('center_axis',(0.,0.911479343942638,-0.411345846661781));
#42729=DIRECTION('ref_axis',(0.,0.411345846661781,0.911479343942638));
#42730=DIRECTION('center_axis',(0.,0.5,0.866025403784438));
#42731=DIRECTION('ref_axis',(0.,-0.866025403784438,0.5));
#42732=DIRECTION('center_axis',(0.561006631580396,-0.244027156056938,0.791026109827976));
#42733=DIRECTION('ref_axis',(0.815685591418261,0.,-0.578495476173014));
#42734=DIRECTION('',(0.705516335778303,-0.358916460582535,-0.611085652157587));
#42735=DIRECTION('',(0.,0.955563307154871,0.294785966455742));
#42736=DIRECTION('',(-0.705516335778307,-0.640807009641837,0.302676520965598));
#42737=DIRECTION('center_axis',(0.,-0.294785966455742,0.955563307154871));
#42738=DIRECTION('ref_axis',(1.,0.,0.));
#42739=DIRECTION('',(0.557191914001242,-0.793484241614032,-0.244785476043487));
#42740=DIRECTION('',(1.,0.,0.));
#42741=DIRECTION('',(-1.,0.,0.));
#42742=DIRECTION('',(-0.557191914001242,-0.793484241614032,-0.244785476043487));
#42743=DIRECTION('center_axis',(0.707106781186547,-0.607940616597037,0.361120764691833));
#42744=DIRECTION('ref_axis',(0.454822071931221,0.,-0.890582327965355));
#42745=DIRECTION('',(0.,0.510701883081734,0.859757865108992));
#42746=DIRECTION('',(0.,-0.510701883081734,-0.859757865108992));
#42747=DIRECTION('center_axis',(0.561006631580424,0.762818788136169,0.321526135468413));
#42748=DIRECTION('ref_axis',(0.497247150959849,0.,-0.867608938901803));
#42749=DIRECTION('',(0.705516335778299,-0.643766472946357,0.296329931428078));
#42750=DIRECTION('',(0.,0.388405102597364,-0.921488728241605));
#42751=DIRECTION('',(-0.705516335778301,0.237411714330098,0.667744245837284));
#42752=DIRECTION('center_axis',(0.,0.921488728241605,0.388405102597364));
#42753=DIRECTION('ref_axis',(0.,-0.388405102597364,0.921488728241605));
#42754=DIRECTION('',(0.557191914001242,-0.322525285311673,0.765189265022881));
#42755=DIRECTION('',(1.,0.,0.));
#42756=DIRECTION('',(-1.,0.,0.));
#42757=DIRECTION('',(-0.557191914001238,-0.322525285311674,0.765189265022883));
#42758=DIRECTION('center_axis',(0.707106781186551,0.298836238730119,0.640856382055785));
#42759=DIRECTION('ref_axis',(0.671542934237814,0.,-0.740965645273293));
#42760=DIRECTION('',(0.,0.90630778703665,-0.4226182617407));
#42761=DIRECTION('',(0.,-0.90630778703665,0.4226182617407));
#42762=DIRECTION('center_axis',(0.707106781186551,0.667411250860821,-0.233585577946046));
#42763=DIRECTION('ref_axis',(-0.313668483594039,0.,-0.949532559947165));
#42764=DIRECTION('',(0.,0.330339892306058,0.943862042647771));
#42765=DIRECTION('',(0.,-0.330339892306058,-0.943862042647771));
#42766=DIRECTION('center_axis',(-0.707106781186546,-0.607940616597038,0.361120764691834));
#42767=DIRECTION('ref_axis',(0.454822071931223,0.,0.890582327965354));
#42768=DIRECTION('',(-0.595596683047429,0.236796741375871,-0.767588362611542));
#42769=DIRECTION('',(0.,-0.510701883081734,-0.859757865108992));
#42770=DIRECTION('',(0.,0.510701883081734,0.859757865108992));
#42771=DIRECTION('center_axis',(0.,0.4226182617407,0.90630778703665));
#42772=DIRECTION('ref_axis',(0.,-0.90630778703665,0.4226182617407));
#42773=DIRECTION('',(0.,0.90630778703665,-0.4226182617407));
#42774=DIRECTION('center_axis',(-0.70710678118655,0.298836238730119,0.640856382055786));
#42775=DIRECTION('ref_axis',(0.671542934237816,0.,0.740965645273291));
#42776=DIRECTION('',(0.595596683047418,0.740216811151934,0.311999460946611));
#42777=DIRECTION('',(0.,-0.90630778703665,0.4226182617407));
#42778=DIRECTION('center_axis',(-0.70710678118655,0.667411250860823,-0.233585577946047));
#42779=DIRECTION('ref_axis',(-0.31366848359404,0.,0.949532559947164));
#42780=DIRECTION('',(0.,-0.330339892306058,-0.943862042647771));
#42781=DIRECTION('',(0.,0.330339892306058,0.943862042647771));
#42782=DIRECTION('center_axis',(0.,0.943862042647771,-0.330339892306058));
#42783=DIRECTION('ref_axis',(0.,0.330339892306058,0.943862042647771));
#42784=DIRECTION('center_axis',(0.,-0.859757865108992,0.510701883081734));
#42785=DIRECTION('ref_axis',(0.,-0.510701883081734,-0.859757865108992));
#42786=DIRECTION('center_axis',(0.561006631580406,0.731893183196498,0.386786669513448));
#42787=DIRECTION('ref_axis',(0.567619122871711,0.,-0.823291279773052));
#42788=DIRECTION('',(0.705516335778304,-0.667143602430351,0.239094361468878));
#42789=DIRECTION('',(0.,0.467240138462772,-0.884130450221736));
#42790=DIRECTION('',(-0.705516335778305,0.178310545369065,0.685895071683811));
#42791=DIRECTION('center_axis',(0.561006631580414,-0.312041027189174,0.766747648626015));
#42792=DIRECTION('ref_axis',(0.80704448738357,0.,-0.59049063953952));
#42793=DIRECTION('',(0.705516335778303,-0.304291051193915,-0.64004191746577));
#42794=DIRECTION('',(0.,0.926234810420659,0.376947046632555));
#42795=DIRECTION('',(-0.70551633577831,-0.664748542502243,0.245674734539575));
#42796=DIRECTION('center_axis',(-0.561006631580404,0.731893183196499,0.386786669513448));
#42797=DIRECTION('ref_axis',(0.567619122871712,0.,0.823291279773051));
#42798=DIRECTION('',(0.,-0.467240138462772,0.884130450221736));
#42799=DIRECTION('',(0.705516335778315,0.667143602430346,-0.239094361468855));
#42800=DIRECTION('',(-0.705516335778296,-0.178310545369049,-0.685895071683825));
#42801=DIRECTION('center_axis',(-0.707106781186539,0.685229874095371,-0.174527991013632));
#42802=DIRECTION('ref_axis',(-0.239628661022764,0.,0.97086461714105));
#42803=DIRECTION('',(0.,0.246819851905205,0.96906138128887));
#42804=DIRECTION('',(0.,-0.246819851905205,-0.96906138128887));
#42805=DIRECTION('center_axis',(-0.561006631580427,-0.312041027189171,0.766747648626007));
#42806=DIRECTION('ref_axis',(0.80704448738356,0.,0.590490639539533));
#42807=DIRECTION('',(0.705516335778291,0.304291051193921,0.640041917465781));
#42808=DIRECTION('',(-0.705516335778313,0.664748542502231,-0.2456747345396));
#42809=DIRECTION('',(0.,-0.926234810420659,-0.376947046632555));
#42810=DIRECTION('center_axis',(-0.707106781186541,-0.637100967476919,0.30676107517086));
#42811=DIRECTION('ref_axis',(0.397987666358449,0.,0.917390765937044));
#42812=DIRECTION('',(0.,0.433825672914779,0.900996828806872));
#42813=DIRECTION('',(0.,-0.433825672914779,-0.900996828806872));
#42814=DIRECTION('center_axis',(0.,-0.376947046632555,0.926234810420659));
#42815=DIRECTION('ref_axis',(1.,0.,0.));
#42816=DIRECTION('',(-1.,0.,0.));
#42817=DIRECTION('',(1.,0.,0.));
#42818=DIRECTION('center_axis',(-0.707106781186561,0.241844762647971,0.664463024388662));
#42819=DIRECTION('ref_axis',(0.684791078771722,0.,0.728739444818696));
#42820=DIRECTION('',(0.,0.939692620785908,-0.342020143325669));
#42821=DIRECTION('',(0.,-0.939692620785908,0.342020143325669));
#42822=DIRECTION('center_axis',(0.,0.884130450221736,0.467240138462772));
#42823=DIRECTION('ref_axis',(0.,-0.467240138462772,0.884130450221736));
#42824=DIRECTION('',(-1.,0.,0.));
#42825=DIRECTION('',(1.,0.,0.));
#42826=DIRECTION('center_axis',(0.707106781186543,-0.637100967476918,0.306761075170859));
#42827=DIRECTION('ref_axis',(0.397987666358448,0.,-0.917390765937044));
#42828=DIRECTION('',(0.,0.433825672914779,0.900996828806872));
#42829=DIRECTION('',(0.,-0.433825672914779,-0.900996828806872));
#42830=DIRECTION('center_axis',(0.707106781186551,0.241844762647975,0.664463024388671));
#42831=DIRECTION('ref_axis',(0.684791078771732,0.,-0.728739444818686));
#42832=DIRECTION('',(0.,0.939692620785908,-0.342020143325669));
#42833=DIRECTION('',(0.,-0.939692620785908,0.342020143325669));
#42834=DIRECTION('center_axis',(0.707106781186549,0.685229874095361,-0.174527991013629));
#42835=DIRECTION('ref_axis',(-0.239628661022757,0.,-0.970864617141052));
#42836=DIRECTION('',(0.,0.246819851905205,0.96906138128887));
#42837=DIRECTION('',(0.,-0.246819851905205,-0.96906138128887));
#42838=DIRECTION('center_axis',(1.,0.,0.));
#42839=DIRECTION('ref_axis',(0.,-0.342020143325669,-0.939692620785908));
#42840=DIRECTION('center_axis',(0.,0.96906138128887,-0.246819851905205));
#42841=DIRECTION('ref_axis',(0.,0.246819851905205,0.96906138128887));
#42842=DIRECTION('center_axis',(0.,0.342020143325669,0.939692620785908));
#42843=DIRECTION('ref_axis',(0.,-0.939692620785908,0.342020143325669));
#42844=DIRECTION('center_axis',(0.561006631580403,0.695397429203503,0.449103523455304));
#42845=DIRECTION('ref_axis',(0.62494805391789,0.,-0.780666337114802));
#42846=DIRECTION('',(0.705516335778305,-0.685443366267539,0.18003913904976));
#42847=DIRECTION('',(0.,0.542519194747167,-0.840043405623117));
#42848=DIRECTION('',(-0.705516335778305,0.117852325490942,0.698825821880052));
#42849=DIRECTION('center_axis',(0.561006631580396,-0.37768007768899,0.736633774843142));
#42850=DIRECTION('ref_axis',(0.795555689966284,0.,-0.605880470193808));
#42851=DIRECTION('',(0.705516335778306,-0.2473498031698,-0.664127077314135));
#42852=DIRECTION('',(0.,0.889857107503274,0.456239332177649));
#42853=DIRECTION('',(-0.705516335778303,-0.683630937568099,0.186803215041171));
#42854=DIRECTION('center_axis',(-0.561006631580402,0.695397429203504,0.449103523455304));
#42855=DIRECTION('ref_axis',(0.624948053917891,0.,0.780666337114801));
#42856=DIRECTION('',(0.,-0.542519194747167,0.840043405623117));
#42857=DIRECTION('',(0.705516335778306,0.685443366267538,-0.180039139049759));
#42858=DIRECTION('',(-0.705516335778307,-0.117852325490942,-0.698825821880051));
#42859=DIRECTION('center_axis',(-0.707106781186546,0.697833484234925,-0.114142140686716));
#42860=DIRECTION('ref_axis',(-0.159358523666364,0.,0.987220776186805));
#42861=DIRECTION('',(0.,0.161421363397451,0.986885577683101));
#42862=DIRECTION('',(0.,-0.161421363397451,-0.986885577683101));
#42863=DIRECTION('center_axis',(-0.561006631580394,-0.37768007768899,0.736633774843143));
#42864=DIRECTION('ref_axis',(0.795555689966285,0.,0.605880470193806));
#42865=DIRECTION('',(0.705516335778307,0.247349803169799,0.664127077314133));
#42866=DIRECTION('',(-0.705516335778305,0.683630937568098,-0.18680321504117));
#42867=DIRECTION('',(0.,-0.889857107503274,-0.456239332177649));
#42868=DIRECTION('center_axis',(-0.707106781186544,-0.661412595302213,0.25006674864043));
#42869=DIRECTION('ref_axis',(0.333412439312664,0.,0.942781069661233));
#42870=DIRECTION('',(0.,0.353647787425838,0.935378662600772));
#42871=DIRECTION('',(0.,-0.353647787425838,-0.935378662600772));
#42872=DIRECTION('center_axis',(0.,-0.456239332177649,0.889857107503274));
#42873=DIRECTION('ref_axis',(1.,0.,0.));
#42874=DIRECTION('',(-1.,0.,0.));
#42875=DIRECTION('',(1.,0.,0.));
#42876=DIRECTION('center_axis',(-0.707106781186551,0.183012701892218,0.683012701892216));
#42877=DIRECTION('ref_axis',(0.694746590606862,0.,0.719254596676407));
#42878=DIRECTION('',(0.,0.965925826289068,-0.258819045102521));
#42879=DIRECTION('',(0.,-0.965925826289068,0.258819045102521));
#42880=DIRECTION('center_axis',(0.,0.840043405623117,0.542519194747167));
#42881=DIRECTION('ref_axis',(1.,0.,0.));
#42882=DIRECTION('',(-1.,0.,0.));
#42883=DIRECTION('',(1.,0.,0.));
#42884=DIRECTION('center_axis',(0.707106781186545,-0.661412595302212,0.25006674864043));
#42885=DIRECTION('ref_axis',(0.333412439312663,0.,-0.942781069661234));
#42886=DIRECTION('',(0.,0.353647787425838,0.935378662600772));
#42887=DIRECTION('',(0.,-0.353647787425838,-0.935378662600772));
#42888=DIRECTION('center_axis',(0.707106781186552,0.183012701892218,0.683012701892215));
#42889=DIRECTION('ref_axis',(0.694746590606861,0.,-0.719254596676408));
#42890=DIRECTION('',(0.,0.965925826289068,-0.258819045102521));
#42891=DIRECTION('',(0.,-0.965925826289068,0.258819045102521));
#42892=DIRECTION('center_axis',(0.707106781186548,0.697833484234924,-0.114142140686716));
#42893=DIRECTION('ref_axis',(-0.159358523666364,0.,-0.987220776186805));
#42894=DIRECTION('',(0.,0.161421363397451,0.986885577683101));
#42895=DIRECTION('',(0.,-0.161421363397451,-0.986885577683101));
#42896=DIRECTION('center_axis',(1.,0.,0.));
#42897=DIRECTION('ref_axis',(0.,-0.258819045102521,-0.965925826289068));
#42898=DIRECTION('center_axis',(0.,0.986885577683101,-0.161421363397451));
#42899=DIRECTION('ref_axis',(0.,0.161421363397451,0.986885577683101));
#42900=DIRECTION('center_axis',(0.,0.258819045102521,0.965925826289068));
#42901=DIRECTION('ref_axis',(0.,-0.965925826289068,0.258819045102521));
#42902=DIRECTION('center_axis',(-1.,0.,-9.34622984744497E-15));
#42903=DIRECTION('ref_axis',(0.,-1.,-3.06609014182674E-17));
#42904=DIRECTION('center_axis',(-1.,0.,0.));
#42905=DIRECTION('ref_axis',(0.,-1.,-6.12323399573676E-17));
#42906=DIRECTION('center_axis',(-1.,0.,0.));
#42907=DIRECTION('ref_axis',(0.,-1.,-6.12323399573676E-17));
#42908=DIRECTION('',(0.913500063388735,-0.406838584931147,8.5751308774215E-15));
#42909=DIRECTION('center_axis',(1.,0.,0.));
#42910=DIRECTION('ref_axis',(0.,-1.,0.));
#42911=DIRECTION('center_axis',(1.,0.,0.));
#42912=DIRECTION('ref_axis',(0.,-1.,0.));
#42913=DIRECTION('center_axis',(-1.,0.,0.));
#42914=DIRECTION('ref_axis',(0.,1.,0.));
#42915=DIRECTION('',(-0.668964731622448,-0.743294146247168,-9.10272797026559E-17));
#42916=DIRECTION('center_axis',(1.,0.,0.));
#42917=DIRECTION('ref_axis',(0.,-1.,-6.12323399573677E-17));
#42918=DIRECTION('center_axis',(1.,0.,0.));
#42919=DIRECTION('ref_axis',(0.,-1.,-6.12323399573677E-17));
#42920=DIRECTION('center_axis',(1.,0.,0.));
#42921=DIRECTION('ref_axis',(0.,1.,0.));
#42922=DIRECTION('center_axis',(1.,0.,0.));
#42923=DIRECTION('ref_axis',(0.,0.,-1.));
#42924=DIRECTION('',(-1.,0.,0.));
#42925=DIRECTION('center_axis',(0.561006631580394,0.653609280881836,0.508002428407532));
#42926=DIRECTION('ref_axis',(0.671222048820192,0.,-0.741256339721708));
#42927=DIRECTION('',(0.705516335778306,-0.698526492205406,0.119613710071895));
#42928=DIRECTION('',(0.,0.613669352377473,-0.789563123475643));
#42929=DIRECTION('',(-0.70551633577831,0.0564971782546651,0.706438085609211));
#42930=DIRECTION('center_axis',(0.56100663158039,-0.44044475474812,0.700913673242072));
#42931=DIRECTION('ref_axis',(0.780718990354277,0.,-0.624882275392892));
#42932=DIRECTION('',(0.70551633577831,-0.188526073789633,-0.683157829093258));
#42933=DIRECTION('',(0.,0.846707054687377,0.532059360920026));
#42934=DIRECTION('',(-0.705516335778307,-0.697310488411391,0.126510010281474));
#42935=DIRECTION('center_axis',(-0.561006631580392,0.653609280881837,0.508002428407533));
#42936=DIRECTION('ref_axis',(0.671222048820193,0.,0.741256339721707));
#42937=DIRECTION('',(0.,-0.613669352377473,0.789563123475643));
#42938=DIRECTION('',(0.705516335778308,0.698526492205404,-0.119613710071895));
#42939=DIRECTION('',(-0.705516335778312,-0.056497178254665,-0.70643808560921));
#42940=DIRECTION('center_axis',(-0.707106781186545,0.705126160196082,-0.0528875997482675));
#42941=DIRECTION('ref_axis',(-0.0745860273602106,0.,0.997214582987344));
#42942=DIRECTION('',(0.,0.0747943608453595,0.997198978933359));
#42943=DIRECTION('',(0.,-0.0747943608453595,-0.997198978933359));
#42944=DIRECTION('center_axis',(-0.561006631580385,-0.440444754748121,0.700913673242074));
#42945=DIRECTION('ref_axis',(0.780718990354281,0.,0.624882275392888));
#42946=DIRECTION('',(0.705516335778311,0.188526073789638,0.683157829093256));
#42947=DIRECTION('',(-0.705516335778312,0.697310488411386,-0.126510010281475));
#42948=DIRECTION('',(0.,-0.846707054687377,-0.532059360920026));
#42949=DIRECTION('center_axis',(-0.707106781186541,-0.680690473905417,0.191469263158418));
#42950=DIRECTION('ref_axis',(0.261366100937227,0.,0.965239742903736));
#42951=DIRECTION('',(0.,0.270778428736215,0.962641699975202));
#42952=DIRECTION('',(0.,-0.270778428736215,-0.962641699975202));
#42953=DIRECTION('center_axis',(0.,-0.532059360920026,0.846707054687377));
#42954=DIRECTION('ref_axis',(1.,0.,0.));
#42955=DIRECTION('',(-1.,0.,0.));
#42956=DIRECTION('',(1.,0.,0.));
#42957=DIRECTION('center_axis',(-0.707106781186541,0.122787803968974,0.696364240320026));
#42958=DIRECTION('ref_axis',(0.70167384315987,0.,0.712498293208663));
#42959=DIRECTION('',(0.,0.984807753012208,-0.17364817766693));
#42960=DIRECTION('',(0.,-0.984807753012208,0.17364817766693));
#42961=DIRECTION('center_axis',(0.,0.789563123475643,0.613669352377473));
#42962=DIRECTION('ref_axis',(1.,0.,0.));
#42963=DIRECTION('',(-1.,0.,0.));
#42964=DIRECTION('',(1.,0.,0.));
#42965=DIRECTION('center_axis',(0.707106781186546,-0.680690473905413,0.191469263158417));
#42966=DIRECTION('ref_axis',(0.261366100937224,0.,-0.965239742903737));
#42967=DIRECTION('',(0.,0.270778428736215,0.962641699975202));
#42968=DIRECTION('',(0.,-0.270778428736215,-0.962641699975202));
#42969=DIRECTION('center_axis',(0.707106781186542,0.122787803968974,0.696364240320024));
#42970=DIRECTION('ref_axis',(0.701673843159868,0.,-0.712498293208665));
#42971=DIRECTION('',(0.,0.984807753012208,-0.17364817766693));
#42972=DIRECTION('',(0.,-0.984807753012208,0.17364817766693));
#42973=DIRECTION('center_axis',(0.707106781186546,0.705126160196081,-0.0528875997482674));
#42974=DIRECTION('ref_axis',(-0.0745860273602103,0.,-0.997214582987344));
#42975=DIRECTION('',(0.,0.0747943608453595,0.997198978933359));
#42976=DIRECTION('',(0.,-0.0747943608453595,-0.997198978933359));
#42977=DIRECTION('center_axis',(1.,0.,0.));
#42978=DIRECTION('ref_axis',(0.,-0.17364817766693,-0.984807753012208));
#42979=DIRECTION('center_axis',(0.,0.997198978933359,-0.0747943608453595));
#42980=DIRECTION('ref_axis',(0.,0.0747943608453595,0.997198978933359));
#42981=DIRECTION('center_axis',(0.,0.17364817766693,0.984807753012208));
#42982=DIRECTION('ref_axis',(0.,-0.984807753012208,0.17364817766693));
#42983=DIRECTION('center_axis',(0.561006631580395,0.606846771272568,0.563035128139337));
#42984=DIRECTION('ref_axis',(0.708381704532398,0.,-0.705829554980361));
#42985=DIRECTION('',(0.705516335778303,-0.706293409755772,0.0582779485356275));
#42986=DIRECTION('',(0.,0.680149115692518,-0.733073789207257));
#42987=DIRECTION('',(-0.705516335778312,-0.00528794662206119,0.708673928947909));
#42988=DIRECTION('center_axis',(0.561006631580394,-0.499857381275784,0.659859195364387));
#42989=DIRECTION('ref_axis',(0.761867344215974,0.,-0.64773308531933));
#42990=DIRECTION('',(0.705516335778315,-0.128267547152788,-0.696989337290999));
#42991=DIRECTION('',(0.,0.797113049929625,0.603830096659557));
#42992=DIRECTION('',(-0.705516335778304,-0.70568308539029,0.0652539879547269));
#42993=DIRECTION('center_axis',(-0.561006631580407,0.606846771272561,0.563035128139331));
#42994=DIRECTION('ref_axis',(0.708381704532386,0.,0.705829554980372));
#42995=DIRECTION('',(0.,-0.680149115692518,0.733073789207257));
#42996=DIRECTION('',(0.705516335778306,0.706293409755772,-0.0582779485356024));
#42997=DIRECTION('',(-0.705516335778301,0.00528794662206109,-0.70867392894792));
#42998=DIRECTION('center_axis',(-0.707106781186548,0.707052400311326,0.00876944775867122));
#42999=DIRECTION('ref_axis',(0.0124009183210272,0.,0.999923105656027));
#43000=DIRECTION('',(0.,-0.0124018719548352,0.999923093828728));
#43001=DIRECTION('',(0.,0.0124018719548352,-0.999923093828728));
#43002=DIRECTION('center_axis',(-0.561006631580406,-0.499857381275779,0.659859195364381));
#43003=DIRECTION('ref_axis',(0.761867344215965,0.,0.647733085319341));
#43004=DIRECTION('',(0.705516335778304,0.128267547152789,0.696989337291011));
#43005=DIRECTION('',(-0.705516335778308,0.705683085390284,-0.065253987954752));
#43006=DIRECTION('',(0.,-0.797113049929625,-0.603830096659557));
#43007=DIRECTION('center_axis',(-0.707106781186545,-0.694787886990049,0.131414580971466));
#43008=DIRECTION('ref_axis',(0.182719541232955,0.,0.983165077314903));
#43009=DIRECTION('',(0.,0.185848282703424,0.982578452753869));
#43010=DIRECTION('',(0.,-0.185848282703424,-0.982578452753869));
#43011=DIRECTION('center_axis',(0.,-0.603830096659558,0.797113049929625));
#43012=DIRECTION('ref_axis',(1.,0.,0.));
#43013=DIRECTION('',(-1.,0.,0.));
#43014=DIRECTION('',(1.,0.,0.));
#43015=DIRECTION('center_axis',(-0.707106781186556,0.0616284167162187,0.70441602640275));
#43016=DIRECTION('ref_axis',(0.705757556807943,0.,0.708453436019956));
#43017=DIRECTION('',(0.,0.996194698091746,-0.0871557427476583));
#43018=DIRECTION('',(0.,-0.996194698091746,0.0871557427476583));
#43019=DIRECTION('center_axis',(0.,0.733073789207257,0.680149115692518));
#43020=DIRECTION('ref_axis',(1.,0.,0.));
#43021=DIRECTION('',(-1.,0.,0.));
#43022=DIRECTION('',(1.,0.,0.));
#43023=DIRECTION('center_axis',(0.707106781186546,-0.694787886990048,0.131414580971466));
#43024=DIRECTION('ref_axis',(0.182719541232955,0.,-0.983165077314903));
#43025=DIRECTION('',(0.,0.185848282703424,0.982578452753869));
#43026=DIRECTION('',(0.,-0.185848282703424,-0.982578452753869));
#43027=DIRECTION('center_axis',(0.707106781186545,0.0616284167162197,0.704416026402761));
#43028=DIRECTION('ref_axis',(0.705757556807954,0.,-0.708453436019945));
#43029=DIRECTION('',(0.,0.996194698091746,-0.0871557427476583));
#43030=DIRECTION('',(0.,-0.996194698091746,0.0871557427476583));
#43031=DIRECTION('center_axis',(0.707106781186549,0.707052400311324,0.00876944775867119));
#43032=DIRECTION('ref_axis',(0.0124009183210271,0.,-0.999923105656027));
#43033=DIRECTION('',(0.,-0.0124018719548352,0.999923093828728));
#43034=DIRECTION('',(0.,0.0124018719548352,-0.999923093828728));
#43035=DIRECTION('center_axis',(1.,0.,0.));
#43036=DIRECTION('ref_axis',(0.,-0.0871557427476583,-0.996194698091746));
#43037=DIRECTION('center_axis',(0.,0.999923093828728,0.0124018719548352));
#43038=DIRECTION('ref_axis',(0.,-0.0124018719548352,0.999923093828728));
#43039=DIRECTION('center_axis',(0.,0.0871557427476583,0.996194698091746));
#43040=DIRECTION('ref_axis',(0.,-0.996194698091746,0.0871557427476583));
#43041=DIRECTION('center_axis',(-1.,0.,1.45673360119678E-14));
#43042=DIRECTION('ref_axis',(0.,-1.,-3.05617576116583E-17));
#43043=DIRECTION('center_axis',(-1.,0.,0.));
#43044=DIRECTION('ref_axis',(0.,-1.,-6.12323399573677E-17));
#43045=DIRECTION('center_axis',(-1.,0.,0.));
#43046=DIRECTION('ref_axis',(0.,-1.,-6.12323399573677E-17));
#43047=DIRECTION('',(-0.763019982472722,0.6463748961302,1.12140809161872E-14));
#43048=DIRECTION('center_axis',(1.,0.,0.));
#43049=DIRECTION('ref_axis',(0.,-1.,0.));
#43050=DIRECTION('center_axis',(1.,0.,0.));
#43051=DIRECTION('ref_axis',(0.,-1.,0.));
#43052=DIRECTION('center_axis',(1.,0.,0.));
#43053=DIRECTION('ref_axis',(0.,1.,0.));
#43054=DIRECTION('',(-1.,0.,0.));
#43055=DIRECTION('center_axis',(-1.,0.,0.));
#43056=DIRECTION('ref_axis',(0.,-1.,0.));
#43057=DIRECTION('center_axis',(-1.,0.,0.));
#43058=DIRECTION('ref_axis',(0.,-1.,0.));
#43059=DIRECTION('center_axis',(-1.,0.,0.));
#43060=DIRECTION('ref_axis',(0.,1.,0.));
#43061=DIRECTION('',(-0.164398987305357,-0.986393923832144,-1.20798416151943E-16));
#43062=DIRECTION('center_axis',(-1.,0.,2.35474746642391E-14));
#43063=DIRECTION('ref_axis',(0.,-1.,-3.05127853847422E-17));
#43064=DIRECTION('center_axis',(-1.,0.,0.));
#43065=DIRECTION('ref_axis',(0.,-1.,0.));
#43066=DIRECTION('',(0.358263767183369,-0.933620411689666,-8.35035881523851E-15));
#43067=DIRECTION('center_axis',(-1.,0.,0.));
#43068=DIRECTION('ref_axis',(0.,0.,1.));
#43069=DIRECTION('center_axis',(1.,0.,0.));
#43070=DIRECTION('ref_axis',(0.,-1.,0.));
#43071=DIRECTION('center_axis',(1.,0.,-9.94623938728346E-15));
#43072=DIRECTION('ref_axis',(0.,-1.,-3.05771835236612E-17));
#43073=DIRECTION('center_axis',(1.,0.,0.));
#43074=DIRECTION('ref_axis',(0.,-1.,-6.12323399573677E-17));
#43075=DIRECTION('',(0.923879532511288,0.382683432365087,-9.22429081787917E-15));
#43076=DIRECTION('center_axis',(1.,0.,0.));
#43077=DIRECTION('ref_axis',(0.,-1.,0.));
#43078=DIRECTION('',(-0.707106781186549,-0.707106781186546,-8.65956056235492E-17));
#43079=DIRECTION('center_axis',(-1.,0.,0.));
#43080=DIRECTION('ref_axis',(0.,-1.,-6.12323399573677E-17));
#43081=DIRECTION('center_axis',(1.,0.,2.39616194920574E-14));
#43082=DIRECTION('ref_axis',(0.,-1.,-3.07109033448888E-17));
#43083=DIRECTION('',(-0.382683432365081,-0.92387953251129,-9.31123057850062E-15));
#43084=DIRECTION('center_axis',(0.,-0.982578452753869,0.185848282703424));
#43085=DIRECTION('ref_axis',(0.,-0.185848282703424,-0.982578452753869));
#43086=DIRECTION('center_axis',(1.,0.,0.));
#43087=DIRECTION('ref_axis',(0.,-0.0871557427476583,-0.996194698091746));
#43088=DIRECTION('center_axis',(0.,-0.962641699975202,0.270778428736215));
#43089=DIRECTION('ref_axis',(0.,-0.270778428736215,-0.962641699975202));
#43090=DIRECTION('center_axis',(1.,0.,0.));
#43091=DIRECTION('ref_axis',(0.,-0.17364817766693,-0.984807753012208));
#43092=DIRECTION('center_axis',(0.,-0.935378662600772,0.353647787425838));
#43093=DIRECTION('ref_axis',(0.,-0.353647787425838,-0.935378662600772));
#43094=DIRECTION('center_axis',(1.,0.,0.));
#43095=DIRECTION('ref_axis',(0.,-0.258819045102521,-0.965925826289068));
#43096=DIRECTION('center_axis',(0.,-0.900996828806872,0.433825672914779));
#43097=DIRECTION('ref_axis',(0.,-0.433825672914779,-0.900996828806872));
#43098=DIRECTION('center_axis',(1.,0.,0.));
#43099=DIRECTION('ref_axis',(0.,-0.342020143325669,-0.939692620785908));
#43100=DIRECTION('center_axis',(1.,0.,0.));
#43101=DIRECTION('ref_axis',(0.,-0.4226182617407,-0.90630778703665));
#43102=DIRECTION('center_axis',(1.,0.,0.));
#43103=DIRECTION('ref_axis',(0.,-0.4226182617407,-0.90630778703665));
#43104=DIRECTION('center_axis',(0.,-0.811975624921639,0.583691343548209));
#43105=DIRECTION('ref_axis',(0.,-0.583691343548209,-0.81197562492164));
#43106=DIRECTION('center_axis',(1.,0.,0.));
#43107=DIRECTION('ref_axis',(0.,-0.5,-0.866025403784438));
#43108=DIRECTION('center_axis',(1.,0.,0.));
#43109=DIRECTION('ref_axis',(0.,-0.573576436351046,-0.819152044288992));
#43110=DIRECTION('center_axis',(0.,-0.758013759944346,0.652238560447813));
#43111=DIRECTION('ref_axis',(0.,-0.652238560447812,-0.758013759944346));
#43112=DIRECTION('center_axis',(0.,-0.698282952552655,0.715821848069998));
#43113=DIRECTION('ref_axis',(0.,-0.715821848069998,-0.698282952552655));
#43114=DIRECTION('center_axis',(1.,0.,0.));
#43115=DIRECTION('ref_axis',(0.,-0.64278760968654,-0.766044443118978));
#43116=DIRECTION('center_axis',(0.,-0.633237790257263,0.773957299203321));
#43117=DIRECTION('ref_axis',(0.,-0.773957299203321,-0.633237790257263));
#43118=DIRECTION('center_axis',(1.,0.,0.));
#43119=DIRECTION('ref_axis',(0.,-0.707106781186548,-0.707106781186547));
#43120=DIRECTION('center_axis',(1.,0.,0.));
#43121=DIRECTION('ref_axis',(0.,-0.766044443118978,-0.642787609686539));
#43122=DIRECTION('center_axis',(1.,0.,0.));
#43123=DIRECTION('ref_axis',(0.,-0.766044443118978,-0.642787609686539));
#43124=DIRECTION('center_axis',(0.,-0.489221210746995,0.872159737063827));
#43125=DIRECTION('ref_axis',(0.,-0.872159737063827,-0.489221210746995));
#43126=DIRECTION('center_axis',(1.,0.,0.));
#43127=DIRECTION('ref_axis',(0.,-0.819152044288992,-0.573576436351046));
#43128=DIRECTION('center_axis',(1.,0.,0.));
#43129=DIRECTION('ref_axis',(0.,-0.866025403784439,-0.5));
#43130=DIRECTION('center_axis',(0.,-0.411345846661781,0.911479343942639));
#43131=DIRECTION('ref_axis',(0.,-0.911479343942638,-0.411345846661781));
#43132=DIRECTION('center_axis',(0.,-0.330339892306057,0.943862042647771));
#43133=DIRECTION('ref_axis',(0.,-0.943862042647771,-0.330339892306057));
#43134=DIRECTION('center_axis',(1.,0.,0.));
#43135=DIRECTION('ref_axis',(0.,-0.90630778703665,-0.422618261740699));
#43136=DIRECTION('center_axis',(0.,-0.246819851905204,0.96906138128887));
#43137=DIRECTION('ref_axis',(0.,-0.96906138128887,-0.246819851905204));
#43138=DIRECTION('center_axis',(1.,0.,0.));
#43139=DIRECTION('ref_axis',(0.,-0.939692620785909,-0.342020143325668));
#43140=DIRECTION('center_axis',(1.,0.,0.));
#43141=DIRECTION('ref_axis',(0.,-0.965925826289068,-0.25881904510252));
#43142=DIRECTION('center_axis',(1.,0.,0.));
#43143=DIRECTION('ref_axis',(0.,-0.965925826289068,-0.25881904510252));
#43144=DIRECTION('center_axis',(0.,-0.0747943608453591,0.997198978933359));
#43145=DIRECTION('ref_axis',(0.,-0.997198978933359,-0.0747943608453591));
#43146=DIRECTION('center_axis',(1.,0.,0.));
#43147=DIRECTION('ref_axis',(0.,-0.984807753012208,-0.17364817766693));
#43148=DIRECTION('center_axis',(1.,0.,0.));
#43149=DIRECTION('ref_axis',(0.,-0.996194698091746,-0.0871557427476579));
#43150=DIRECTION('center_axis',(0.,0.0124018719548356,0.999923093828728));
#43151=DIRECTION('ref_axis',(0.,-0.999923093828728,0.0124018719548356));
#43152=DIRECTION('center_axis',(0.,0.099503719020999,0.995037190209989));
#43153=DIRECTION('ref_axis',(0.,-0.995037190209989,0.099503719020999));
#43154=DIRECTION('center_axis',(1.,0.,0.));
#43155=DIRECTION('ref_axis',(0.,-1.,1.83697019872103E-16));
#43156=DIRECTION('center_axis',(0.,0.185848282703424,0.98257845275387));
#43157=DIRECTION('ref_axis',(0.,-0.982578452753869,0.185848282703424));
#43158=DIRECTION('center_axis',(1.,0.,0.));
#43159=DIRECTION('ref_axis',(0.,-0.996194698091746,0.0871557427476582));
#43160=DIRECTION('center_axis',(1.,0.,0.));
#43161=DIRECTION('ref_axis',(0.,-0.984807753012208,0.17364817766693));
#43162=DIRECTION('center_axis',(1.,0.,0.));
#43163=DIRECTION('ref_axis',(0.,-0.984807753012208,0.17364817766693));
#43164=DIRECTION('center_axis',(0.,0.353647787425838,0.935378662600772));
#43165=DIRECTION('ref_axis',(0.,-0.935378662600772,0.353647787425838));
#43166=DIRECTION('center_axis',(1.,0.,0.));
#43167=DIRECTION('ref_axis',(0.,-0.965925826289068,0.258819045102521));
#43168=DIRECTION('center_axis',(1.,0.,0.));
#43169=DIRECTION('ref_axis',(0.,-0.939692620785908,0.342020143325669));
#43170=DIRECTION('center_axis',(0.,0.433825672914779,0.900996828806872));
#43171=DIRECTION('ref_axis',(0.,-0.900996828806872,0.433825672914779));
#43172=DIRECTION('center_axis',(0.,0.510701883081734,0.859757865108992));
#43173=DIRECTION('ref_axis',(0.,-0.859757865108992,0.510701883081734));
#43174=DIRECTION('center_axis',(1.,0.,0.));
#43175=DIRECTION('ref_axis',(0.,-0.90630778703665,0.4226182617407));
#43176=DIRECTION('center_axis',(0.,0.583691343548209,0.811975624921639));
#43177=DIRECTION('ref_axis',(0.,-0.81197562492164,0.583691343548209));
#43178=DIRECTION('center_axis',(1.,0.,0.));
#43179=DIRECTION('ref_axis',(0.,-0.866025403784438,0.5));
#43180=DIRECTION('center_axis',(1.,0.,0.));
#43181=DIRECTION('ref_axis',(0.,-0.819152044288992,0.573576436351046));
#43182=DIRECTION('center_axis',(1.,0.,0.));
#43183=DIRECTION('ref_axis',(0.,-0.819152044288992,0.573576436351046));
#43184=DIRECTION('center_axis',(0.,0.715821848069998,0.698282952552655));
#43185=DIRECTION('ref_axis',(0.,-0.698282952552655,0.715821848069998));
#43186=DIRECTION('center_axis',(1.,0.,0.));
#43187=DIRECTION('ref_axis',(0.,-0.766044443118978,0.642787609686539));
#43188=DIRECTION('center_axis',(1.,0.,0.));
#43189=DIRECTION('ref_axis',(0.,-0.707106781186547,0.707106781186548));
#43190=DIRECTION('center_axis',(0.,0.773957299203321,0.633237790257263));
#43191=DIRECTION('ref_axis',(0.,-0.633237790257263,0.773957299203321));
#43192=DIRECTION('center_axis',(0.,0.826202467961513,0.563373306018581));
#43193=DIRECTION('ref_axis',(0.,-0.563373306018581,0.826202467961513));
#43194=DIRECTION('center_axis',(1.,0.,0.));
#43195=DIRECTION('ref_axis',(0.,-0.642787609686539,0.766044443118978));
#43196=DIRECTION('center_axis',(0.,0.872159737063828,0.489221210746995));
#43197=DIRECTION('ref_axis',(0.,-0.489221210746995,0.872159737063827));
#43198=DIRECTION('center_axis',(1.,0.,0.));
#43199=DIRECTION('ref_axis',(0.,-0.573576436351046,0.819152044288992));
#43200=DIRECTION('center_axis',(1.,0.,0.));
#43201=DIRECTION('ref_axis',(0.,-0.5,0.866025403784439));
#43202=DIRECTION('center_axis',(1.,0.,0.));
#43203=DIRECTION('ref_axis',(0.,-0.5,0.866025403784439));
#43204=DIRECTION('center_axis',(0.,0.943862042647771,0.330339892306057));
#43205=DIRECTION('ref_axis',(0.,-0.330339892306057,0.943862042647771));
#43206=DIRECTION('center_axis',(1.,0.,0.));
#43207=DIRECTION('ref_axis',(0.,-0.422618261740699,0.90630778703665));
#43208=DIRECTION('center_axis',(1.,0.,0.));
#43209=DIRECTION('ref_axis',(0.,-0.342020143325669,0.939692620785909));
#43210=DIRECTION('center_axis',(0.,0.96906138128887,0.246819851905204));
#43211=DIRECTION('ref_axis',(0.,-0.246819851905204,0.96906138128887));
#43212=DIRECTION('center_axis',(0.,0.986885577683101,0.161421363397451));
#43213=DIRECTION('ref_axis',(0.,-0.161421363397451,0.986885577683101));
#43214=DIRECTION('center_axis',(1.,0.,0.));
#43215=DIRECTION('ref_axis',(0.,-0.258819045102521,0.965925826289068));
#43216=DIRECTION('center_axis',(0.,0.997198978933359,0.0747943608453591));
#43217=DIRECTION('ref_axis',(0.,-0.0747943608453591,0.997198978933359));
#43218=DIRECTION('center_axis',(1.,0.,0.));
#43219=DIRECTION('ref_axis',(0.,-0.17364817766693,0.984807753012208));
#43220=DIRECTION('center_axis',(1.,0.,0.));
#43221=DIRECTION('ref_axis',(0.,-0.0871557427476579,0.996194698091746));
#43222=DIRECTION('center_axis',(1.,0.,0.));
#43223=DIRECTION('ref_axis',(0.,-0.0871557427476579,0.996194698091746));
#43224=DIRECTION('center_axis',(0.,0.995037190209989,-0.0995037190209989));
#43225=DIRECTION('ref_axis',(0.,0.0995037190209989,0.995037190209989));
#43226=DIRECTION('center_axis',(1.,0.,0.));
#43227=DIRECTION('ref_axis',(0.,1.22464679914735E-16,1.));
#43228=DIRECTION('center_axis',(1.,0.,0.));
#43229=DIRECTION('ref_axis',(0.,0.0871557427476582,0.996194698091746));
#43230=DIRECTION('center_axis',(0.,0.98257845275387,-0.185848282703424));
#43231=DIRECTION('ref_axis',(0.,0.185848282703424,0.982578452753869));
#43232=DIRECTION('center_axis',(0.,0.962641699975202,-0.270778428736216));
#43233=DIRECTION('ref_axis',(0.,0.270778428736216,0.962641699975202));
#43234=DIRECTION('center_axis',(1.,0.,0.));
#43235=DIRECTION('ref_axis',(0.,0.173648177666931,0.984807753012208));
#43236=DIRECTION('center_axis',(0.,0.935378662600772,-0.353647787425838));
#43237=DIRECTION('ref_axis',(0.,0.353647787425838,0.935378662600772));
#43238=DIRECTION('center_axis',(1.,0.,0.));
#43239=DIRECTION('ref_axis',(0.,0.258819045102521,0.965925826289068));
#43240=DIRECTION('center_axis',(1.,0.,0.));
#43241=DIRECTION('ref_axis',(0.,0.342020143325669,0.939692620785908));
#43242=DIRECTION('center_axis',(1.,0.,0.));
#43243=DIRECTION('ref_axis',(0.,0.342020143325669,0.939692620785908));
#43244=DIRECTION('center_axis',(0.,0.859757865108992,-0.510701883081733));
#43245=DIRECTION('ref_axis',(0.,0.510701883081733,0.859757865108992));
#43246=DIRECTION('center_axis',(1.,0.,0.));
#43247=DIRECTION('ref_axis',(0.,0.422618261740699,0.90630778703665));
#43248=DIRECTION('center_axis',(1.,0.,0.));
#43249=DIRECTION('ref_axis',(0.,0.5,0.866025403784439));
#43250=DIRECTION('center_axis',(0.,0.81197562492164,-0.583691343548208));
#43251=DIRECTION('ref_axis',(0.,0.583691343548208,0.81197562492164));
#43252=DIRECTION('center_axis',(0.,0.758013759944346,-0.652238560447812));
#43253=DIRECTION('ref_axis',(0.,0.652238560447812,0.758013759944346));
#43254=DIRECTION('center_axis',(1.,0.,0.));
#43255=DIRECTION('ref_axis',(0.,0.573576436351046,0.819152044288992));
#43256=DIRECTION('center_axis',(0.,0.698282952552655,-0.715821848069998));
#43257=DIRECTION('ref_axis',(0.,0.715821848069998,0.698282952552655));
#43258=DIRECTION('center_axis',(1.,0.,0.));
#43259=DIRECTION('ref_axis',(0.,0.642787609686539,0.766044443118978));
#43260=DIRECTION('center_axis',(1.,0.,0.));
#43261=DIRECTION('ref_axis',(0.,0.707106781186548,0.707106781186547));
#43262=DIRECTION('center_axis',(1.,0.,0.));
#43263=DIRECTION('ref_axis',(0.,0.707106781186548,0.707106781186547));
#43264=DIRECTION('center_axis',(0.,0.563373306018581,-0.826202467961513));
#43265=DIRECTION('ref_axis',(0.,0.826202467961513,0.563373306018581));
#43266=DIRECTION('center_axis',(1.,0.,0.));
#43267=DIRECTION('ref_axis',(0.,0.766044443118978,0.642787609686539));
#43268=DIRECTION('center_axis',(1.,0.,0.));
#43269=DIRECTION('ref_axis',(0.,0.819152044288992,0.573576436351046));
#43270=DIRECTION('center_axis',(0.,0.489221210746995,-0.872159737063828));
#43271=DIRECTION('ref_axis',(0.,0.872159737063827,0.489221210746995));
#43272=DIRECTION('center_axis',(0.,0.411345846661781,-0.911479343942639));
#43273=DIRECTION('ref_axis',(0.,0.911479343942639,0.411345846661781));
#43274=DIRECTION('center_axis',(1.,0.,0.));
#43275=DIRECTION('ref_axis',(0.,0.866025403784439,0.5));
#43276=DIRECTION('center_axis',(0.,0.330339892306057,-0.943862042647771));
#43277=DIRECTION('ref_axis',(0.,0.943862042647771,0.330339892306057));
#43278=DIRECTION('center_axis',(1.,0.,0.));
#43279=DIRECTION('ref_axis',(0.,0.90630778703665,0.422618261740699));
#43280=DIRECTION('center_axis',(1.,0.,0.));
#43281=DIRECTION('ref_axis',(0.,0.939692620785908,0.342020143325669));
#43282=DIRECTION('center_axis',(1.,0.,0.));
#43283=DIRECTION('ref_axis',(0.,0.939692620785908,0.342020143325669));
#43284=DIRECTION('center_axis',(0.,0.161421363397451,-0.986885577683101));
#43285=DIRECTION('ref_axis',(0.,0.986885577683101,0.161421363397451));
#43286=DIRECTION('center_axis',(1.,0.,0.));
#43287=DIRECTION('ref_axis',(0.,0.965925826289068,0.258819045102521));
#43288=DIRECTION('center_axis',(1.,0.,0.));
#43289=DIRECTION('ref_axis',(0.,0.984807753012208,0.17364817766693));
#43290=DIRECTION('center_axis',(0.,0.0747943608453594,-0.997198978933359));
#43291=DIRECTION('ref_axis',(0.,0.997198978933359,0.0747943608453594));
#43292=DIRECTION('center_axis',(0.,-0.0124018719548355,-0.999923093828728));
#43293=DIRECTION('ref_axis',(0.,0.999923093828728,-0.0124018719548355));
#43294=DIRECTION('center_axis',(1.,0.,0.));
#43295=DIRECTION('ref_axis',(0.,0.996194698091746,0.087155742747658));
#43296=DIRECTION('center_axis',(0.,-0.0995037190209988,-0.995037190209989));
#43297=DIRECTION('ref_axis',(0.,0.995037190209989,-0.0995037190209988));
#43298=DIRECTION('center_axis',(1.,0.,0.));
#43299=DIRECTION('ref_axis',(0.,1.,-6.12323399573677E-17));
#43300=DIRECTION('center_axis',(1.,0.,0.));
#43301=DIRECTION('ref_axis',(0.,0.996194698091746,-0.0871557427476584));
#43302=DIRECTION('center_axis',(1.,0.,0.));
#43303=DIRECTION('ref_axis',(0.,0.996194698091746,-0.0871557427476584));
#43304=DIRECTION('center_axis',(0.,-0.270778428736215,-0.962641699975202));
#43305=DIRECTION('ref_axis',(0.,0.962641699975202,-0.270778428736215));
#43306=DIRECTION('center_axis',(1.,0.,0.));
#43307=DIRECTION('ref_axis',(0.,0.984807753012208,-0.17364817766693));
#43308=DIRECTION('center_axis',(1.,0.,0.));
#43309=DIRECTION('ref_axis',(0.,0.965925826289068,-0.258819045102521));
#43310=DIRECTION('center_axis',(0.,-0.353647787425838,-0.935378662600772));
#43311=DIRECTION('ref_axis',(0.,0.935378662600772,-0.353647787425838));
#43312=DIRECTION('center_axis',(0.,-0.433825672914778,-0.900996828806872));
#43313=DIRECTION('ref_axis',(0.,0.900996828806872,-0.433825672914778));
#43314=DIRECTION('center_axis',(1.,0.,0.));
#43315=DIRECTION('ref_axis',(0.,0.939692620785908,-0.342020143325669));
#43316=DIRECTION('center_axis',(0.,-0.510701883081733,-0.859757865108992));
#43317=DIRECTION('ref_axis',(0.,0.859757865108992,-0.510701883081733));
#43318=DIRECTION('center_axis',(1.,0.,0.));
#43319=DIRECTION('ref_axis',(0.,0.90630778703665,-0.422618261740699));
#43320=DIRECTION('center_axis',(1.,0.,0.));
#43321=DIRECTION('ref_axis',(0.,0.866025403784439,-0.5));
#43322=DIRECTION('center_axis',(1.,0.,0.));
#43323=DIRECTION('ref_axis',(0.,0.866025403784439,-0.5));
#43324=DIRECTION('center_axis',(0.,-0.652238560447812,-0.758013759944347));
#43325=DIRECTION('ref_axis',(0.,0.758013759944347,-0.652238560447812));
#43326=DIRECTION('center_axis',(1.,0.,0.));
#43327=DIRECTION('ref_axis',(0.,0.819152044288992,-0.573576436351046));
#43328=DIRECTION('center_axis',(1.,0.,0.));
#43329=DIRECTION('ref_axis',(0.,0.766044443118978,-0.642787609686539));
#43330=DIRECTION('center_axis',(0.,-0.715821848069998,-0.698282952552655));
#43331=DIRECTION('ref_axis',(0.,0.698282952552655,-0.715821848069998));
#43332=DIRECTION('center_axis',(0.,-0.773957299203321,-0.633237790257263));
#43333=DIRECTION('ref_axis',(0.,0.633237790257263,-0.773957299203321));
#43334=DIRECTION('center_axis',(1.,0.,0.));
#43335=DIRECTION('ref_axis',(0.,0.707106781186548,-0.707106781186548));
#43336=DIRECTION('center_axis',(0.,-0.826202467961513,-0.563373306018581));
#43337=DIRECTION('ref_axis',(0.,0.563373306018581,-0.826202467961513));
#43338=DIRECTION('center_axis',(1.,0.,0.));
#43339=DIRECTION('ref_axis',(0.,0.642787609686539,-0.766044443118978));
#43340=DIRECTION('center_axis',(1.,0.,0.));
#43341=DIRECTION('ref_axis',(0.,0.573576436351046,-0.819152044288992));
#43342=DIRECTION('center_axis',(1.,0.,0.));
#43343=DIRECTION('ref_axis',(0.,0.573576436351046,-0.819152044288992));
#43344=DIRECTION('center_axis',(0.,-0.911479343942639,-0.411345846661781));
#43345=DIRECTION('ref_axis',(0.,0.411345846661781,-0.911479343942639));
#43346=DIRECTION('center_axis',(1.,0.,0.));
#43347=DIRECTION('ref_axis',(0.,0.5,-0.866025403784439));
#43348=DIRECTION('center_axis',(1.,0.,0.));
#43349=DIRECTION('ref_axis',(0.,0.422618261740699,-0.90630778703665));
#43350=DIRECTION('center_axis',(0.,-0.943862042647771,-0.330339892306057));
#43351=DIRECTION('ref_axis',(0.,0.330339892306057,-0.943862042647771));
#43352=DIRECTION('center_axis',(0.,-0.96906138128887,-0.246819851905204));
#43353=DIRECTION('ref_axis',(0.,0.246819851905204,-0.96906138128887));
#43354=DIRECTION('center_axis',(1.,0.,0.));
#43355=DIRECTION('ref_axis',(0.,0.342020143325669,-0.939692620785908));
#43356=DIRECTION('center_axis',(0.,-0.986885577683101,-0.161421363397451));
#43357=DIRECTION('ref_axis',(0.,0.161421363397451,-0.986885577683101));
#43358=DIRECTION('center_axis',(1.,0.,0.));
#43359=DIRECTION('ref_axis',(0.,0.258819045102521,-0.965925826289068));
#43360=DIRECTION('center_axis',(1.,0.,0.));
#43361=DIRECTION('ref_axis',(0.,0.17364817766693,-0.984807753012208));
#43362=DIRECTION('center_axis',(1.,0.,0.));
#43363=DIRECTION('ref_axis',(0.,0.17364817766693,-0.984807753012208));
#43364=DIRECTION('center_axis',(0.,-0.999923093828728,0.0124018719548353));
#43365=DIRECTION('ref_axis',(0.,-0.0124018719548353,-0.999923093828728));
#43366=DIRECTION('center_axis',(1.,0.,0.));
#43367=DIRECTION('ref_axis',(0.,0.0871557427476582,-0.996194698091746));
#43368=DIRECTION('center_axis',(1.,0.,0.));
#43369=DIRECTION('ref_axis',(0.,0.,-1.));
#43370=DIRECTION('center_axis',(0.,-0.995037190209989,0.0995037190209988));
#43371=DIRECTION('ref_axis',(0.,-0.0995037190209988,-0.995037190209989));
#43372=DIRECTION('center_axis',(-1.,0.,0.));
#43373=DIRECTION('ref_axis',(0.,0.,-1.));
#43374=DIRECTION('',(-1.,0.,0.));
#43375=DIRECTION('center_axis',(1.,0.,0.));
#43376=DIRECTION('ref_axis',(0.,0.,-1.));
#43377=DIRECTION('center_axis',(-1.,0.,0.));
#43378=DIRECTION('ref_axis',(0.,0.,-1.));
#43379=DIRECTION('',(-1.,0.,0.));
#43380=DIRECTION('center_axis',(1.,0.,0.));
#43381=DIRECTION('ref_axis',(0.,0.,-1.));
#43382=DIRECTION('center_axis',(-1.,0.,0.));
#43383=DIRECTION('ref_axis',(0.,0.,-1.));
#43384=DIRECTION('',(-1.,0.,0.));
#43385=DIRECTION('center_axis',(1.,0.,0.));
#43386=DIRECTION('ref_axis',(0.,0.,-1.));
#43387=DIRECTION('center_axis',(-1.,0.,0.));
#43388=DIRECTION('ref_axis',(0.,0.,-1.));
#43389=DIRECTION('',(-1.,0.,0.));
#43390=DIRECTION('center_axis',(1.,0.,0.));
#43391=DIRECTION('ref_axis',(0.,0.,-1.));
#43392=DIRECTION('center_axis',(-1.,0.,0.));
#43393=DIRECTION('ref_axis',(0.,0.,-1.));
#43394=DIRECTION('',(-1.,0.,0.));
#43395=DIRECTION('center_axis',(1.,0.,0.));
#43396=DIRECTION('ref_axis',(0.,0.,-1.));
#43397=DIRECTION('center_axis',(-1.,0.,0.));
#43398=DIRECTION('ref_axis',(0.,1.,0.));
#43399=DIRECTION('center_axis',(1.,0.,0.));
#43400=DIRECTION('ref_axis',(0.,0.,-1.));
#43401=DIRECTION('',(0.447213595499958,0.894427190999916,1.09535739652841E-16));
#43402=DIRECTION('center_axis',(1.,0.,0.));
#43403=DIRECTION('ref_axis',(0.,0.,-1.));
#43404=DIRECTION('center_axis',(1.,0.,0.));
#43405=DIRECTION('ref_axis',(0.,1.,0.));
#43406=DIRECTION('',(1.,0.,0.));
#43407=DIRECTION('center_axis',(-1.,0.,0.));
#43408=DIRECTION('ref_axis',(0.,1.,0.));
#43409=DIRECTION('center_axis',(1.,0.,0.));
#43410=DIRECTION('ref_axis',(0.,-0.951056516295154,0.309016994374948));
#43411=DIRECTION('',(1.,0.,0.));
#43412=DIRECTION('center_axis',(-1.,0.,0.));
#43413=DIRECTION('ref_axis',(0.,0.,-1.));
#43414=DIRECTION('center_axis',(1.,0.,0.));
#43415=DIRECTION('ref_axis',(0.,0.,-1.));
#43416=DIRECTION('',(1.,0.,0.));
#43417=DIRECTION('center_axis',(-1.,0.,0.));
#43418=DIRECTION('ref_axis',(0.,0.,-1.));
#43419=DIRECTION('center_axis',(1.,0.,0.));
#43420=DIRECTION('ref_axis',(0.,5.66553889764798E-16,1.));
#43421=DIRECTION('',(1.,0.,0.));
#43422=DIRECTION('center_axis',(-1.,0.,0.));
#43423=DIRECTION('ref_axis',(0.,0.,-1.));
#43424=DIRECTION('center_axis',(1.,0.,0.));
#43425=DIRECTION('ref_axis',(0.,0.,-1.));
#43426=DIRECTION('center_axis',(-1.,0.,0.));
#43427=DIRECTION('ref_axis',(0.,0.,-1.));
#43428=DIRECTION('center_axis',(1.,0.,0.));
#43429=DIRECTION('ref_axis',(0.,0.,-1.));
#43430=DIRECTION('center_axis',(1.,0.,0.));
#43431=DIRECTION('ref_axis',(0.,1.,0.));
#43432=DIRECTION('',(-1.,0.,0.));
#43433=DIRECTION('center_axis',(1.,0.,0.));
#43434=DIRECTION('ref_axis',(0.,0.,-1.));
#43435=DIRECTION('center_axis',(1.,0.,0.));
#43436=DIRECTION('ref_axis',(0.,0.,-1.));
#43437=DIRECTION('center_axis',(1.,0.,0.));
#43438=DIRECTION('ref_axis',(0.,1.,0.));
#43439=DIRECTION('',(-1.,0.,0.));
#43440=DIRECTION('center_axis',(1.,0.,0.));
#43441=DIRECTION('ref_axis',(0.,0.,-1.));
#43442=DIRECTION('center_axis',(1.,0.,0.));
#43443=DIRECTION('ref_axis',(0.,0.,-1.));
#43444=DIRECTION('center_axis',(1.,0.,0.));
#43445=DIRECTION('ref_axis',(0.,1.,0.));
#43446=DIRECTION('',(-1.,0.,0.));
#43447=DIRECTION('center_axis',(1.,0.,0.));
#43448=DIRECTION('ref_axis',(0.,0.,-1.));
#43449=DIRECTION('center_axis',(-1.,0.,0.));
#43450=DIRECTION('ref_axis',(0.,0.,1.));
#43451=DIRECTION('center_axis',(1.,0.,0.));
#43452=DIRECTION('ref_axis',(0.,0.,-1.));
#43453=DIRECTION('center_axis',(1.,0.,0.));
#43454=DIRECTION('ref_axis',(0.,1.,0.));
#43455=DIRECTION('',(-1.,0.,0.));
#43456=DIRECTION('center_axis',(1.,0.,0.));
#43457=DIRECTION('ref_axis',(0.,0.,-1.));
#43458=DIRECTION('center_axis',(-1.,0.,0.));
#43459=DIRECTION('ref_axis',(0.,1.,0.));
#43460=DIRECTION('',(-0.707106781186547,-0.707106781186548,-8.65956056235494E-17));
#43461=DIRECTION('center_axis',(1.,0.,0.));
#43462=DIRECTION('ref_axis',(0.,1.,0.));
#43463=DIRECTION('center_axis',(1.,0.,0.));
#43464=DIRECTION('ref_axis',(0.,0.,-1.));
#43465=DIRECTION('',(-0.707106781186548,0.707106781186547,8.65956056235493E-17));
#43466=DIRECTION('center_axis',(-1.,0.,0.));
#43467=DIRECTION('ref_axis',(0.,0.,1.));
#43468=DIRECTION('center_axis',(1.,0.,0.));
#43469=DIRECTION('ref_axis',(0.,0.,-1.));
#43470=DIRECTION('center_axis',(-1.,0.,0.));
#43471=DIRECTION('ref_axis',(0.,1.,0.));
#43472=DIRECTION('',(-0.496138938356835,-0.868243142124459,-1.06329118488436E-16));
#43473=DIRECTION('center_axis',(1.,0.,0.));
#43474=DIRECTION('ref_axis',(0.,0.,-1.));
#43475=DIRECTION('center_axis',(-1.,0.,0.));
#43476=DIRECTION('ref_axis',(0.,1.,0.));
#43477=DIRECTION('',(-0.447213595499971,-0.89442719099991,-1.0953573965284E-16));
#43478=DIRECTION('axis',(0.,0.,1.));
#43479=DIRECTION('refdir',(1.,0.,0.));
#43480=DIRECTION('center_axis',(1.,0.,0.));
#43481=DIRECTION('ref_axis',(0.,0.655966063895196,-0.754790383495871));
#43482=DIRECTION('',(1.,0.,0.));
#43483=DIRECTION('center_axis',(1.,0.,0.));
#43484=DIRECTION('ref_axis',(0.,1.,4.47017618667391E-14));
#43485=DIRECTION('',(1.,0.,0.));
#43486=DIRECTION('center_axis',(1.,0.,0.));
#43487=DIRECTION('ref_axis',(0.,1.,4.47017618667391E-14));
#43488=DIRECTION('',(1.,0.,0.));
#43489=DIRECTION('center_axis',(1.,0.,0.));
#43490=DIRECTION('ref_axis',(0.,1.,4.47017618667391E-14));
#43491=DIRECTION('',(1.,0.,0.));
#43492=DIRECTION('center_axis',(1.,0.,0.));
#43493=DIRECTION('ref_axis',(0.,1.,4.47017618667391E-14));
#43494=DIRECTION('',(1.,0.,0.));
#43495=DIRECTION('center_axis',(1.,0.,0.));
#43496=DIRECTION('ref_axis',(0.,1.,4.47017618667391E-14));
#43497=DIRECTION('',(1.,0.,0.));
#43498=DIRECTION('center_axis',(1.,0.,0.));
#43499=DIRECTION('ref_axis',(0.,0.947929631065919,-0.31847984951521));
#43500=DIRECTION('',(1.,0.,0.));
#43501=DIRECTION('center_axis',(1.,0.,0.));
#43502=DIRECTION('ref_axis',(0.,1.,4.47017618667391E-14));
#43503=DIRECTION('center_axis',(1.,0.,0.));
#43504=DIRECTION('ref_axis',(0.,1.,4.47017618667391E-14));
#43505=DIRECTION('',(1.,0.,0.));
#43506=DIRECTION('center_axis',(1.,0.,0.));
#43507=DIRECTION('ref_axis',(0.,1.,4.47017618667391E-14));
#43508=DIRECTION('',(1.,0.,0.));
#43509=DIRECTION('center_axis',(1.,0.,3.99334313142758E-16));
#43510=DIRECTION('ref_axis',(0.,1.,2.6597345215342E-17));
#43511=DIRECTION('center_axis',(1.,0.,0.));
#43512=DIRECTION('ref_axis',(0.,1.,0.));
#43513=DIRECTION('',(-0.452487571992747,0.891770708866415,-4.77646659520457E-17));
#43514=DIRECTION('center_axis',(-1.,0.,0.));
#43515=DIRECTION('ref_axis',(0.,1.,6.12323399573677E-17));
#43516=DIRECTION('center_axis',(1.,0.,0.));
#43517=DIRECTION('ref_axis',(0.,1.,0.));
#43518=DIRECTION('',(0.807030325658429,-0.590509994384219,-7.23166174487155E-17));
#43519=DIRECTION('center_axis',(1.,0.,0.));
#43520=DIRECTION('ref_axis',(0.,0.,-1.));
#43521=DIRECTION('center_axis',(1.,0.,0.));
#43522=DIRECTION('ref_axis',(0.,0.,-1.));
#43523=DIRECTION('center_axis',(0.707106781186543,0.,-0.707106781186552));
#43524=DIRECTION('ref_axis',(-0.707106781186552,0.,-0.707106781186543));
#43525=DIRECTION('',(0.707106781186552,0.,0.707106781186543));
#43526=DIRECTION('',(0.,1.,0.));
#43527=DIRECTION('',(-0.707106781186552,0.,-0.707106781186543));
#43528=DIRECTION('',(0.,-1.,0.));
#43529=DIRECTION('center_axis',(0.,0.,1.));
#43530=DIRECTION('ref_axis',(0.,1.,0.));
#43531=DIRECTION('',(-1.,0.,0.));
#43532=DIRECTION('',(0.,1.,0.));
#43533=DIRECTION('',(-1.,0.,0.));
#43534=DIRECTION('center_axis',(0.,-0.38268343236509,0.923879532511287));
#43535=DIRECTION('ref_axis',(1.,0.,0.));
#43536=DIRECTION('',(-0.357406744336595,0.862856209461016,0.357406744336593));
#43537=DIRECTION('',(-1.,0.,0.));
#43538=DIRECTION('',(-0.357406744336594,-0.862856209461017,-0.357406744336594));
#43539=DIRECTION('',(0.357406744336593,-0.862856209461017,-0.357406744336594));
#43540=DIRECTION('',(1.,0.,0.));
#43541=DIRECTION('',(0.357406744336594,0.862856209461017,0.357406744336593));
#43542=DIRECTION('center_axis',(0.,-0.707106781186548,0.707106781186548));
#43543=DIRECTION('ref_axis',(0.,-0.707106781186548,-0.707106781186548));
#43544=DIRECTION('',(0.,0.707106781186548,0.707106781186548));
#43545=DIRECTION('',(-1.,0.,0.));
#43546=DIRECTION('',(0.,-0.707106781186548,-0.707106781186548));
#43547=DIRECTION('center_axis',(-0.707106781186548,-0.5,0.5));
#43548=DIRECTION('ref_axis',(0.577350269189625,0.,0.816496580927726));
#43549=DIRECTION('',(0.67859834454585,-0.281084637714835,0.678598344545838));
#43550=DIRECTION('',(0.,-0.707106781186548,-0.707106781186548));
#43551=DIRECTION('',(0.653281482438187,-0.191341716182544,0.732537816328743));
#43552=DIRECTION('center_axis',(-0.707106781186548,0.,0.707106781186548));
#43553=DIRECTION('ref_axis',(0.707106781186548,0.,0.707106781186548));
#43554=DIRECTION('',(0.,1.,0.));
#43555=DIRECTION('',(0.357406744336594,-0.862856209461017,0.357406744336594));
#43556=DIRECTION('',(0.678598344545847,0.281084637714822,0.678598344545847));
#43557=DIRECTION('',(0.,-1.,0.));
#43558=DIRECTION('center_axis',(0.573302186256021,0.313549377219833,0.756975158957757));
#43559=DIRECTION('ref_axis',(0.797175191421303,0.,-0.603748055220394));
#43560=DIRECTION('',(0.653281482438189,-0.732537816328742,-0.191341716182544));
#43561=DIRECTION('',(0.,0.923879532511287,-0.38268343236509));
#43562=DIRECTION('',(-0.653281482438193,-0.382683432365078,0.65328148243819));
#43563=DIRECTION('center_axis',(0.,0.38268343236509,0.923879532511287));
#43564=DIRECTION('ref_axis',(1.,0.,0.));
#43565=DIRECTION('',(1.,0.,0.));
#43566=DIRECTION('',(-1.,0.,0.));
#43567=DIRECTION('',(-0.357406744336593,-0.862856209461017,0.357406744336594));
#43568=DIRECTION('center_axis',(0.707106781186546,0.,0.707106781186549));
#43569=DIRECTION('ref_axis',(0.707106781186549,0.,-0.707106781186546));
#43570=DIRECTION('',(0.678598344545848,0.281084637714821,-0.678598344545845));
#43571=DIRECTION('',(0.,1.,0.));
#43572=DIRECTION('',(0.,-1.,0.));
#43573=DIRECTION('center_axis',(0.573302186256017,0.75697515895776,0.313549377219834));
#43574=DIRECTION('ref_axis',(0.479841491130335,0.,-0.87735519796136));
#43575=DIRECTION('',(0.65328148243819,-0.653281482438187,0.382683432365088));
#43576=DIRECTION('',(0.,0.38268343236509,-0.923879532511287));
#43577=DIRECTION('',(-0.653281482438189,0.191341716182544,0.732537816328742));
#43578=DIRECTION('center_axis',(0.,0.923879532511287,0.38268343236509));
#43579=DIRECTION('ref_axis',(0.,-0.38268343236509,0.923879532511287));
#43580=DIRECTION('',(0.357406744336592,-0.357406744336594,0.862856209461017));
#43581=DIRECTION('',(1.,0.,0.));
#43582=DIRECTION('',(-1.,0.,0.));
#43583=DIRECTION('',(-0.357406744336593,-0.357406744336593,0.862856209461017));
#43584=DIRECTION('center_axis',(0.707106781186547,0.500000000000001,0.500000000000001));
#43585=DIRECTION('ref_axis',(0.577350269189627,0.,-0.816496580927725));
#43586=DIRECTION('',(0.,0.707106781186548,-0.707106781186548));
#43587=DIRECTION('',(0.,-0.707106781186548,0.707106781186548));
#43588=DIRECTION('center_axis',(0.573302186256021,0.756975158957757,-0.313549377219833));
#43589=DIRECTION('ref_axis',(-0.479841491130332,0.,-0.877355197961361));
#43590=DIRECTION('',(0.653281482438189,-0.191341716182544,0.732537816328742));
#43591=DIRECTION('',(0.,-0.38268343236509,-0.923879532511287));
#43592=DIRECTION('',(-0.653281482438193,0.65328148243819,0.382683432365078));
#43593=DIRECTION('center_axis',(0.,0.923879532511287,-0.38268343236509));
#43594=DIRECTION('ref_axis',(0.,0.38268343236509,0.923879532511287));
#43595=DIRECTION('',(0.357406744336593,0.357406744336593,0.862856209461017));
#43596=DIRECTION('',(1.,0.,0.));
#43597=DIRECTION('',(-1.,0.,0.));
#43598=DIRECTION('',(-0.357406744336592,0.357406744336594,0.862856209461017));
#43599=DIRECTION('center_axis',(0.707106781186546,0.707106781186549,0.));
#43600=DIRECTION('ref_axis',(0.,0.,-1.));
#43601=DIRECTION('',(0.,0.,-1.));
#43602=DIRECTION('',(0.,0.,1.));
#43603=DIRECTION('center_axis',(0.573302186256017,0.313549377219834,-0.75697515895776));
#43604=DIRECTION('ref_axis',(-0.797175191421306,0.,-0.603748055220391));
#43605=DIRECTION('',(0.65328148243819,0.382683432365088,0.653281482438187));
#43606=DIRECTION('',(0.,-0.923879532511287,-0.38268343236509));
#43607=DIRECTION('',(-0.653281482438189,0.732537816328742,-0.191341716182544));
#43608=DIRECTION('center_axis',(0.,0.38268343236509,-0.923879532511287));
#43609=DIRECTION('ref_axis',(-1.,0.,0.));
#43610=DIRECTION('',(0.357406744336593,0.862856209461017,0.357406744336594));
#43611=DIRECTION('',(1.,0.,0.));
#43612=DIRECTION('',(-1.,0.,0.));
#43613=DIRECTION('',(-0.357406744336594,0.862856209461017,0.357406744336594));
#43614=DIRECTION('center_axis',(0.707106781186547,0.500000000000001,-0.500000000000001));
#43615=DIRECTION('ref_axis',(-0.577350269189627,0.,-0.816496580927725));
#43616=DIRECTION('',(0.,-0.707106781186548,-0.707106781186548));
#43617=DIRECTION('',(0.,0.707106781186548,0.707106781186548));
#43618=DIRECTION('center_axis',(0.573302186256021,-0.313549377219833,-0.756975158957757));
#43619=DIRECTION('ref_axis',(-0.797175191421303,0.,-0.603748055220394));
#43620=DIRECTION('',(0.653281482438189,0.732537816328742,0.191341716182544));
#43621=DIRECTION('',(0.,-0.923879532511287,0.38268343236509));
#43622=DIRECTION('',(-0.653281482438193,0.382683432365078,-0.65328148243819));
#43623=DIRECTION('center_axis',(0.,-0.38268343236509,-0.923879532511287));
#43624=DIRECTION('ref_axis',(-1.,0.,0.));
#43625=DIRECTION('',(0.357406744336594,0.862856209461017,-0.357406744336594));
#43626=DIRECTION('',(1.,0.,0.));
#43627=DIRECTION('',(-1.,0.,0.));
#43628=DIRECTION('',(-0.357406744336593,0.862856209461017,-0.357406744336594));
#43629=DIRECTION('center_axis',(0.707106781186546,0.,-0.707106781186549));
#43630=DIRECTION('ref_axis',(-0.707106781186549,0.,-0.707106781186546));
#43631=DIRECTION('',(0.,-1.,0.));
#43632=DIRECTION('',(0.,1.,0.));
#43633=DIRECTION('center_axis',(0.573302186256017,-0.75697515895776,-0.313549377219834));
#43634=DIRECTION('ref_axis',(-0.479841491130335,0.,-0.87735519796136));
#43635=DIRECTION('',(0.65328148243819,0.653281482438187,-0.382683432365088));
#43636=DIRECTION('',(0.,-0.38268343236509,0.923879532511287));
#43637=DIRECTION('',(-0.653281482438189,-0.191341716182544,-0.732537816328742));
#43638=DIRECTION('center_axis',(0.,-0.923879532511287,-0.38268343236509));
#43639=DIRECTION('ref_axis',(0.,0.38268343236509,-0.923879532511287));
#43640=DIRECTION('',(0.357406744336592,0.357406744336594,-0.862856209461017));
#43641=DIRECTION('',(1.,0.,0.));
#43642=DIRECTION('',(-1.,0.,0.));
#43643=DIRECTION('',(-0.357406744336593,0.357406744336593,-0.862856209461017));
#43644=DIRECTION('center_axis',(0.707106781186547,-0.500000000000001,-0.500000000000001));
#43645=DIRECTION('ref_axis',(-0.577350269189627,0.,-0.816496580927725));
#43646=DIRECTION('',(0.,-0.707106781186548,0.707106781186548));
#43647=DIRECTION('',(0.,0.707106781186548,-0.707106781186548));
#43648=DIRECTION('center_axis',(0.707106781186546,-0.707106781186549,0.));
#43649=DIRECTION('ref_axis',(0.,0.,-1.));
#43650=DIRECTION('',(-0.357406744336595,-0.357406744336593,-0.862856209461016));
#43651=DIRECTION('',(0.,0.,-1.));
#43652=DIRECTION('',(0.,0.,1.));
#43653=DIRECTION('',(-0.678598344545848,-0.678598344545845,0.281084637714821));
#43654=DIRECTION('center_axis',(-0.707106781186548,0.707106781186548,0.));
#43655=DIRECTION('ref_axis',(0.,0.,1.));
#43656=DIRECTION('',(0.678598344545847,0.678598344545847,-0.281084637714822));
#43657=DIRECTION('',(0.,0.,1.));
#43658=DIRECTION('',(0.67859834454585,0.678598344545838,0.281084637714835));
#43659=DIRECTION('',(0.,0.,-1.));
#43660=DIRECTION('center_axis',(0.,0.707106781186548,-0.707106781186548));
#43661=DIRECTION('ref_axis',(0.,0.707106781186548,0.707106781186548));
#43662=DIRECTION('',(0.,-0.707106781186548,-0.707106781186548));
#43663=DIRECTION('center_axis',(-0.707106781186548,0.5,-0.5));
#43664=DIRECTION('ref_axis',(-0.577350269189625,0.,0.816496580927726));
#43665=DIRECTION('',(0.67859834454585,0.281084637714835,-0.678598344545838));
#43666=DIRECTION('',(0.,0.707106781186548,0.707106781186548));
#43667=DIRECTION('center_axis',(0.,0.,-1.));
#43668=DIRECTION('ref_axis',(0.,1.,0.));
#43669=DIRECTION('',(0.,-1.,0.));
#43670=DIRECTION('center_axis',(-0.707106781186548,0.,-0.707106781186548));
#43671=DIRECTION('ref_axis',(-0.707106781186548,0.,0.707106781186548));
#43672=DIRECTION('',(0.678598344545847,-0.281084637714822,-0.678598344545847));
#43673=DIRECTION('',(0.,1.,0.));
#43674=DIRECTION('center_axis',(0.,-0.707106781186548,-0.707106781186548));
#43675=DIRECTION('ref_axis',(0.,0.707106781186548,-0.707106781186548));
#43676=DIRECTION('',(0.,-0.707106781186548,0.707106781186548));
#43677=DIRECTION('center_axis',(-0.707106781186548,-0.5,-0.5));
#43678=DIRECTION('ref_axis',(-0.577350269189625,0.,0.816496580927726));
#43679=DIRECTION('',(0.67859834454585,-0.678598344545838,-0.281084637714835));
#43680=DIRECTION('',(0.,0.707106781186548,-0.707106781186548));
#43681=DIRECTION('center_axis',(-0.707106781186548,-0.707106781186548,0.));
#43682=DIRECTION('ref_axis',(0.,0.,1.));
#43683=DIRECTION('',(0.,0.,1.));
#43684=DIRECTION('',(-0.653281482438189,0.653281482438189,0.382683432365089));
#43685=DIRECTION('',(0.,0.,-1.));
#43686=DIRECTION('center_axis',(0.,-1.,0.));
#43687=DIRECTION('ref_axis',(0.,0.,-1.));
#43688=DIRECTION('',(1.,0.,0.));
#43689=DIRECTION('center_axis',(0.,-0.923879532511287,0.38268343236509));
#43690=DIRECTION('ref_axis',(0.,-0.38268343236509,-0.923879532511287));
#43691=DIRECTION('',(-0.35740674433659,0.357406744336597,0.862856209461016));
#43692=DIRECTION('',(0.,-0.38268343236509,-0.923879532511287));
#43693=DIRECTION('center_axis',(1.,0.,0.));
#43694=DIRECTION('ref_axis',(0.,0.,-1.));
#43695=DIRECTION('center_axis',(1.,0.,0.));
#43696=DIRECTION('ref_axis',(0.,0.,-1.));
#43697=DIRECTION('',(-0.707106781186549,8.65956056235492E-17,-0.707106781186546));
#43698=DIRECTION('center_axis',(-1.,0.,0.));
#43699=DIRECTION('ref_axis',(0.,0.,-1.));
#43700=DIRECTION('center_axis',(1.,0.,0.));
#43701=DIRECTION('ref_axis',(0.,0.,-1.));
#43702=DIRECTION('',(0.,0.707106781186548,0.707106781186548));
#43703=DIRECTION('center_axis',(1.,0.,0.));
#43704=DIRECTION('ref_axis',(0.,0.,-1.));
#43705=DIRECTION('center_axis',(1.,0.,0.));
#43706=DIRECTION('ref_axis',(0.,0.,-1.));
#43707=DIRECTION('center_axis',(1.,0.,0.));
#43708=DIRECTION('ref_axis',(0.,0.,-1.));
#43709=DIRECTION('center_axis',(1.,0.,0.));
#43710=DIRECTION('ref_axis',(0.,0.,-1.));
#43711=DIRECTION('center_axis',(1.,0.,0.));
#43712=DIRECTION('ref_axis',(0.,0.,-1.));
#43713=DIRECTION('center_axis',(1.,0.,0.));
#43714=DIRECTION('ref_axis',(0.,0.,-1.));
#43715=DIRECTION('',(1.,0.,0.));
#43716=DIRECTION('center_axis',(1.,0.,0.));
#43717=DIRECTION('ref_axis',(0.,0.,-1.));
#43718=DIRECTION('',(-0.707106781186549,8.65956056235491E-17,-0.707106781186546));
#43719=DIRECTION('center_axis',(-1.,0.,0.));
#43720=DIRECTION('ref_axis',(0.,0.,-1.));
#43721=DIRECTION('center_axis',(1.,0.,0.));
#43722=DIRECTION('ref_axis',(0.,0.,-1.));
#43723=DIRECTION('center_axis',(1.,0.,0.));
#43724=DIRECTION('ref_axis',(0.,0.,-1.));
#43725=DIRECTION('',(1.,0.,0.));
#43726=DIRECTION('center_axis',(1.,0.,0.));
#43727=DIRECTION('ref_axis',(0.,0.,-1.));
#43728=DIRECTION('',(-0.707106781186549,8.65956056235491E-17,-0.707106781186546));
#43729=DIRECTION('center_axis',(-1.,0.,0.));
#43730=DIRECTION('ref_axis',(0.,0.,-1.));
#43731=DIRECTION('center_axis',(1.,0.,0.));
#43732=DIRECTION('ref_axis',(0.,0.,-1.));
#43733=DIRECTION('center_axis',(1.,0.,0.));
#43734=DIRECTION('ref_axis',(0.,0.,-1.));
#43735=DIRECTION('',(1.,0.,0.));
#43736=DIRECTION('center_axis',(1.,0.,0.));
#43737=DIRECTION('ref_axis',(0.,0.,-1.));
#43738=DIRECTION('',(-0.707106781186549,8.65956056235491E-17,-0.707106781186546));
#43739=DIRECTION('center_axis',(-1.,0.,0.));
#43740=DIRECTION('ref_axis',(0.,0.,-1.));
#43741=DIRECTION('center_axis',(1.,0.,0.));
#43742=DIRECTION('ref_axis',(0.,0.,-1.));
#43743=DIRECTION('center_axis',(1.,0.,0.));
#43744=DIRECTION('ref_axis',(0.,0.,-1.));
#43745=DIRECTION('',(1.,0.,0.));
#43746=DIRECTION('center_axis',(-1.,0.,0.));
#43747=DIRECTION('ref_axis',(0.,0.,-1.));
#43748=DIRECTION('center_axis',(-1.,0.,0.));
#43749=DIRECTION('ref_axis',(0.,0.,-1.));
#43750=DIRECTION('',(0.707106781186548,-8.65956056235493E-17,-0.707106781186548));
#43751=DIRECTION('center_axis',(1.,0.,0.));
#43752=DIRECTION('ref_axis',(0.,0.,-1.));
#43753=DIRECTION('',(0.,-0.707106781186548,0.707106781186548));
#43754=DIRECTION('center_axis',(-1.,0.,0.));
#43755=DIRECTION('ref_axis',(0.,0.,-1.));
#43756=DIRECTION('center_axis',(-1.,0.,0.));
#43757=DIRECTION('ref_axis',(0.,0.,-1.));
#43758=DIRECTION('center_axis',(-1.,0.,0.));
#43759=DIRECTION('ref_axis',(0.,1.,0.));
#43760=DIRECTION('center_axis',(-1.,0.,0.));
#43761=DIRECTION('ref_axis',(0.,0.,-1.));
#43762=DIRECTION('center_axis',(-1.,0.,0.));
#43763=DIRECTION('ref_axis',(0.,0.,-1.));
#43764=DIRECTION('',(0.707106781186548,-8.65956056235493E-17,-0.707106781186548));
#43765=DIRECTION('center_axis',(-1.,0.,0.));
#43766=DIRECTION('ref_axis',(0.,0.,-1.));
#43767=DIRECTION('',(0.707106781186548,-8.65956056235493E-17,-0.707106781186548));
#43768=DIRECTION('center_axis',(-1.,0.,0.));
#43769=DIRECTION('ref_axis',(0.,0.,-1.));
#43770=DIRECTION('',(0.707106781186547,-8.65956056235493E-17,-0.707106781186547));
#43771=DIRECTION('center_axis',(-0.707106781186548,0.5,0.5));
#43772=DIRECTION('ref_axis',(0.577350269189625,0.,0.816496580927726));
#43773=DIRECTION('',(0.,0.707106781186548,-0.707106781186548));
#43774=DIRECTION('center_axis',(-0.573302186256018,-0.756975158957759,0.313549377219833));
#43775=DIRECTION('ref_axis',(0.479841491130334,0.,0.87735519796136));
#43776=DIRECTION('center_axis',(0.707106781186547,-0.500000000000001,0.500000000000001));
#43777=DIRECTION('ref_axis',(0.577350269189627,0.,-0.816496580927725));
#43778=DIRECTION('center_axis',(0.,1.,0.));
#43779=DIRECTION('ref_axis',(0.,0.,1.));
#43780=DIRECTION('center_axis',(0.,0.707106781186548,0.707106781186548));
#43781=DIRECTION('ref_axis',(0.,-0.707106781186548,0.707106781186548));
#43782=DIRECTION('center_axis',(0.,0.,1.));
#43783=DIRECTION('ref_axis',(0.,-1.,0.));
#43784=DIRECTION('center_axis',(1.,0.,1.79678570832605E-15));
#43785=DIRECTION('ref_axis',(0.,-1.,-3.04015968733321E-17));
#43786=DIRECTION('center_axis',(-1.,0.,0.));
#43787=DIRECTION('ref_axis',(0.,-1.,0.));
#43788=DIRECTION('center_axis',(-1.,0.,0.));
#43789=DIRECTION('ref_axis',(0.,-1.,0.));
#43790=DIRECTION('',(-0.923879532511291,-0.382683432365078,-1.71851293172537E-15));
#43791=DIRECTION('center_axis',(1.,0.,0.));
#43792=DIRECTION('ref_axis',(0.,-1.,-6.12323399573677E-17));
#43793=DIRECTION('center_axis',(1.,0.,0.));
#43794=DIRECTION('ref_axis',(0.,-1.,-6.12323399573677E-17));
#43795=DIRECTION('center_axis',(1.,0.,0.));
#43796=DIRECTION('ref_axis',(0.,1.,0.));
#43797=DIRECTION('',(-0.707106781186548,0.707106781186548,8.65956056235493E-17));
#43798=DIRECTION('center_axis',(-1.,0.,0.));
#43799=DIRECTION('ref_axis',(0.,-1.,-6.12323399573677E-17));
#43800=DIRECTION('center_axis',(-1.,0.,0.));
#43801=DIRECTION('ref_axis',(0.,-1.,-6.12323399573677E-17));
#43802=DIRECTION('center_axis',(1.,0.,0.));
#43803=DIRECTION('ref_axis',(0.,1.,0.));
#43804=DIRECTION('',(-1.,0.,0.));
#43805=DIRECTION('center_axis',(1.,0.,-4.321736136636E-15));
#43806=DIRECTION('ref_axis',(0.,-1.,-3.11489047937176E-17));
#43807=DIRECTION('',(-0.382683432365088,-0.923879532511287,1.51193637171627E-15));
#43808=DIRECTION('center_axis',(1.,0.,0.));
#43809=DIRECTION('ref_axis',(0.,-1.,0.));
#43810=DIRECTION('center_axis',(-1.,0.,0.));
#43811=DIRECTION('ref_axis',(0.,0.,1.));
#43812=DIRECTION('center_axis',(1.,0.,0.));
#43813=DIRECTION('ref_axis',(0.,0.662617229149953,0.748958214878266));
#43814=DIRECTION('center_axis',(1.,0.,0.));
#43815=DIRECTION('ref_axis',(0.,1.,4.47017618667391E-14));
#43816=DIRECTION('center_axis',(-1.,0.,0.));
#43817=DIRECTION('ref_axis',(0.,1.,4.47017618667391E-14));
#43818=DIRECTION('center_axis',(1.,0.,0.));
#43819=DIRECTION('ref_axis',(0.,-0.999706152813195,-0.0242406276206029));
#43820=DIRECTION('center_axis',(1.,0.,0.));
#43821=DIRECTION('ref_axis',(0.,-0.999825056376581,0.0187044551261706));
#43822=DIRECTION('center_axis',(1.,0.,0.));
#43823=DIRECTION('ref_axis',(0.,1.,4.47017618667391E-14));
#43824=DIRECTION('center_axis',(1.,0.,0.));
#43825=DIRECTION('ref_axis',(0.,0.,-1.));
#43826=DIRECTION('center_axis',(-1.,0.,0.));
#43827=DIRECTION('ref_axis',(0.,1.,0.));
#43828=DIRECTION('center_axis',(-1.,0.,0.));
#43829=DIRECTION('ref_axis',(0.,1.,0.));
#43830=DIRECTION('center_axis',(1.,0.,0.));
#43831=DIRECTION('ref_axis',(0.,0.,-1.));
#43832=DIRECTION('',(0.,-1.,0.));
#43833=DIRECTION('center_axis',(1.,0.,0.));
#43834=DIRECTION('ref_axis',(0.,1.,0.));
#43835=DIRECTION('center_axis',(1.,0.,0.));
#43836=DIRECTION('ref_axis',(0.,1.,0.));
#43837=DIRECTION('center_axis',(1.,0.,0.));
#43838=DIRECTION('ref_axis',(0.,1.,0.));
#43839=DIRECTION('center_axis',(0.,0.,1.));
#43840=DIRECTION('ref_axis',(0.,1.,0.));
#43841=DIRECTION('center_axis',(0.,0.,-1.));
#43842=DIRECTION('ref_axis',(1.,0.,0.));
#43843=DIRECTION('',(-1.,0.,0.));
#43844=DIRECTION('center_axis',(0.,0.,1.));
#43845=DIRECTION('ref_axis',(0.,1.,0.));
#43846=DIRECTION('',(-1.,0.,0.));
#43847=DIRECTION('',(1.,0.,0.));
#43848=DIRECTION('center_axis',(0.,0.,1.));
#43849=DIRECTION('ref_axis',(0.,1.,0.));
#43850=DIRECTION('',(1.,0.,0.));
#43851=DIRECTION('',(-1.,0.,0.));
#43852=DIRECTION('center_axis',(0.,0.,1.));
#43853=DIRECTION('ref_axis',(0.,1.,0.));
#43854=DIRECTION('',(1.,0.,0.));
#43855=DIRECTION('',(-1.,0.,0.));
#43856=DIRECTION('center_axis',(0.,0.,1.));
#43857=DIRECTION('ref_axis',(0.,1.,0.));
#43858=DIRECTION('',(1.,0.,0.));
#43859=DIRECTION('',(-1.,0.,0.));
#43860=DIRECTION('center_axis',(0.,0.,1.));
#43861=DIRECTION('ref_axis',(0.,1.,0.));
#43862=DIRECTION('',(1.,0.,0.));
#43863=DIRECTION('',(-1.,0.,0.));
#43864=DIRECTION('center_axis',(0.,0.,1.));
#43865=DIRECTION('ref_axis',(0.,1.,0.));
#43866=DIRECTION('',(1.,0.,0.));
#43867=DIRECTION('',(-1.,0.,0.));
#43868=DIRECTION('center_axis',(0.,0.,1.));
#43869=DIRECTION('ref_axis',(0.,1.,0.));
#43870=DIRECTION('',(-1.,0.,0.));
#43871=DIRECTION('',(1.,0.,0.));
#43872=DIRECTION('center_axis',(0.,0.,1.));
#43873=DIRECTION('ref_axis',(0.,1.,0.));
#43874=DIRECTION('',(-1.,0.,0.));
#43875=DIRECTION('',(1.,0.,0.));
#43876=DIRECTION('center_axis',(0.,0.,1.));
#43877=DIRECTION('ref_axis',(0.,1.,0.));
#43878=DIRECTION('',(1.,0.,0.));
#43879=DIRECTION('',(-1.,0.,0.));
#43880=DIRECTION('center_axis',(0.,0.,1.));
#43881=DIRECTION('ref_axis',(0.,1.,0.));
#43882=DIRECTION('center_axis',(0.,0.,-1.));
#43883=DIRECTION('ref_axis',(1.,0.,0.));
#43884=DIRECTION('',(1.,0.,0.));
#43885=DIRECTION('',(-1.,0.,0.));
#43886=DIRECTION('center_axis',(1.,0.,0.));
#43887=DIRECTION('ref_axis',(0.,4.25719507862852E-15,1.));
#43888=DIRECTION('center_axis',(1.,0.,0.));
#43889=DIRECTION('ref_axis',(0.,-0.99996617381244,0.00822503683331852));
#43890=DIRECTION('center_axis',(1.,0.,0.));
#43891=DIRECTION('ref_axis',(0.,1.13626224362295E-14,1.));
#43892=DIRECTION('center_axis',(1.,0.,0.));
#43893=DIRECTION('ref_axis',(0.,1.40271576953299E-14,1.));
#43894=DIRECTION('center_axis',(-1.,0.,0.));
#43895=DIRECTION('ref_axis',(0.,1.,0.));
#43896=DIRECTION('center_axis',(1.,0.,0.));
#43897=DIRECTION('ref_axis',(0.,1.,0.));
#43898=DIRECTION('center_axis',(-1.,0.,0.));
#43899=DIRECTION('ref_axis',(0.,1.,0.));
#43900=DIRECTION('center_axis',(1.,0.,0.));
#43901=DIRECTION('ref_axis',(0.,1.,0.));
#43902=DIRECTION('center_axis',(1.,0.,0.));
#43903=DIRECTION('ref_axis',(0.,2.04893359930602E-14,1.));
#43904=DIRECTION('center_axis',(1.,0.,0.));
#43905=DIRECTION('ref_axis',(0.,1.1607551796059E-14,1.));
#43906=DIRECTION('center_axis',(1.,0.,0.));
#43907=DIRECTION('ref_axis',(0.,-1.59259792146449E-14,1.));
#43908=DIRECTION('center_axis',(1.,0.,0.));
#43909=DIRECTION('ref_axis',(0.,3.86969935969128E-14,1.));
#43910=DIRECTION('center_axis',(1.,0.,0.));
#43911=DIRECTION('ref_axis',(0.,-2.52518526214962E-14,1.));
#43912=DIRECTION('center_axis',(1.,0.,0.));
#43913=DIRECTION('ref_axis',(0.,-0.957484047746987,0.288486218579061));
#43914=DIRECTION('center_axis',(1.,0.,0.));
#43915=DIRECTION('ref_axis',(0.,1.,0.));
#43916=DIRECTION('center_axis',(1.,0.,0.));
#43917=DIRECTION('ref_axis',(0.,-1.08418380562736E-14,1.));
#43918=DIRECTION('center_axis',(1.,0.,0.));
#43919=DIRECTION('ref_axis',(0.,-0.999997956527064,-0.00202161858351363));
#43920=DIRECTION('center_axis',(0.,0.,-1.));
#43921=DIRECTION('ref_axis',(1.,0.,0.));
#43922=DIRECTION('',(0.,0.,-1.));
#43923=DIRECTION('center_axis',(-1.,0.,0.));
#43924=DIRECTION('ref_axis',(0.,1.,0.));
#43925=DIRECTION('center_axis',(1.,0.,0.));
#43926=DIRECTION('ref_axis',(0.,0.,-1.));
#43927=DIRECTION('',(-0.387484117215795,-0.921876379405339,-1.1289729572483E-16));
#43928=DIRECTION('center_axis',(1.,0.,0.));
#43929=DIRECTION('ref_axis',(0.,1.,0.));
#43930=DIRECTION('center_axis',(1.,0.,0.));
#43931=DIRECTION('ref_axis',(0.,0.,-1.));
#43932=DIRECTION('',(-1.,0.,0.));
#43933=DIRECTION('center_axis',(1.,0.,0.));
#43934=DIRECTION('ref_axis',(0.,0.,-1.));
#43935=DIRECTION('center_axis',(1.,0.,0.));
#43936=DIRECTION('ref_axis',(0.,0.,-1.));
#43937=DIRECTION('center_axis',(-1.,0.,0.));
#43938=DIRECTION('ref_axis',(0.,1.,0.));
#43939=DIRECTION('center_axis',(1.,0.,0.));
#43940=DIRECTION('ref_axis',(0.,0.,-1.));
#43941=DIRECTION('',(-0.707106781186547,-0.707106781186548,-8.65956056235494E-17));
#43942=DIRECTION('center_axis',(1.,0.,0.));
#43943=DIRECTION('ref_axis',(0.,1.,0.));
#43944=DIRECTION('center_axis',(1.,0.,0.));
#43945=DIRECTION('ref_axis',(0.,0.,-1.));
#43946=DIRECTION('',(-1.,0.,0.));
#43947=DIRECTION('center_axis',(-1.,0.,0.));
#43948=DIRECTION('ref_axis',(0.,1.,0.));
#43949=DIRECTION('center_axis',(1.,0.,0.));
#43950=DIRECTION('ref_axis',(0.,0.,-1.));
#43951=DIRECTION('',(-0.81923192051904,-0.573462344363328,-7.02288824456087E-17));
#43952=DIRECTION('center_axis',(-1.,0.,0.));
#43953=DIRECTION('ref_axis',(0.,1.,0.));
#43954=DIRECTION('center_axis',(1.,0.,0.));
#43955=DIRECTION('ref_axis',(0.,0.,-1.));
#43956=DIRECTION('',(-0.707106781186546,-0.707106781186549,-8.65956056235495E-17));
#43957=DIRECTION('center_axis',(-1.,0.,0.));
#43958=DIRECTION('ref_axis',(0.,0.,1.));
#43959=DIRECTION('center_axis',(-1.,0.,0.));
#43960=DIRECTION('ref_axis',(0.,1.,0.));
#43961=DIRECTION('',(0.,0.,-1.));
#43962=DIRECTION('',(0.,0.,1.));
#43963=DIRECTION('center_axis',(0.,-1.,0.));
#43964=DIRECTION('ref_axis',(0.,0.,1.));
#43965=DIRECTION('',(0.,0.,1.));
#43966=DIRECTION('',(1.,0.,0.));
#43967=DIRECTION('center_axis',(1.,0.,0.));
#43968=DIRECTION('ref_axis',(0.,1.,0.));
#43969=DIRECTION('',(-1.,0.,0.));
#43970=DIRECTION('center_axis',(1.,0.,0.));
#43971=DIRECTION('ref_axis',(0.,0.,-1.));
#43972=DIRECTION('',(-1.,0.,0.));
#43973=DIRECTION('center_axis',(1.,0.,0.));
#43974=DIRECTION('ref_axis',(0.,0.,-1.));
#43975=DIRECTION('center_axis',(0.,1.,0.));
#43976=DIRECTION('ref_axis',(0.,0.,-1.));
#43977=DIRECTION('',(0.,0.,-1.));
#43978=DIRECTION('center_axis',(1.,0.,0.));
#43979=DIRECTION('ref_axis',(0.,0.,-1.));
#43980=DIRECTION('center_axis',(1.,0.,0.));
#43981=DIRECTION('ref_axis',(0.,0.,-1.));
#43982=DIRECTION('center_axis',(1.,0.,0.));
#43983=DIRECTION('ref_axis',(0.,1.,0.));
#43984=DIRECTION('center_axis',(1.,0.,0.));
#43985=DIRECTION('ref_axis',(0.,0.,-1.));
#43986=DIRECTION('',(-1.,0.,0.));
#43987=DIRECTION('center_axis',(1.,0.,0.));
#43988=DIRECTION('ref_axis',(0.,1.,0.));
#43989=DIRECTION('',(-0.529998940003185,0.847998304005085,1.03849840868221E-16));
#43990=DIRECTION('center_axis',(-1.,0.,0.));
#43991=DIRECTION('ref_axis',(0.,1.,0.));
#43992=DIRECTION('',(-0.707106781186549,-0.707106781186546,-8.65956056235492E-17));
#43993=DIRECTION('center_axis',(0.,0.,1.));
#43994=DIRECTION('ref_axis',(0.,1.,0.));
#43995=DIRECTION('center_axis',(1.,0.,0.));
#43996=DIRECTION('ref_axis',(0.,1.,0.));
#43997=DIRECTION('axis',(0.,0.,1.));
#43998=DIRECTION('refdir',(1.,0.,0.));
#43999=DIRECTION('center_axis',(1.,0.,0.));
#44000=DIRECTION('ref_axis',(0.,-1.,0.));
#44001=DIRECTION('center_axis',(-1.,0.,0.));
#44002=DIRECTION('ref_axis',(0.,-1.,0.));
#44003=DIRECTION('center_axis',(-1.,0.,0.));
#44004=DIRECTION('ref_axis',(0.,-1.,0.));
#44005=DIRECTION('',(0.707106781186549,0.707106781186545,-8.65956056235491E-17));
#44006=DIRECTION('center_axis',(1.,0.,0.));
#44007=DIRECTION('ref_axis',(0.,-1.,0.));
#44008=DIRECTION('center_axis',(1.,0.,0.));
#44009=DIRECTION('ref_axis',(0.,0.,-1.));
#44010=DIRECTION('center_axis',(1.,0.,0.));
#44011=DIRECTION('ref_axis',(0.,0.,-1.));
#44012=DIRECTION('center_axis',(1.,0.,0.));
#44013=DIRECTION('ref_axis',(0.,1.,0.));
#44014=DIRECTION('',(-1.,0.,0.));
#44015=DIRECTION('center_axis',(1.,0.,0.));
#44016=DIRECTION('ref_axis',(0.,0.,-1.));
#44017=DIRECTION('center_axis',(-1.,0.,0.));
#44018=DIRECTION('ref_axis',(0.,-1.,0.));
#44019=DIRECTION('center_axis',(-1.,0.,0.));
#44020=DIRECTION('ref_axis',(0.,-1.,0.));
#44021=DIRECTION('',(0.707106781186549,-0.707106781186546,8.65956056235491E-17));
#44022=DIRECTION('center_axis',(1.,0.,0.));
#44023=DIRECTION('ref_axis',(0.,-1.,0.));
#44024=DIRECTION('center_axis',(1.,0.,0.));
#44025=DIRECTION('ref_axis',(0.,-1.,0.));
#44026=DIRECTION('center_axis',(-1.,0.,0.));
#44027=DIRECTION('ref_axis',(0.,0.,1.));
#44028=DIRECTION('center_axis',(1.,0.,0.));
#44029=DIRECTION('ref_axis',(0.,0.,-1.));
#44030=DIRECTION('center_axis',(1.,0.,0.));
#44031=DIRECTION('ref_axis',(0.,1.,0.));
#44032=DIRECTION('center_axis',(1.,0.,0.));
#44033=DIRECTION('ref_axis',(0.,0.,-1.));
#44034=DIRECTION('',(-1.,0.,0.));
#44035=DIRECTION('center_axis',(1.,0.,0.));
#44036=DIRECTION('ref_axis',(0.,0.,-1.));
#44037=DIRECTION('center_axis',(1.,0.,0.));
#44038=DIRECTION('ref_axis',(0.,0.,-1.));
#44039=DIRECTION('center_axis',(0.,1.,1.22464679914735E-16));
#44040=DIRECTION('ref_axis',(0.,-1.22464679914735E-16,1.));
#44041=DIRECTION('center_axis',(-1.,0.,0.));
#44042=DIRECTION('ref_axis',(0.,0.,-1.));
#44043=DIRECTION('center_axis',(-1.,0.,0.));
#44044=DIRECTION('ref_axis',(0.,0.,1.));
#44045=DIRECTION('center_axis',(1.,0.,0.));
#44046=DIRECTION('ref_axis',(0.,0.,-1.));
#44047=DIRECTION('center_axis',(1.,0.,0.));
#44048=DIRECTION('ref_axis',(0.,1.,0.));
#44049=DIRECTION('center_axis',(1.,0.,0.));
#44050=DIRECTION('ref_axis',(0.,0.,-1.));
#44051=DIRECTION('',(-0.707106781186547,0.707106781186548,8.65956056235494E-17));
#44052=DIRECTION('center_axis',(1.,0.,0.));
#44053=DIRECTION('ref_axis',(0.,1.,0.));
#44054=DIRECTION('center_axis',(1.,0.,0.));
#44055=DIRECTION('ref_axis',(0.,0.,-1.));
#44056=DIRECTION('',(-1.,0.,0.));
#44057=DIRECTION('center_axis',(-1.,0.,0.));
#44058=DIRECTION('ref_axis',(0.,1.,0.));
#44059=DIRECTION('',(-0.707106781186547,-0.707106781186547,-8.65956056235493E-17));
#44060=DIRECTION('center_axis',(1.,0.,0.));
#44061=DIRECTION('ref_axis',(0.,1.,0.));
#44062=DIRECTION('',(-0.853281833651959,0.521450009453976,6.38592084993168E-17));
#44063=DIRECTION('center_axis',(1.,0.,0.));
#44064=DIRECTION('ref_axis',(0.,0.,-1.));
#44065=DIRECTION('center_axis',(1.,0.,0.));
#44066=DIRECTION('ref_axis',(0.,1.,0.));
#44067=DIRECTION('',(-0.773128112524476,0.634249888943105,7.76732096353738E-17));
#44068=DIRECTION('center_axis',(1.,0.,0.));
#44069=DIRECTION('ref_axis',(0.,0.,-1.));
#44070=DIRECTION('center_axis',(1.,0.,0.));
#44071=DIRECTION('ref_axis',(0.,1.,0.));
#44072=DIRECTION('',(-1.,0.,0.));
#44073=DIRECTION('center_axis',(1.,0.,0.));
#44074=DIRECTION('ref_axis',(0.,0.,-1.));
#44075=DIRECTION('center_axis',(-1.,0.,0.));
#44076=DIRECTION('ref_axis',(0.,1.,0.));
#44077=DIRECTION('',(-0.695672465134814,-0.718359117192266,-8.79736193507827E-17));
#44078=DIRECTION('center_axis',(-1.,0.,0.));
#44079=DIRECTION('ref_axis',(0.,0.,1.));
#44080=DIRECTION('axis',(0.,0.,1.));
#44081=DIRECTION('refdir',(1.,0.,0.));
#44082=DIRECTION('center_axis',(1.,0.,0.));
#44083=DIRECTION('ref_axis',(0.,1.,0.));
#44084=DIRECTION('center_axis',(1.,0.,0.));
#44085=DIRECTION('ref_axis',(0.,0.,-1.));
#44086=DIRECTION('',(-0.707106781186547,0.707106781186548,8.65956056235494E-17));
#44087=DIRECTION('center_axis',(1.,0.,0.));
#44088=DIRECTION('ref_axis',(0.,0.,-1.));
#44089=DIRECTION('center_axis',(1.,0.,0.));
#44090=DIRECTION('ref_axis',(0.,1.,0.));
#44091=DIRECTION('center_axis',(1.,0.,0.));
#44092=DIRECTION('ref_axis',(0.,0.,-1.));
#44093=DIRECTION('',(-1.,0.,0.));
#44094=DIRECTION('center_axis',(-1.,0.,0.));
#44095=DIRECTION('ref_axis',(0.,1.,0.));
#44096=DIRECTION('center_axis',(1.,0.,0.));
#44097=DIRECTION('ref_axis',(0.,0.,-1.));
#44098=DIRECTION('',(-0.707106781186546,-0.707106781186549,-8.65956056235495E-17));
#44099=DIRECTION('center_axis',(1.,0.,0.));
#44100=DIRECTION('ref_axis',(0.,0.,-1.));
#44101=DIRECTION('center_axis',(1.,0.,0.));
#44102=DIRECTION('ref_axis',(0.,0.,-1.));
#44103=DIRECTION('center_axis',(1.,0.,0.));
#44104=DIRECTION('ref_axis',(0.,1.,0.));
#44105=DIRECTION('',(-0.707106781186545,0.70710678118655,8.65956056235497E-17));
#44106=DIRECTION('center_axis',(1.,0.,0.));
#44107=DIRECTION('ref_axis',(0.,0.,-1.));
#44108=DIRECTION('center_axis',(1.,0.,0.));
#44109=DIRECTION('ref_axis',(0.,1.,0.));
#44110=DIRECTION('',(-0.987688340595138,0.156434465040231,1.91576966887847E-17));
#44111=DIRECTION('center_axis',(1.,0.,0.));
#44112=DIRECTION('ref_axis',(0.,0.,-1.));
#44113=DIRECTION('center_axis',(-1.,0.,0.));
#44114=DIRECTION('ref_axis',(0.,1.,0.));
#44115=DIRECTION('',(-0.765095769134174,-0.643916503945182,-7.88570285474622E-17));
#44116=DIRECTION('center_axis',(1.,0.,0.));
#44117=DIRECTION('ref_axis',(0.,0.,-1.));
#44118=DIRECTION('center_axis',(-1.,0.,0.));
#44119=DIRECTION('ref_axis',(0.,0.,1.));
#44120=DIRECTION('axis',(0.,0.,1.));
#44121=DIRECTION('refdir',(1.,0.,0.));
#44122=DIRECTION('center_axis',(1.,0.,0.));
#44123=DIRECTION('ref_axis',(0.,-1.,0.));
#44124=DIRECTION('center_axis',(-1.,0.,0.));
#44125=DIRECTION('ref_axis',(0.,-1.,0.));
#44126=DIRECTION('center_axis',(-1.,0.,0.));
#44127=DIRECTION('ref_axis',(0.,-1.,0.));
#44128=DIRECTION('',(-0.707106781186549,-0.707106781186546,-8.65956056235491E-17));
#44129=DIRECTION('center_axis',(1.,0.,0.));
#44130=DIRECTION('ref_axis',(0.,-1.,0.));
#44131=DIRECTION('center_axis',(-1.,0.,0.));
#44132=DIRECTION('ref_axis',(0.,0.,1.));
#44133=DIRECTION('center_axis',(1.,0.,0.));
#44134=DIRECTION('ref_axis',(0.,0.,-1.));
#44135=DIRECTION('center_axis',(1.,0.,0.));
#44136=DIRECTION('ref_axis',(0.,1.,0.));
#44137=DIRECTION('center_axis',(1.,0.,0.));
#44138=DIRECTION('ref_axis',(0.,0.,-1.));
#44139=DIRECTION('',(-1.,0.,0.));
#44140=DIRECTION('center_axis',(-1.,0.,0.));
#44141=DIRECTION('ref_axis',(0.,-1.,0.));
#44142=DIRECTION('center_axis',(-1.,0.,0.));
#44143=DIRECTION('ref_axis',(0.,-1.,0.));
#44144=DIRECTION('',(-0.707106781186549,0.707106781186546,8.65956056235492E-17));
#44145=DIRECTION('center_axis',(1.,0.,0.));
#44146=DIRECTION('ref_axis',(0.,-1.,0.));
#44147=DIRECTION('center_axis',(1.,0.,0.));
#44148=DIRECTION('ref_axis',(0.,-1.,0.));
#44149=DIRECTION('center_axis',(1.,0.,0.));
#44150=DIRECTION('ref_axis',(0.,1.,0.));
#44151=DIRECTION('',(-1.,0.,0.));
#44152=DIRECTION('center_axis',(1.,0.,0.));
#44153=DIRECTION('ref_axis',(0.,0.,-1.));
#44154=DIRECTION('center_axis',(1.,0.,0.));
#44155=DIRECTION('ref_axis',(0.,0.,-1.));
#44156=DIRECTION('center_axis',(1.,0.,0.));
#44157=DIRECTION('ref_axis',(0.,0.,-1.));
#44158=DIRECTION('center_axis',(0.992546151641322,0.116932778696252,-0.0343345617181185));
#44159=DIRECTION('ref_axis',(0.,-0.28173255684143,-0.959492973614497));
#44160=DIRECTION('center_axis',(-0.992546151641322,-0.116932778696252,0.0343345617181191));
#44161=DIRECTION('ref_axis',(0.121869343405148,-0.952341058487958,0.279632565085031));
#44162=DIRECTION('center_axis',(0.121869343405148,-0.952341058487958,0.279632565085031));
#44163=DIRECTION('ref_axis',(0.,0.281732556841429,0.959492973614497));
#44164=DIRECTION('center_axis',(0.992546151641322,0.116932778696252,-0.0343345617181185));
#44165=DIRECTION('ref_axis',(0.121869343405148,-0.952341058487958,0.279632565085031));
#44166=DIRECTION('center_axis',(-0.992546151641322,-0.116932778696252,0.0343345617181191));
#44167=DIRECTION('ref_axis',(0.121869343405148,-0.952341058487958,0.279632565085031));
#44168=DIRECTION('center_axis',(0.992546151641322,0.116932778696252,-0.0343345617181185));
#44169=DIRECTION('ref_axis',(-0.121869343405146,0.952341058487958,-0.279632565085031));
#44170=DIRECTION('center_axis',(0.992546151641322,0.116932778696252,-0.0343345617181179));
#44171=DIRECTION('ref_axis',(0.121869343405148,-0.952341058487958,0.279632565085031));
#44172=DIRECTION('center_axis',(0.992546151641322,0.116932778696252,-0.0343345617181179));
#44173=DIRECTION('ref_axis',(0.121869343405148,-0.952341058487958,0.279632565085031));
#44174=DIRECTION('center_axis',(0.992546151641322,0.116932778696252,-0.0343345617181185));
#44175=DIRECTION('ref_axis',(0.,-0.28173255684143,-0.959492973614497));
#44176=DIRECTION('center_axis',(-0.992546151641322,-0.116932778696252,0.0343345617181185));
#44177=DIRECTION('ref_axis',(0.121869343405148,-0.952341058487958,0.279632565085031));
#44178=DIRECTION('center_axis',(0.121869343405148,-0.952341058487958,0.279632565085031));
#44179=DIRECTION('ref_axis',(0.,0.28173255684143,0.959492973614497));
#44180=DIRECTION('center_axis',(0.992546151641322,0.116932778696252,-0.0343345617181185));
#44181=DIRECTION('ref_axis',(0.,-0.28173255684143,-0.959492973614497));
#44182=DIRECTION('center_axis',(-0.992546151641322,-0.116932778696252,0.0343345617181185));
#44183=DIRECTION('ref_axis',(0.,0.28173255684143,0.959492973614497));
#44184=DIRECTION('center_axis',(0.992546151641322,0.102523015683397,-0.0658875414413361));
#44185=DIRECTION('ref_axis',(0.,-0.540640817455598,-0.841253532831181));
#44186=DIRECTION('center_axis',(-0.992546151641322,-0.102523015683397,0.0658875414413366));
#44187=DIRECTION('ref_axis',(0.121869343405148,-0.834982956566255,0.536610962785772));
#44188=DIRECTION('center_axis',(0.121869343405148,-0.834982956566256,0.536610962785772));
#44189=DIRECTION('ref_axis',(0.,0.540640817455598,0.841253532831181));
#44190=DIRECTION('center_axis',(0.992546151641322,0.102523015683397,-0.0658875414413361));
#44191=DIRECTION('ref_axis',(0.121869343405148,-0.834982956566255,0.536610962785772));
#44192=DIRECTION('center_axis',(-0.992546151641322,-0.102523015683397,0.0658875414413366));
#44193=DIRECTION('ref_axis',(0.121869343405148,-0.834982956566255,0.536610962785772));
#44194=DIRECTION('center_axis',(0.992546151641322,0.102523015683397,-0.0658875414413361));
#44195=DIRECTION('ref_axis',(-0.121869343405146,0.834982956566256,-0.536610962785772));
#44196=DIRECTION('center_axis',(0.992546151641322,0.102523015683398,-0.0658875414413355));
#44197=DIRECTION('ref_axis',(0.121869343405148,-0.834982956566256,0.536610962785772));
#44198=DIRECTION('center_axis',(0.992546151641322,0.102523015683398,-0.0658875414413355));
#44199=DIRECTION('ref_axis',(0.121869343405148,-0.834982956566256,0.536610962785772));
#44200=DIRECTION('center_axis',(0.992546151641322,0.102523015683397,-0.0658875414413361));
#44201=DIRECTION('ref_axis',(0.,-0.540640817455597,-0.841253532831181));
#44202=DIRECTION('center_axis',(-0.992546151641322,-0.102523015683397,0.0658875414413361));
#44203=DIRECTION('ref_axis',(0.121869343405148,-0.834982956566255,0.536610962785772));
#44204=DIRECTION('center_axis',(0.121869343405148,-0.834982956566256,0.536610962785772));
#44205=DIRECTION('ref_axis',(0.,0.540640817455597,0.841253532831181));
#44206=DIRECTION('center_axis',(0.992546151641322,0.102523015683397,-0.0658875414413361));
#44207=DIRECTION('ref_axis',(0.,-0.540640817455597,-0.841253532831181));
#44208=DIRECTION('center_axis',(-0.992546151641322,-0.102523015683397,0.0658875414413361));
#44209=DIRECTION('ref_axis',(0.,0.540640817455597,0.841253532831181));
#44210=DIRECTION('center_axis',(0.992546151641322,0.0798074476677251,-0.0921027044052734));
#44211=DIRECTION('ref_axis',(0.,-0.755749574354258,-0.654860733945285));
#44212=DIRECTION('center_axis',(-0.992546151641322,-0.0798074476677248,
0.0921027044052738));
#44213=DIRECTION('ref_axis',(0.121869343405148,-0.649979501338405,0.750116331629886));
#44214=DIRECTION('center_axis',(0.121869343405148,-0.649979501338405,0.750116331629886));
#44215=DIRECTION('ref_axis',(0.,0.755749574354258,0.654860733945286));
#44216=DIRECTION('center_axis',(0.992546151641322,0.0798074476677251,-0.0921027044052734));
#44217=DIRECTION('ref_axis',(0.121869343405148,-0.649979501338405,0.750116331629886));
#44218=DIRECTION('center_axis',(-0.992546151641322,-0.0798074476677248,
0.0921027044052738));
#44219=DIRECTION('ref_axis',(0.121869343405148,-0.649979501338405,0.750116331629886));
#44220=DIRECTION('center_axis',(0.992546151641322,0.0798074476677251,-0.0921027044052734));
#44221=DIRECTION('ref_axis',(-0.121869343405146,0.649979501338405,-0.750116331629886));
#44222=DIRECTION('center_axis',(0.992546151641322,0.0798074476677259,-0.092102704405273));
#44223=DIRECTION('ref_axis',(0.121869343405148,-0.649979501338404,0.750116331629886));
#44224=DIRECTION('center_axis',(0.992546151641322,0.0798074476677259,-0.092102704405273));
#44225=DIRECTION('ref_axis',(0.121869343405148,-0.649979501338404,0.750116331629886));
#44226=DIRECTION('center_axis',(0.992546151641322,0.0798074476677251,-0.0921027044052734));
#44227=DIRECTION('ref_axis',(0.,-0.755749574354258,-0.654860733945286));
#44228=DIRECTION('center_axis',(-0.992546151641322,-0.0798074476677251,
0.0921027044052734));
#44229=DIRECTION('ref_axis',(0.121869343405148,-0.649979501338405,0.750116331629886));
#44230=DIRECTION('center_axis',(0.121869343405148,-0.649979501338405,0.750116331629886));
#44231=DIRECTION('ref_axis',(0.,0.755749574354258,0.654860733945286));
#44232=DIRECTION('center_axis',(0.992546151641322,0.0798074476677251,-0.0921027044052734));
#44233=DIRECTION('ref_axis',(0.,-0.755749574354258,-0.654860733945285));
#44234=DIRECTION('center_axis',(-0.992546151641322,-0.0798074476677251,
0.0921027044052734));
#44235=DIRECTION('ref_axis',(0.,0.755749574354258,0.654860733945285));
#44236=DIRECTION('center_axis',(0.992546151641322,0.0506263548751808,-0.11085625401417));
#44237=DIRECTION('ref_axis',(0.,-0.909631995354518,-0.415415013001887));
#44238=DIRECTION('center_axis',(-0.992546151641322,-0.0506263548751804,
0.11085625401417));
#44239=DIRECTION('ref_axis',(0.121869343405148,-0.412318572489052,0.902851736398944));
#44240=DIRECTION('center_axis',(0.121869343405148,-0.412318572489052,0.902851736398944));
#44241=DIRECTION('ref_axis',(0.,0.909631995354519,0.415415013001886));
#44242=DIRECTION('center_axis',(0.992546151641322,0.0506263548751808,-0.11085625401417));
#44243=DIRECTION('ref_axis',(0.121869343405148,-0.412318572489052,0.902851736398944));
#44244=DIRECTION('center_axis',(-0.992546151641322,-0.0506263548751804,
0.11085625401417));
#44245=DIRECTION('ref_axis',(0.121869343405148,-0.412318572489052,0.902851736398944));
#44246=DIRECTION('center_axis',(0.992546151641322,0.0506263548751808,-0.11085625401417));
#44247=DIRECTION('ref_axis',(-0.121869343405146,0.412318572489052,-0.902851736398945));
#44248=DIRECTION('center_axis',(0.992546151641322,0.0506263548751816,-0.11085625401417));
#44249=DIRECTION('ref_axis',(0.121869343405148,-0.412318572489052,0.902851736398944));
#44250=DIRECTION('center_axis',(0.992546151641322,0.0506263548751816,-0.11085625401417));
#44251=DIRECTION('ref_axis',(0.121869343405148,-0.412318572489052,0.902851736398944));
#44252=DIRECTION('center_axis',(0.992546151641322,0.0506263548751808,-0.11085625401417));
#44253=DIRECTION('ref_axis',(0.,-0.909631995354518,-0.415415013001887));
#44254=DIRECTION('center_axis',(-0.992546151641322,-0.0506263548751808,
0.11085625401417));
#44255=DIRECTION('ref_axis',(0.121869343405148,-0.412318572489052,0.902851736398944));
#44256=DIRECTION('center_axis',(0.121869343405148,-0.412318572489052,0.902851736398944));
#44257=DIRECTION('ref_axis',(0.,0.909631995354519,0.415415013001886));
#44258=DIRECTION('center_axis',(0.992546151641322,0.0506263548751808,-0.11085625401417));
#44259=DIRECTION('ref_axis',(0.,-0.909631995354519,-0.415415013001886));
#44260=DIRECTION('center_axis',(-0.992546151641322,-0.0506263548751808,
0.11085625401417));
#44261=DIRECTION('ref_axis',(0.,0.909631995354519,0.415415013001886));
#44262=DIRECTION('center_axis',(0.992546151641322,0.017343815897175,-0.120628889210366));
#44263=DIRECTION('ref_axis',(0.,-0.989821441880933,-0.142314838273285));
#44264=DIRECTION('center_axis',(-0.992546151641322,-0.0173438158971745,
0.120628889210366));
#44265=DIRECTION('ref_axis',(0.121869343405148,-0.141254045049606,0.982443462950984));
#44266=DIRECTION('center_axis',(0.121869343405148,-0.141254045049607,0.982443462950984));
#44267=DIRECTION('ref_axis',(0.,0.989821441880933,0.142314838273285));
#44268=DIRECTION('center_axis',(0.992546151641322,0.017343815897175,-0.120628889210366));
#44269=DIRECTION('ref_axis',(0.121869343405148,-0.141254045049606,0.982443462950984));
#44270=DIRECTION('center_axis',(-0.992546151641322,-0.0173438158971745,
0.120628889210366));
#44271=DIRECTION('ref_axis',(0.121869343405148,-0.141254045049606,0.982443462950984));
#44272=DIRECTION('center_axis',(0.992546151641322,0.017343815897175,-0.120628889210366));
#44273=DIRECTION('ref_axis',(-0.121869343405146,0.141254045049606,-0.982443462950985));
#44274=DIRECTION('center_axis',(0.992546151641322,0.0173438158971758,-0.120628889210366));
#44275=DIRECTION('ref_axis',(0.121869343405148,-0.141254045049606,0.982443462950984));
#44276=DIRECTION('center_axis',(0.992546151641322,0.0173438158971758,-0.120628889210366));
#44277=DIRECTION('ref_axis',(0.121869343405148,-0.141254045049606,0.982443462950984));
#44278=DIRECTION('center_axis',(0.992546151641322,0.017343815897175,-0.120628889210366));
#44279=DIRECTION('ref_axis',(0.,-0.989821441880933,-0.142314838273284));
#44280=DIRECTION('center_axis',(-0.992546151641322,-0.017343815897175,0.120628889210366));
#44281=DIRECTION('ref_axis',(0.121869343405148,-0.141254045049606,0.982443462950984));
#44282=DIRECTION('center_axis',(0.121869343405148,-0.141254045049606,0.982443462950984));
#44283=DIRECTION('ref_axis',(0.,0.989821441880933,0.142314838273285));
#44284=DIRECTION('center_axis',(0.992546151641322,0.017343815897175,-0.120628889210366));
#44285=DIRECTION('ref_axis',(0.,-0.989821441880933,-0.142314838273285));
#44286=DIRECTION('center_axis',(-0.992546151641322,-0.017343815897175,0.120628889210366));
#44287=DIRECTION('ref_axis',(0.,0.989821441880933,0.142314838273285));
#44288=DIRECTION('center_axis',(0.992546151641322,-0.0173438158971751,-0.120628889210366));
#44289=DIRECTION('ref_axis',(0.,-0.989821441880933,0.142314838273285));
#44290=DIRECTION('center_axis',(-0.992546151641322,0.0173438158971756,0.120628889210366));
#44291=DIRECTION('ref_axis',(0.121869343405148,0.141254045049606,0.982443462950984));
#44292=DIRECTION('center_axis',(0.121869343405148,0.141254045049607,0.982443462950984));
#44293=DIRECTION('ref_axis',(0.,0.989821441880933,-0.142314838273285));
#44294=DIRECTION('center_axis',(0.992546151641322,-0.0173438158971751,-0.120628889210366));
#44295=DIRECTION('ref_axis',(0.121869343405148,0.141254045049606,0.982443462950984));
#44296=DIRECTION('center_axis',(-0.992546151641322,0.0173438158971756,0.120628889210366));
#44297=DIRECTION('ref_axis',(0.121869343405148,0.141254045049606,0.982443462950984));
#44298=DIRECTION('center_axis',(0.992546151641322,-0.0173438158971751,-0.120628889210366));
#44299=DIRECTION('ref_axis',(-0.121869343405146,-0.141254045049606,-0.982443462950985));
#44300=DIRECTION('center_axis',(0.992546151641322,-0.0173438158971743,-0.120628889210366));
#44301=DIRECTION('ref_axis',(0.121869343405148,0.141254045049606,0.982443462950984));
#44302=DIRECTION('center_axis',(0.992546151641322,-0.0173438158971743,-0.120628889210366));
#44303=DIRECTION('ref_axis',(0.121869343405148,0.141254045049606,0.982443462950984));
#44304=DIRECTION('center_axis',(0.992546151641322,-0.0173438158971751,-0.120628889210366));
#44305=DIRECTION('ref_axis',(0.,-0.989821441880933,0.142314838273286));
#44306=DIRECTION('center_axis',(-0.992546151641322,0.0173438158971751,0.120628889210366));
#44307=DIRECTION('ref_axis',(0.121869343405148,0.141254045049606,0.982443462950984));
#44308=DIRECTION('center_axis',(0.121869343405148,0.141254045049607,0.982443462950984));
#44309=DIRECTION('ref_axis',(0.,0.989821441880933,-0.142314838273285));
#44310=DIRECTION('center_axis',(0.992546151641322,-0.0173438158971751,-0.120628889210366));
#44311=DIRECTION('ref_axis',(0.,-0.989821441880933,0.142314838273285));
#44312=DIRECTION('center_axis',(-0.992546151641322,0.0173438158971751,0.120628889210366));
#44313=DIRECTION('ref_axis',(0.,0.989821441880933,-0.142314838273285));
#44314=DIRECTION('center_axis',(0.992546151641322,-0.0506263548751808,-0.11085625401417));
#44315=DIRECTION('ref_axis',(0.,-0.909631995354518,0.415415013001887));
#44316=DIRECTION('center_axis',(-0.992546151641322,0.0506263548751814,0.11085625401417));
#44317=DIRECTION('ref_axis',(0.121869343405148,0.412318572489052,0.902851736398944));
#44318=DIRECTION('center_axis',(0.121869343405148,0.412318572489052,0.902851736398944));
#44319=DIRECTION('ref_axis',(0.,0.909631995354519,-0.415415013001886));
#44320=DIRECTION('center_axis',(0.992546151641322,-0.0506263548751808,-0.11085625401417));
#44321=DIRECTION('ref_axis',(0.121869343405148,0.412318572489052,0.902851736398944));
#44322=DIRECTION('center_axis',(-0.992546151641322,0.0506263548751814,0.11085625401417));
#44323=DIRECTION('ref_axis',(0.121869343405148,0.412318572489052,0.902851736398944));
#44324=DIRECTION('center_axis',(0.992546151641322,-0.0506263548751808,-0.11085625401417));
#44325=DIRECTION('ref_axis',(-0.121869343405146,-0.412318572489052,-0.902851736398944));
#44326=DIRECTION('center_axis',(0.992546151641322,-0.0506263548751802,-0.11085625401417));
#44327=DIRECTION('ref_axis',(0.121869343405148,0.412318572489052,0.902851736398944));
#44328=DIRECTION('center_axis',(0.992546151641322,-0.0506263548751802,-0.11085625401417));
#44329=DIRECTION('ref_axis',(0.121869343405148,0.412318572489052,0.902851736398944));
#44330=DIRECTION('center_axis',(0.992546151641322,-0.0506263548751808,-0.11085625401417));
#44331=DIRECTION('ref_axis',(0.,-0.909631995354518,0.415415013001887));
#44332=DIRECTION('center_axis',(-0.992546151641322,0.0506263548751808,0.11085625401417));
#44333=DIRECTION('ref_axis',(0.121869343405148,0.412318572489052,0.902851736398944));
#44334=DIRECTION('center_axis',(0.121869343405148,0.412318572489052,0.902851736398944));
#44335=DIRECTION('ref_axis',(0.,0.909631995354519,-0.415415013001886));
#44336=DIRECTION('center_axis',(0.992546151641322,-0.0506263548751808,-0.11085625401417));
#44337=DIRECTION('ref_axis',(0.,-0.909631995354518,0.415415013001886));
#44338=DIRECTION('center_axis',(-0.992546151641322,0.0506263548751808,0.11085625401417));
#44339=DIRECTION('ref_axis',(0.,0.909631995354518,-0.415415013001886));
#44340=DIRECTION('center_axis',(0.992546151641322,-0.0798074476677251,-0.0921027044052734));
#44341=DIRECTION('ref_axis',(0.,-0.755749574354258,0.654860733945286));
#44342=DIRECTION('center_axis',(-0.992546151641322,0.0798074476677256,0.0921027044052731));
#44343=DIRECTION('ref_axis',(0.121869343405148,0.649979501338405,0.750116331629886));
#44344=DIRECTION('center_axis',(0.121869343405148,0.649979501338405,0.750116331629886));
#44345=DIRECTION('ref_axis',(0.,0.755749574354258,-0.654860733945286));
#44346=DIRECTION('center_axis',(0.992546151641322,-0.0798074476677251,-0.0921027044052734));
#44347=DIRECTION('ref_axis',(0.121869343405148,0.649979501338404,0.750116331629886));
#44348=DIRECTION('center_axis',(-0.992546151641322,0.0798074476677256,0.0921027044052731));
#44349=DIRECTION('ref_axis',(0.121869343405148,0.649979501338405,0.750116331629886));
#44350=DIRECTION('center_axis',(0.992546151641322,-0.0798074476677251,-0.0921027044052734));
#44351=DIRECTION('ref_axis',(-0.121869343405146,-0.649979501338405,-0.750116331629886));
#44352=DIRECTION('center_axis',(0.992546151641322,-0.0798074476677247,-0.092102704405274));
#44353=DIRECTION('ref_axis',(0.121869343405148,0.649979501338404,0.750116331629886));
#44354=DIRECTION('center_axis',(0.992546151641322,-0.0798074476677247,-0.092102704405274));
#44355=DIRECTION('ref_axis',(0.121869343405148,0.649979501338404,0.750116331629886));
#44356=DIRECTION('center_axis',(0.992546151641322,-0.0798074476677251,-0.0921027044052734));
#44357=DIRECTION('ref_axis',(0.,-0.755749574354258,0.654860733945286));
#44358=DIRECTION('center_axis',(-0.992546151641322,0.0798074476677251,0.0921027044052734));
#44359=DIRECTION('ref_axis',(0.121869343405148,0.649979501338404,0.750116331629886));
#44360=DIRECTION('center_axis',(0.121869343405148,0.649979501338404,0.750116331629886));
#44361=DIRECTION('ref_axis',(0.,0.755749574354258,-0.654860733945285));
#44362=DIRECTION('center_axis',(0.992546151641322,-0.0798074476677251,-0.0921027044052734));
#44363=DIRECTION('ref_axis',(0.,-0.755749574354258,0.654860733945285));
#44364=DIRECTION('center_axis',(-0.992546151641322,0.0798074476677251,0.0921027044052734));
#44365=DIRECTION('ref_axis',(0.,0.755749574354258,-0.654860733945285));
#44366=DIRECTION('center_axis',(0.992546151641322,-0.102523015683397,-0.0658875414413361));
#44367=DIRECTION('ref_axis',(0.,-0.540640817455598,0.841253532831181));
#44368=DIRECTION('center_axis',(-0.992546151641322,0.102523015683397,0.0658875414413357));
#44369=DIRECTION('ref_axis',(0.121869343405148,0.834982956566255,0.536610962785772));
#44370=DIRECTION('center_axis',(0.121869343405148,0.834982956566256,0.536610962785772));
#44371=DIRECTION('ref_axis',(0.,0.540640817455598,-0.841253532831181));
#44372=DIRECTION('center_axis',(0.992546151641322,-0.102523015683397,-0.0658875414413361));
#44373=DIRECTION('ref_axis',(0.121869343405148,0.834982956566256,0.536610962785772));
#44374=DIRECTION('center_axis',(-0.992546151641322,0.102523015683397,0.0658875414413357));
#44375=DIRECTION('ref_axis',(0.121869343405148,0.834982956566255,0.536610962785772));
#44376=DIRECTION('center_axis',(0.992546151641322,-0.102523015683397,-0.0658875414413361));
#44377=DIRECTION('ref_axis',(-0.121869343405146,-0.834982956566256,-0.536610962785772));
#44378=DIRECTION('center_axis',(0.992546151641322,-0.102523015683397,-0.0658875414413368));
#44379=DIRECTION('ref_axis',(0.121869343405148,0.834982956566255,0.536610962785772));
#44380=DIRECTION('center_axis',(0.992546151641322,-0.102523015683397,-0.0658875414413368));
#44381=DIRECTION('ref_axis',(0.121869343405148,0.834982956566255,0.536610962785772));
#44382=DIRECTION('center_axis',(0.992546151641322,-0.102523015683397,-0.0658875414413361));
#44383=DIRECTION('ref_axis',(0.,-0.540640817455598,0.841253532831181));
#44384=DIRECTION('center_axis',(-0.992546151641322,0.102523015683397,0.0658875414413361));
#44385=DIRECTION('ref_axis',(0.121869343405148,0.834982956566255,0.536610962785772));
#44386=DIRECTION('center_axis',(0.121869343405148,0.834982956566256,0.536610962785772));
#44387=DIRECTION('ref_axis',(0.,0.540640817455597,-0.841253532831181));
#44388=DIRECTION('center_axis',(0.992546151641322,-0.102523015683397,-0.0658875414413361));
#44389=DIRECTION('ref_axis',(0.,-0.540640817455598,0.841253532831181));
#44390=DIRECTION('center_axis',(-0.992546151641322,0.102523015683397,0.0658875414413361));
#44391=DIRECTION('ref_axis',(0.,0.540640817455598,-0.841253532831181));
#44392=DIRECTION('center_axis',(0.992546151641322,-0.116932778696252,-0.0343345617181185));
#44393=DIRECTION('ref_axis',(0.,-0.281732556841429,0.959492973614498));
#44394=DIRECTION('center_axis',(-0.992546151641322,0.116932778696252,0.034334561718118));
#44395=DIRECTION('ref_axis',(0.121869343405148,0.952341058487958,0.279632565085031));
#44396=DIRECTION('center_axis',(0.121869343405148,0.952341058487958,0.279632565085031));
#44397=DIRECTION('ref_axis',(0.,0.281732556841429,-0.959492973614497));
#44398=DIRECTION('center_axis',(0.992546151641322,-0.116932778696252,-0.0343345617181185));
#44399=DIRECTION('ref_axis',(0.121869343405148,0.952341058487958,0.279632565085031));
#44400=DIRECTION('center_axis',(-0.992546151641322,0.116932778696252,0.034334561718118));
#44401=DIRECTION('ref_axis',(0.121869343405148,0.952341058487958,0.279632565085031));
#44402=DIRECTION('center_axis',(0.992546151641322,-0.116932778696252,-0.0343345617181185));
#44403=DIRECTION('ref_axis',(-0.121869343405146,-0.952341058487958,-0.279632565085031));
#44404=DIRECTION('center_axis',(0.992546151641322,-0.116932778696252,-0.0343345617181193));
#44405=DIRECTION('ref_axis',(0.121869343405148,0.952341058487958,0.279632565085031));
#44406=DIRECTION('center_axis',(0.992546151641322,-0.116932778696252,-0.0343345617181193));
#44407=DIRECTION('ref_axis',(0.121869343405148,0.952341058487958,0.279632565085031));
#44408=DIRECTION('center_axis',(0.992546151641322,-0.116932778696252,-0.0343345617181185));
#44409=DIRECTION('ref_axis',(0.,-0.281732556841429,0.959492973614498));
#44410=DIRECTION('center_axis',(-0.992546151641322,0.116932778696252,0.0343345617181185));
#44411=DIRECTION('ref_axis',(0.121869343405148,0.952341058487958,0.279632565085031));
#44412=DIRECTION('center_axis',(0.121869343405148,0.952341058487958,0.279632565085031));
#44413=DIRECTION('ref_axis',(0.,0.28173255684143,-0.959492973614497));
#44414=DIRECTION('center_axis',(0.992546151641322,-0.116932778696252,-0.0343345617181185));
#44415=DIRECTION('ref_axis',(0.,-0.281732556841429,0.959492973614497));
#44416=DIRECTION('center_axis',(-0.992546151641322,0.116932778696252,0.0343345617181185));
#44417=DIRECTION('ref_axis',(0.,0.281732556841429,-0.959492973614497));
#44418=DIRECTION('center_axis',(0.992546151641322,-0.121869343405148,1.49246901315304E-17));
#44419=DIRECTION('ref_axis',(0.,0.,1.));
#44420=DIRECTION('center_axis',(-0.992546151641322,0.121869343405148,-5.59450180107848E-16));
#44421=DIRECTION('ref_axis',(0.121869343405148,0.992546151641322,-6.03195068039892E-17));
#44422=DIRECTION('center_axis',(0.121869343405148,0.992546151641322,0.));
#44423=DIRECTION('ref_axis',(0.,0.,-1.));
#44424=DIRECTION('center_axis',(0.992546151641322,-0.121869343405148,1.49246901315304E-17));
#44425=DIRECTION('ref_axis',(0.121869343405148,0.992546151641322,-1.21551846761357E-16));
#44426=DIRECTION('center_axis',(-0.992546151641322,0.121869343405148,-5.59450180107848E-16));
#44427=DIRECTION('ref_axis',(0.121869343405148,0.992546151641322,-6.03195068039892E-17));
#44428=DIRECTION('center_axis',(0.992546151641322,-0.121869343405148,1.49246901315304E-17));
#44429=DIRECTION('ref_axis',(-0.121869343405146,-0.992546151641322,1.21551846761357E-16));
#44430=DIRECTION('center_axis',(0.992546151641322,-0.121869343405148,-7.53073054377815E-16));
#44431=DIRECTION('ref_axis',(0.121869343405148,0.992546151641322,-6.03195068039892E-17));
#44432=DIRECTION('center_axis',(0.992546151641322,-0.121869343405148,-7.53073054377815E-16));
#44433=DIRECTION('ref_axis',(0.121869343405148,0.992546151641322,-6.03195068039892E-17));
#44434=DIRECTION('center_axis',(0.992546151641322,-0.121869343405148,1.49246901315304E-17));
#44435=DIRECTION('ref_axis',(0.,0.,1.));
#44436=DIRECTION('center_axis',(-0.992546151641322,0.121869343405148,-1.49246901315304E-17));
#44437=DIRECTION('ref_axis',(0.121869343405148,0.992546151641322,-1.21551846761357E-16));
#44438=DIRECTION('center_axis',(0.121869343405148,0.992546151641322,0.));
#44439=DIRECTION('ref_axis',(0.,0.,-1.));
#44440=DIRECTION('center_axis',(0.992546151641322,-0.121869343405148,1.49246901315304E-17));
#44441=DIRECTION('ref_axis',(0.,1.22464679914735E-16,1.));
#44442=DIRECTION('center_axis',(-0.992546151641322,0.121869343405148,-1.49246901315304E-17));
#44443=DIRECTION('ref_axis',(0.,-1.22464679914735E-16,-1.));
#44444=DIRECTION('center_axis',(0.992546151641322,-0.116932778696252,0.0343345617181185));
#44445=DIRECTION('ref_axis',(0.,0.281732556841431,0.959492973614497));
#44446=DIRECTION('center_axis',(-0.992546151641322,0.116932778696252,-0.0343345617181191));
#44447=DIRECTION('ref_axis',(0.121869343405148,0.952341058487958,-0.279632565085031));
#44448=DIRECTION('center_axis',(0.121869343405148,0.952341058487958,-0.279632565085031));
#44449=DIRECTION('ref_axis',(0.,-0.281732556841429,-0.959492973614497));
#44450=DIRECTION('center_axis',(0.992546151641322,-0.116932778696252,0.0343345617181185));
#44451=DIRECTION('ref_axis',(0.121869343405148,0.952341058487958,-0.279632565085031));
#44452=DIRECTION('center_axis',(-0.992546151641322,0.116932778696252,-0.0343345617181191));
#44453=DIRECTION('ref_axis',(0.121869343405148,0.952341058487958,-0.279632565085031));
#44454=DIRECTION('center_axis',(0.992546151641322,-0.116932778696252,0.0343345617181185));
#44455=DIRECTION('ref_axis',(-0.121869343405146,-0.952341058487958,0.279632565085031));
#44456=DIRECTION('center_axis',(0.992546151641322,-0.116932778696252,0.0343345617181179));
#44457=DIRECTION('ref_axis',(0.121869343405148,0.952341058487958,-0.279632565085031));
#44458=DIRECTION('center_axis',(0.992546151641322,-0.116932778696252,0.0343345617181179));
#44459=DIRECTION('ref_axis',(0.121869343405148,0.952341058487958,-0.279632565085031));
#44460=DIRECTION('center_axis',(0.992546151641322,-0.116932778696252,0.0343345617181185));
#44461=DIRECTION('ref_axis',(0.,0.28173255684143,0.959492973614497));
#44462=DIRECTION('center_axis',(-0.992546151641322,0.116932778696252,-0.0343345617181185));
#44463=DIRECTION('ref_axis',(0.121869343405148,0.952341058487958,-0.279632565085031));
#44464=DIRECTION('center_axis',(0.121869343405148,0.952341058487958,-0.279632565085031));
#44465=DIRECTION('ref_axis',(0.,-0.28173255684143,-0.959492973614497));
#44466=DIRECTION('center_axis',(0.992546151641322,-0.116932778696252,0.0343345617181185));
#44467=DIRECTION('ref_axis',(0.,0.28173255684143,0.959492973614497));
#44468=DIRECTION('center_axis',(-0.992546151641322,0.116932778696252,-0.0343345617181185));
#44469=DIRECTION('ref_axis',(0.,-0.28173255684143,-0.959492973614497));
#44470=DIRECTION('center_axis',(0.992546151641322,-0.102523015683397,0.0658875414413361));
#44471=DIRECTION('ref_axis',(0.,0.540640817455598,0.841253532831181));
#44472=DIRECTION('center_axis',(-0.992546151641322,0.102523015683397,-0.0658875414413366));
#44473=DIRECTION('ref_axis',(0.121869343405148,0.834982956566255,-0.536610962785772));
#44474=DIRECTION('center_axis',(0.121869343405148,0.834982956566256,-0.536610962785772));
#44475=DIRECTION('ref_axis',(0.,-0.540640817455598,-0.841253532831181));
#44476=DIRECTION('center_axis',(0.992546151641322,-0.102523015683397,0.0658875414413361));
#44477=DIRECTION('ref_axis',(0.121869343405148,0.834982956566255,-0.536610962785772));
#44478=DIRECTION('center_axis',(-0.992546151641322,0.102523015683397,-0.0658875414413366));
#44479=DIRECTION('ref_axis',(0.121869343405148,0.834982956566255,-0.536610962785772));
#44480=DIRECTION('center_axis',(0.992546151641322,-0.102523015683397,0.0658875414413361));
#44481=DIRECTION('ref_axis',(-0.121869343405146,-0.834982956566256,0.536610962785772));
#44482=DIRECTION('center_axis',(0.992546151641322,-0.102523015683398,0.0658875414413355));
#44483=DIRECTION('ref_axis',(0.121869343405148,0.834982956566255,-0.536610962785772));
#44484=DIRECTION('center_axis',(0.992546151641322,-0.102523015683398,0.0658875414413355));
#44485=DIRECTION('ref_axis',(0.121869343405148,0.834982956566255,-0.536610962785772));
#44486=DIRECTION('center_axis',(0.992546151641322,-0.102523015683397,0.0658875414413361));
#44487=DIRECTION('ref_axis',(0.,0.540640817455597,0.841253532831181));
#44488=DIRECTION('center_axis',(-0.992546151641322,0.102523015683397,-0.0658875414413361));
#44489=DIRECTION('ref_axis',(0.121869343405148,0.834982956566255,-0.536610962785772));
#44490=DIRECTION('center_axis',(0.121869343405148,0.834982956566256,-0.536610962785772));
#44491=DIRECTION('ref_axis',(0.,-0.540640817455597,-0.841253532831181));
#44492=DIRECTION('center_axis',(0.992546151641322,-0.102523015683397,0.0658875414413361));
#44493=DIRECTION('ref_axis',(0.,0.540640817455598,0.841253532831181));
#44494=DIRECTION('center_axis',(-0.992546151641322,0.102523015683397,-0.0658875414413361));
#44495=DIRECTION('ref_axis',(0.,-0.540640817455598,-0.841253532831181));
#44496=DIRECTION('center_axis',(0.992546151641322,-0.0798074476677251,0.0921027044052734));
#44497=DIRECTION('ref_axis',(0.,0.755749574354258,0.654860733945285));
#44498=DIRECTION('center_axis',(-0.992546151641322,0.0798074476677248,-0.0921027044052739));
#44499=DIRECTION('ref_axis',(0.121869343405148,0.649979501338404,-0.750116331629886));
#44500=DIRECTION('center_axis',(0.121869343405148,0.649979501338404,-0.750116331629886));
#44501=DIRECTION('ref_axis',(0.,-0.755749574354258,-0.654860733945285));
#44502=DIRECTION('center_axis',(0.992546151641322,-0.0798074476677251,0.0921027044052734));
#44503=DIRECTION('ref_axis',(0.121869343405148,0.649979501338404,-0.750116331629886));
#44504=DIRECTION('center_axis',(-0.992546151641322,0.0798074476677248,-0.0921027044052739));
#44505=DIRECTION('ref_axis',(0.121869343405148,0.649979501338404,-0.750116331629886));
#44506=DIRECTION('center_axis',(0.992546151641322,-0.0798074476677251,0.0921027044052734));
#44507=DIRECTION('ref_axis',(-0.121869343405146,-0.649979501338404,0.750116331629886));
#44508=DIRECTION('center_axis',(0.992546151641322,-0.0798074476677258,0.0921027044052731));
#44509=DIRECTION('ref_axis',(0.121869343405148,0.649979501338404,-0.750116331629886));
#44510=DIRECTION('center_axis',(0.992546151641322,-0.0798074476677258,0.0921027044052731));
#44511=DIRECTION('ref_axis',(0.121869343405148,0.649979501338404,-0.750116331629886));
#44512=DIRECTION('center_axis',(0.992546151641322,-0.0798074476677251,0.0921027044052734));
#44513=DIRECTION('ref_axis',(0.,0.755749574354258,0.654860733945285));
#44514=DIRECTION('center_axis',(-0.992546151641322,0.0798074476677251,-0.0921027044052734));
#44515=DIRECTION('ref_axis',(0.121869343405148,0.649979501338404,-0.750116331629886));
#44516=DIRECTION('center_axis',(0.121869343405148,0.649979501338404,-0.750116331629886));
#44517=DIRECTION('ref_axis',(0.,-0.755749574354258,-0.654860733945285));
#44518=DIRECTION('center_axis',(0.992546151641322,-0.0798074476677251,0.0921027044052734));
#44519=DIRECTION('ref_axis',(0.,0.755749574354258,0.654860733945285));
#44520=DIRECTION('center_axis',(-0.992546151641322,0.0798074476677251,-0.0921027044052734));
#44521=DIRECTION('ref_axis',(0.,-0.755749574354258,-0.654860733945285));
#44522=DIRECTION('center_axis',(0.992546151641322,-0.0506263548751808,0.11085625401417));
#44523=DIRECTION('ref_axis',(0.,0.909631995354518,0.415415013001887));
#44524=DIRECTION('center_axis',(-0.992546151641322,0.0506263548751804,-0.11085625401417));
#44525=DIRECTION('ref_axis',(0.121869343405148,0.412318572489052,-0.902851736398944));
#44526=DIRECTION('center_axis',(0.121869343405148,0.412318572489051,-0.902851736398945));
#44527=DIRECTION('ref_axis',(0.,-0.909631995354519,-0.415415013001886));
#44528=DIRECTION('center_axis',(0.992546151641322,-0.0506263548751808,0.11085625401417));
#44529=DIRECTION('ref_axis',(0.121869343405148,0.412318572489052,-0.902851736398944));
#44530=DIRECTION('center_axis',(-0.992546151641322,0.0506263548751804,-0.11085625401417));
#44531=DIRECTION('ref_axis',(0.121869343405148,0.412318572489052,-0.902851736398944));
#44532=DIRECTION('center_axis',(0.992546151641322,-0.0506263548751808,0.11085625401417));
#44533=DIRECTION('ref_axis',(-0.121869343405146,-0.412318572489052,0.902851736398944));
#44534=DIRECTION('center_axis',(0.992546151641322,-0.0506263548751816,0.11085625401417));
#44535=DIRECTION('ref_axis',(0.121869343405148,0.412318572489052,-0.902851736398944));
#44536=DIRECTION('center_axis',(0.992546151641322,-0.0506263548751816,0.11085625401417));
#44537=DIRECTION('ref_axis',(0.121869343405148,0.412318572489052,-0.902851736398944));
#44538=DIRECTION('center_axis',(0.992546151641322,-0.0506263548751808,0.11085625401417));
#44539=DIRECTION('ref_axis',(0.,0.909631995354518,0.415415013001887));
#44540=DIRECTION('center_axis',(-0.992546151641322,0.0506263548751808,-0.11085625401417));
#44541=DIRECTION('ref_axis',(0.121869343405148,0.412318572489052,-0.902851736398944));
#44542=DIRECTION('center_axis',(0.121869343405148,0.412318572489052,-0.902851736398944));
#44543=DIRECTION('ref_axis',(0.,-0.909631995354519,-0.415415013001886));
#44544=DIRECTION('center_axis',(0.992546151641322,-0.0506263548751808,0.11085625401417));
#44545=DIRECTION('ref_axis',(0.,0.909631995354519,0.415415013001886));
#44546=DIRECTION('center_axis',(-0.992546151641322,0.0506263548751808,-0.11085625401417));
#44547=DIRECTION('ref_axis',(0.,-0.909631995354519,-0.415415013001886));
#44548=DIRECTION('center_axis',(0.992546151641322,-0.017343815897175,0.120628889210366));
#44549=DIRECTION('ref_axis',(0.,0.989821441880933,0.142314838273285));
#44550=DIRECTION('center_axis',(-0.992546151641322,0.0173438158971745,-0.120628889210366));
#44551=DIRECTION('ref_axis',(0.121869343405148,0.141254045049606,-0.982443462950984));
#44552=DIRECTION('center_axis',(0.121869343405148,0.141254045049607,-0.982443462950984));
#44553=DIRECTION('ref_axis',(0.,-0.989821441880933,-0.142314838273285));
#44554=DIRECTION('center_axis',(0.992546151641322,-0.017343815897175,0.120628889210366));
#44555=DIRECTION('ref_axis',(0.121869343405148,0.141254045049606,-0.982443462950984));
#44556=DIRECTION('center_axis',(-0.992546151641322,0.0173438158971745,-0.120628889210366));
#44557=DIRECTION('ref_axis',(0.121869343405148,0.141254045049606,-0.982443462950984));
#44558=DIRECTION('center_axis',(0.992546151641322,-0.017343815897175,0.120628889210366));
#44559=DIRECTION('ref_axis',(-0.121869343405146,-0.141254045049606,0.982443462950985));
#44560=DIRECTION('center_axis',(0.992546151641322,-0.0173438158971758,0.120628889210366));
#44561=DIRECTION('ref_axis',(0.121869343405148,0.141254045049606,-0.982443462950984));
#44562=DIRECTION('center_axis',(0.992546151641322,-0.0173438158971758,0.120628889210366));
#44563=DIRECTION('ref_axis',(0.121869343405148,0.141254045049606,-0.982443462950984));
#44564=DIRECTION('center_axis',(0.992546151641322,-0.017343815897175,0.120628889210366));
#44565=DIRECTION('ref_axis',(0.,0.989821441880933,0.142314838273284));
#44566=DIRECTION('center_axis',(-0.992546151641322,0.017343815897175,-0.120628889210366));
#44567=DIRECTION('ref_axis',(0.121869343405148,0.141254045049606,-0.982443462950984));
#44568=DIRECTION('center_axis',(0.121869343405148,0.141254045049606,-0.982443462950984));
#44569=DIRECTION('ref_axis',(0.,-0.989821441880933,-0.142314838273285));
#44570=DIRECTION('center_axis',(0.992546151641322,-0.017343815897175,0.120628889210366));
#44571=DIRECTION('ref_axis',(0.,0.989821441880933,0.142314838273285));
#44572=DIRECTION('center_axis',(-0.992546151641322,0.017343815897175,-0.120628889210366));
#44573=DIRECTION('ref_axis',(0.,-0.989821441880933,-0.142314838273285));
#44574=DIRECTION('center_axis',(0.992546151641322,0.0173438158971751,0.120628889210366));
#44575=DIRECTION('ref_axis',(0.,0.989821441880933,-0.142314838273285));
#44576=DIRECTION('center_axis',(-0.992546151641322,-0.0173438158971756,
-0.120628889210366));
#44577=DIRECTION('ref_axis',(0.121869343405148,-0.141254045049606,-0.982443462950984));
#44578=DIRECTION('center_axis',(0.121869343405148,-0.141254045049607,-0.982443462950984));
#44579=DIRECTION('ref_axis',(0.,-0.989821441880933,0.142314838273285));
#44580=DIRECTION('center_axis',(0.992546151641322,0.0173438158971751,0.120628889210366));
#44581=DIRECTION('ref_axis',(0.121869343405148,-0.141254045049606,-0.982443462950984));
#44582=DIRECTION('center_axis',(-0.992546151641322,-0.0173438158971756,
-0.120628889210366));
#44583=DIRECTION('ref_axis',(0.121869343405148,-0.141254045049606,-0.982443462950984));
#44584=DIRECTION('center_axis',(0.992546151641322,0.0173438158971751,0.120628889210366));
#44585=DIRECTION('ref_axis',(-0.121869343405146,0.141254045049606,0.982443462950985));
#44586=DIRECTION('center_axis',(0.992546151641322,0.0173438158971743,0.120628889210366));
#44587=DIRECTION('ref_axis',(0.121869343405148,-0.141254045049606,-0.982443462950984));
#44588=DIRECTION('center_axis',(0.992546151641322,0.0173438158971743,0.120628889210366));
#44589=DIRECTION('ref_axis',(0.121869343405148,-0.141254045049606,-0.982443462950984));
#44590=DIRECTION('center_axis',(0.992546151641322,0.0173438158971751,0.120628889210366));
#44591=DIRECTION('ref_axis',(0.,0.989821441880933,-0.142314838273284));
#44592=DIRECTION('center_axis',(-0.992546151641322,-0.0173438158971751,
-0.120628889210366));
#44593=DIRECTION('ref_axis',(0.121869343405148,-0.141254045049606,-0.982443462950984));
#44594=DIRECTION('center_axis',(0.121869343405148,-0.141254045049606,-0.982443462950984));
#44595=DIRECTION('ref_axis',(0.,-0.989821441880933,0.142314838273285));
#44596=DIRECTION('center_axis',(0.992546151641322,0.0173438158971751,0.120628889210366));
#44597=DIRECTION('ref_axis',(0.,0.989821441880933,-0.142314838273285));
#44598=DIRECTION('center_axis',(-0.992546151641322,-0.0173438158971751,
-0.120628889210366));
#44599=DIRECTION('ref_axis',(0.,-0.989821441880933,0.142314838273285));
#44600=DIRECTION('center_axis',(0.992546151641322,0.0506263548751809,0.11085625401417));
#44601=DIRECTION('ref_axis',(0.,0.909631995354518,-0.415415013001887));
#44602=DIRECTION('center_axis',(-0.992546151641322,-0.0506263548751814,
-0.11085625401417));
#44603=DIRECTION('ref_axis',(0.121869343405148,-0.412318572489052,-0.902851736398944));
#44604=DIRECTION('center_axis',(0.121869343405148,-0.412318572489052,-0.902851736398944));
#44605=DIRECTION('ref_axis',(0.,-0.909631995354519,0.415415013001886));
#44606=DIRECTION('center_axis',(0.992546151641322,0.0506263548751809,0.11085625401417));
#44607=DIRECTION('ref_axis',(0.121869343405148,-0.412318572489052,-0.902851736398944));
#44608=DIRECTION('center_axis',(-0.992546151641322,-0.0506263548751814,
-0.11085625401417));
#44609=DIRECTION('ref_axis',(0.121869343405148,-0.412318572489052,-0.902851736398944));
#44610=DIRECTION('center_axis',(0.992546151641322,0.0506263548751809,0.11085625401417));
#44611=DIRECTION('ref_axis',(-0.121869343405146,0.412318572489052,0.902851736398944));
#44612=DIRECTION('center_axis',(0.992546151641322,0.0506263548751802,0.11085625401417));
#44613=DIRECTION('ref_axis',(0.121869343405148,-0.412318572489052,-0.902851736398944));
#44614=DIRECTION('center_axis',(0.992546151641322,0.0506263548751802,0.11085625401417));
#44615=DIRECTION('ref_axis',(0.121869343405148,-0.412318572489052,-0.902851736398944));
#44616=DIRECTION('center_axis',(0.992546151641322,0.0506263548751809,0.11085625401417));
#44617=DIRECTION('ref_axis',(0.,0.909631995354518,-0.415415013001887));
#44618=DIRECTION('center_axis',(-0.992546151641322,-0.0506263548751809,
-0.11085625401417));
#44619=DIRECTION('ref_axis',(0.121869343405148,-0.412318572489052,-0.902851736398944));
#44620=DIRECTION('center_axis',(0.121869343405148,-0.412318572489052,-0.902851736398944));
#44621=DIRECTION('ref_axis',(0.,-0.909631995354519,0.415415013001886));
#44622=DIRECTION('center_axis',(0.992546151641322,0.0506263548751809,0.11085625401417));
#44623=DIRECTION('ref_axis',(0.,0.909631995354518,-0.415415013001886));
#44624=DIRECTION('center_axis',(-0.992546151641322,-0.0506263548751809,
-0.11085625401417));
#44625=DIRECTION('ref_axis',(0.,-0.909631995354518,0.415415013001886));
#44626=DIRECTION('center_axis',(0.992546151641322,0.0798074476677251,0.0921027044052734));
#44627=DIRECTION('ref_axis',(0.,0.755749574354258,-0.654860733945286));
#44628=DIRECTION('center_axis',(-0.992546151641322,-0.0798074476677256,
-0.0921027044052731));
#44629=DIRECTION('ref_axis',(0.121869343405148,-0.649979501338404,-0.750116331629886));
#44630=DIRECTION('center_axis',(0.121869343405148,-0.649979501338404,-0.750116331629887));
#44631=DIRECTION('ref_axis',(0.,-0.755749574354259,0.654860733945285));
#44632=DIRECTION('center_axis',(0.992546151641322,0.0798074476677251,0.0921027044052734));
#44633=DIRECTION('ref_axis',(0.121869343405148,-0.649979501338404,-0.750116331629886));
#44634=DIRECTION('center_axis',(-0.992546151641322,-0.0798074476677256,
-0.0921027044052731));
#44635=DIRECTION('ref_axis',(0.121869343405148,-0.649979501338404,-0.750116331629886));
#44636=DIRECTION('center_axis',(0.992546151641322,0.0798074476677251,0.0921027044052734));
#44637=DIRECTION('ref_axis',(-0.121869343405146,0.649979501338405,0.750116331629886));
#44638=DIRECTION('center_axis',(0.992546151641322,0.0798074476677247,0.0921027044052741));
#44639=DIRECTION('ref_axis',(0.121869343405148,-0.649979501338404,-0.750116331629886));
#44640=DIRECTION('center_axis',(0.992546151641322,0.0798074476677247,0.0921027044052741));
#44641=DIRECTION('ref_axis',(0.121869343405148,-0.649979501338404,-0.750116331629886));
#44642=DIRECTION('center_axis',(0.992546151641322,0.0798074476677251,0.0921027044052734));
#44643=DIRECTION('ref_axis',(0.,0.755749574354258,-0.654860733945286));
#44644=DIRECTION('center_axis',(-0.992546151641322,-0.0798074476677251,
-0.0921027044052734));
#44645=DIRECTION('ref_axis',(0.121869343405148,-0.649979501338404,-0.750116331629886));
#44646=DIRECTION('center_axis',(0.121869343405148,-0.649979501338405,-0.750116331629886));
#44647=DIRECTION('ref_axis',(0.,-0.755749574354258,0.654860733945286));
#44648=DIRECTION('center_axis',(0.992546151641322,0.0798074476677251,0.0921027044052734));
#44649=DIRECTION('ref_axis',(0.,0.755749574354258,-0.654860733945285));
#44650=DIRECTION('center_axis',(-0.992546151641322,-0.0798074476677251,
-0.0921027044052734));
#44651=DIRECTION('ref_axis',(0.,-0.755749574354258,0.654860733945285));
#44652=DIRECTION('center_axis',(0.992546151641322,0.102523015683397,0.0658875414413361));
#44653=DIRECTION('ref_axis',(0.,0.540640817455598,-0.841253532831181));
#44654=DIRECTION('center_axis',(-0.992546151641322,-0.102523015683397,-0.0658875414413357));
#44655=DIRECTION('ref_axis',(0.121869343405148,-0.834982956566255,-0.536610962785772));
#44656=DIRECTION('center_axis',(0.121869343405148,-0.834982956566256,-0.536610962785772));
#44657=DIRECTION('ref_axis',(0.,-0.540640817455598,0.841253532831181));
#44658=DIRECTION('center_axis',(0.992546151641322,0.102523015683397,0.0658875414413361));
#44659=DIRECTION('ref_axis',(0.121869343405148,-0.834982956566256,-0.536610962785772));
#44660=DIRECTION('center_axis',(-0.992546151641322,-0.102523015683397,-0.0658875414413357));
#44661=DIRECTION('ref_axis',(0.121869343405148,-0.834982956566255,-0.536610962785772));
#44662=DIRECTION('center_axis',(0.992546151641322,0.102523015683397,0.0658875414413361));
#44663=DIRECTION('ref_axis',(-0.121869343405146,0.834982956566256,0.536610962785772));
#44664=DIRECTION('center_axis',(0.992546151641322,0.102523015683397,0.0658875414413368));
#44665=DIRECTION('ref_axis',(0.121869343405148,-0.834982956566255,-0.536610962785772));
#44666=DIRECTION('center_axis',(0.992546151641322,0.102523015683397,0.0658875414413368));
#44667=DIRECTION('ref_axis',(0.121869343405148,-0.834982956566255,-0.536610962785772));
#44668=DIRECTION('center_axis',(0.992546151641322,0.102523015683397,0.0658875414413361));
#44669=DIRECTION('ref_axis',(0.,0.540640817455598,-0.841253532831181));
#44670=DIRECTION('center_axis',(-0.992546151641322,-0.102523015683397,-0.0658875414413361));
#44671=DIRECTION('ref_axis',(0.121869343405148,-0.834982956566255,-0.536610962785772));
#44672=DIRECTION('center_axis',(0.121869343405148,-0.834982956566256,-0.536610962785772));
#44673=DIRECTION('ref_axis',(0.,-0.540640817455597,0.841253532831181));
#44674=DIRECTION('center_axis',(0.992546151641322,0.102523015683397,0.0658875414413361));
#44675=DIRECTION('ref_axis',(0.,0.540640817455598,-0.841253532831181));
#44676=DIRECTION('center_axis',(-0.992546151641322,-0.102523015683397,-0.0658875414413361));
#44677=DIRECTION('ref_axis',(0.,-0.540640817455598,0.841253532831181));
#44678=DIRECTION('center_axis',(0.992546151641322,0.116932778696252,0.0343345617181185));
#44679=DIRECTION('ref_axis',(0.,0.281732556841431,-0.959492973614497));
#44680=DIRECTION('center_axis',(-0.992546151641322,-0.116932778696252,-0.034334561718118));
#44681=DIRECTION('ref_axis',(0.121869343405148,-0.952341058487958,-0.279632565085031));
#44682=DIRECTION('center_axis',(0.121869343405148,-0.952341058487958,-0.279632565085031));
#44683=DIRECTION('ref_axis',(0.,-0.281732556841429,0.959492973614497));
#44684=DIRECTION('center_axis',(0.992546151641322,0.116932778696252,0.0343345617181185));
#44685=DIRECTION('ref_axis',(0.121869343405148,-0.952341058487958,-0.279632565085031));
#44686=DIRECTION('center_axis',(-0.992546151641322,-0.116932778696252,-0.034334561718118));
#44687=DIRECTION('ref_axis',(0.121869343405148,-0.952341058487958,-0.279632565085031));
#44688=DIRECTION('center_axis',(0.992546151641322,0.116932778696252,0.0343345617181185));
#44689=DIRECTION('ref_axis',(-0.121869343405146,0.952341058487958,0.279632565085031));
#44690=DIRECTION('center_axis',(0.992546151641322,0.116932778696252,0.0343345617181193));
#44691=DIRECTION('ref_axis',(0.121869343405148,-0.952341058487958,-0.279632565085031));
#44692=DIRECTION('center_axis',(0.992546151641322,0.116932778696252,0.0343345617181193));
#44693=DIRECTION('ref_axis',(0.121869343405148,-0.952341058487958,-0.279632565085031));
#44694=DIRECTION('center_axis',(0.992546151641322,0.116932778696252,0.0343345617181185));
#44695=DIRECTION('ref_axis',(0.,0.28173255684143,-0.959492973614497));
#44696=DIRECTION('center_axis',(-0.992546151641322,-0.116932778696252,-0.0343345617181185));
#44697=DIRECTION('ref_axis',(0.121869343405148,-0.952341058487958,-0.279632565085031));
#44698=DIRECTION('center_axis',(0.121869343405148,-0.952341058487958,-0.279632565085031));
#44699=DIRECTION('ref_axis',(0.,-0.28173255684143,0.959492973614497));
#44700=DIRECTION('center_axis',(0.992546151641322,0.116932778696252,0.0343345617181185));
#44701=DIRECTION('ref_axis',(0.,0.28173255684143,-0.959492973614497));
#44702=DIRECTION('center_axis',(-0.992546151641322,-0.116932778696252,-0.0343345617181185));
#44703=DIRECTION('ref_axis',(0.,-0.28173255684143,0.959492973614497));
#44704=DIRECTION('center_axis',(0.992546151641322,0.121869343405148,0.));
#44705=DIRECTION('ref_axis',(0.,0.,-1.));
#44706=DIRECTION('center_axis',(-0.992546151641322,-0.121869343405148,5.44525489976318E-16));
#44707=DIRECTION('ref_axis',(0.121869343405148,-0.992546151641322,-6.12323399573676E-17));
#44708=DIRECTION('center_axis',(0.121869343405148,-0.992546151641322,0.));
#44709=DIRECTION('ref_axis',(0.,0.,1.));
#44710=DIRECTION('center_axis',(0.992546151641322,0.121869343405148,0.));
#44711=DIRECTION('ref_axis',(0.121869343405148,-0.992546151641322,0.));
#44712=DIRECTION('center_axis',(-0.992546151641322,-0.121869343405148,5.44525489976318E-16));
#44713=DIRECTION('ref_axis',(0.121869343405148,-0.992546151641322,-6.12323399573676E-17));
#44714=DIRECTION('center_axis',(0.992546151641322,0.121869343405148,0.));
#44715=DIRECTION('ref_axis',(-0.121869343405146,0.992546151641322,0.));
#44716=DIRECTION('center_axis',(0.992546151641322,0.121869343405148,7.67997744509345E-16));
#44717=DIRECTION('ref_axis',(0.121869343405148,-0.992546151641322,-6.12323399573676E-17));
#44718=DIRECTION('center_axis',(0.992546151641322,0.121869343405148,7.67997744509345E-16));
#44719=DIRECTION('ref_axis',(0.121869343405148,-0.992546151641322,-6.12323399573676E-17));
#44720=DIRECTION('center_axis',(0.992546151641322,0.121869343405148,0.));
#44721=DIRECTION('ref_axis',(0.,0.,-1.));
#44722=DIRECTION('center_axis',(-0.992546151641322,-0.121869343405148,0.));
#44723=DIRECTION('ref_axis',(0.121869343405148,-0.992546151641322,0.));
#44724=DIRECTION('center_axis',(0.121869343405148,-0.992546151641322,0.));
#44725=DIRECTION('ref_axis',(0.,0.,1.));
#44726=DIRECTION('center_axis',(0.992546151641322,0.121869343405148,0.));
#44727=DIRECTION('ref_axis',(0.,0.,-1.));
#44728=DIRECTION('center_axis',(-0.992546151641322,-0.121869343405148,0.));
#44729=DIRECTION('ref_axis',(0.,0.,1.));
#44730=DIRECTION('center_axis',(1.,0.,0.));
#44731=DIRECTION('ref_axis',(0.,1.,0.));
#44732=DIRECTION('',(-0.707106781186551,0.707106781186544,8.65956056235489E-17));
#44733=DIRECTION('center_axis',(1.,0.,0.));
#44734=DIRECTION('ref_axis',(0.,0.,-1.));
#44735=DIRECTION('center_axis',(1.,0.,0.));
#44736=DIRECTION('ref_axis',(0.,1.,0.));
#44737=DIRECTION('',(-0.996194698091746,0.0871557427476584,1.0673500138323E-17));
#44738=DIRECTION('',(-0.996194698091746,0.0871557427476584,1.0673500138323E-17));
#44739=DIRECTION('center_axis',(-1.,0.,0.));
#44740=DIRECTION('ref_axis',(0.,1.,0.));
#44741=DIRECTION('center_axis',(1.,0.,0.));
#44742=DIRECTION('ref_axis',(0.,0.,-1.));
#44743=DIRECTION('',(-0.707106781186547,-0.707106781186547,-8.65956056235493E-17));
#44744=DIRECTION('center_axis',(1.,0.,0.));
#44745=DIRECTION('ref_axis',(0.,0.,-1.));
#44746=DIRECTION('center_axis',(1.,0.,0.));
#44747=DIRECTION('ref_axis',(0.,0.,-1.));
#44748=DIRECTION('center_axis',(1.,0.,0.));
#44749=DIRECTION('ref_axis',(0.,1.,0.));
#44750=DIRECTION('',(-0.707106781186547,0.707106781186547,8.65956056235493E-17));
#44751=DIRECTION('center_axis',(1.,0.,0.));
#44752=DIRECTION('ref_axis',(0.,0.,-1.));
#44753=DIRECTION('center_axis',(1.,0.,0.));
#44754=DIRECTION('ref_axis',(0.,1.,0.));
#44755=DIRECTION('',(-1.,0.,0.));
#44756=DIRECTION('center_axis',(1.,0.,0.));
#44757=DIRECTION('ref_axis',(0.,0.,-1.));
#44758=DIRECTION('center_axis',(-1.,0.,0.));
#44759=DIRECTION('ref_axis',(0.,1.,0.));
#44760=DIRECTION('',(-0.707106781186547,-0.707106781186548,-8.65956056235494E-17));
#44761=DIRECTION('center_axis',(1.,0.,0.));
#44762=DIRECTION('ref_axis',(0.,0.,-1.));
#44763=DIRECTION('center_axis',(-1.,0.,0.));
#44764=DIRECTION('ref_axis',(0.,0.,1.));
#44765=DIRECTION('axis',(0.,0.,1.));
#44766=DIRECTION('refdir',(1.,0.,0.));
#44767=DIRECTION('center_axis',(1.,0.,0.));
#44768=DIRECTION('ref_axis',(0.,1.,0.));
#44769=DIRECTION('center_axis',(1.,0.,0.));
#44770=DIRECTION('ref_axis',(0.,0.,-1.));
#44771=DIRECTION('',(-0.707106781186547,0.707106781186548,8.65956056235494E-17));
#44772=DIRECTION('center_axis',(1.,0.,0.));
#44773=DIRECTION('ref_axis',(0.,0.,-1.));
#44774=DIRECTION('center_axis',(1.,0.,0.));
#44775=DIRECTION('ref_axis',(0.,1.,0.));
#44776=DIRECTION('center_axis',(1.,0.,0.));
#44777=DIRECTION('ref_axis',(0.,0.,-1.));
#44778=DIRECTION('',(-1.,0.,0.));
#44779=DIRECTION('center_axis',(-1.,0.,0.));
#44780=DIRECTION('ref_axis',(0.,1.,0.));
#44781=DIRECTION('center_axis',(1.,0.,0.));
#44782=DIRECTION('ref_axis',(0.,0.,-1.));
#44783=DIRECTION('',(-0.707106781186548,-0.707106781186548,-8.65956056235493E-17));
#44784=DIRECTION('center_axis',(1.,0.,0.));
#44785=DIRECTION('ref_axis',(0.,0.,-1.));
#44786=DIRECTION('center_axis',(1.,0.,0.));
#44787=DIRECTION('ref_axis',(0.,0.,-1.));
#44788=DIRECTION('center_axis',(1.,0.,0.));
#44789=DIRECTION('ref_axis',(0.,1.,0.));
#44790=DIRECTION('',(-0.70710678118655,0.707106781186545,8.6595605623549E-17));
#44791=DIRECTION('center_axis',(1.,0.,0.));
#44792=DIRECTION('ref_axis',(0.,0.,-1.));
#44793=DIRECTION('center_axis',(1.,0.,0.));
#44794=DIRECTION('ref_axis',(0.,1.,0.));
#44795=DIRECTION('',(-0.987688340595138,0.156434465040231,1.91576966887847E-17));
#44796=DIRECTION('center_axis',(1.,0.,0.));
#44797=DIRECTION('ref_axis',(0.,0.,-1.));
#44798=DIRECTION('center_axis',(-1.,0.,0.));
#44799=DIRECTION('ref_axis',(0.,1.,0.));
#44800=DIRECTION('',(-0.765095769134171,-0.643916503945187,-7.88570285474627E-17));
#44801=DIRECTION('center_axis',(1.,0.,0.));
#44802=DIRECTION('ref_axis',(0.,0.,-1.));
#44803=DIRECTION('center_axis',(-1.,0.,0.));
#44804=DIRECTION('ref_axis',(0.,0.,1.));
#44805=DIRECTION('axis',(0.,0.,1.));
#44806=DIRECTION('refdir',(1.,0.,0.));
#44807=DIRECTION('center_axis',(1.,0.,0.));
#44808=DIRECTION('ref_axis',(0.,-1.,0.));
#44809=DIRECTION('center_axis',(-1.,0.,0.));
#44810=DIRECTION('ref_axis',(0.,-1.,0.));
#44811=DIRECTION('center_axis',(-1.,0.,0.));
#44812=DIRECTION('ref_axis',(0.,-1.,0.));
#44813=DIRECTION('',(-0.707106781186549,-0.707106781186546,-8.65956056235492E-17));
#44814=DIRECTION('center_axis',(1.,0.,0.));
#44815=DIRECTION('ref_axis',(0.,-1.,0.));
#44816=DIRECTION('center_axis',(-1.,0.,0.));
#44817=DIRECTION('ref_axis',(0.,0.,1.));
#44818=DIRECTION('center_axis',(1.,0.,0.));
#44819=DIRECTION('ref_axis',(0.,0.,-1.));
#44820=DIRECTION('center_axis',(1.,0.,0.));
#44821=DIRECTION('ref_axis',(0.,1.,0.));
#44822=DIRECTION('center_axis',(1.,0.,0.));
#44823=DIRECTION('ref_axis',(0.,0.,-1.));
#44824=DIRECTION('',(-1.,0.,0.));
#44825=DIRECTION('center_axis',(-1.,0.,0.));
#44826=DIRECTION('ref_axis',(0.,-1.,0.));
#44827=DIRECTION('center_axis',(-1.,0.,0.));
#44828=DIRECTION('ref_axis',(0.,-1.,0.));
#44829=DIRECTION('',(-0.707106781186547,0.707106781186548,8.65956056235494E-17));
#44830=DIRECTION('center_axis',(1.,0.,0.));
#44831=DIRECTION('ref_axis',(0.,-1.,0.));
#44832=DIRECTION('center_axis',(1.,0.,0.));
#44833=DIRECTION('ref_axis',(0.,-1.,0.));
#44834=DIRECTION('center_axis',(1.,0.,0.));
#44835=DIRECTION('ref_axis',(0.,1.,0.));
#44836=DIRECTION('',(-1.,0.,0.));
#44837=DIRECTION('center_axis',(1.,0.,0.));
#44838=DIRECTION('ref_axis',(0.,0.,-1.));
#44839=DIRECTION('center_axis',(1.,0.,0.));
#44840=DIRECTION('ref_axis',(0.,0.,-1.));
#44841=DIRECTION('center_axis',(1.,0.,0.));
#44842=DIRECTION('ref_axis',(0.,0.,-1.));
#44843=DIRECTION('center_axis',(0.992546151641322,0.115904633182077,-0.037659698205507));
#44844=DIRECTION('ref_axis',(0.,-0.309016994374948,-0.951056516295153));
#44845=DIRECTION('center_axis',(-0.992546151641322,-0.115904633182077,0.0376596982055071));
#44846=DIRECTION('ref_axis',(0.121869343405147,-0.943967485242157,0.306713628558622));
#44847=DIRECTION('center_axis',(0.121869343405148,-0.943967485242157,0.306713628558623));
#44848=DIRECTION('ref_axis',(0.,0.309016994374948,0.951056516295153));
#44849=DIRECTION('center_axis',(0.992546151641322,0.115904633182077,-0.037659698205507));
#44850=DIRECTION('ref_axis',(0.121869343405148,-0.943967485242157,0.306713628558622));
#44851=DIRECTION('center_axis',(-0.992546151641322,-0.115904633182077,0.0376596982055071));
#44852=DIRECTION('ref_axis',(0.121869343405147,-0.943967485242157,0.306713628558622));
#44853=DIRECTION('center_axis',(0.992546151641322,0.115904633182077,-0.037659698205507));
#44854=DIRECTION('ref_axis',(-0.121869343405147,0.943967485242157,-0.306713628558622));
#44855=DIRECTION('center_axis',(0.992546151641322,0.115904633182077,-0.0376596982055078));
#44856=DIRECTION('ref_axis',(0.121869343405148,-0.943967485242157,0.306713628558622));
#44857=DIRECTION('center_axis',(0.992546151641322,0.115904633182077,-0.0376596982055078));
#44858=DIRECTION('ref_axis',(0.121869343405148,-0.943967485242157,0.306713628558622));
#44859=DIRECTION('center_axis',(0.992546151641322,0.115904633182077,-0.037659698205507));
#44860=DIRECTION('ref_axis',(0.,-0.309016994374948,-0.951056516295154));
#44861=DIRECTION('center_axis',(-0.992546151641322,-0.115904633182077,0.037659698205507));
#44862=DIRECTION('ref_axis',(0.121869343405147,-0.943967485242157,0.306713628558622));
#44863=DIRECTION('center_axis',(0.121869343405148,-0.943967485242157,0.306713628558623));
#44864=DIRECTION('ref_axis',(0.,0.309016994374948,0.951056516295153));
#44865=DIRECTION('center_axis',(0.992546151641322,0.115904633182077,-0.037659698205507));
#44866=DIRECTION('ref_axis',(0.,-0.309016994374948,-0.951056516295153));
#44867=DIRECTION('center_axis',(-0.992546151641322,-0.115904633182077,0.037659698205507));
#44868=DIRECTION('ref_axis',(0.,0.309016994374948,0.951056516295153));
#44869=DIRECTION('center_axis',(0.992546151641322,0.0985943699080807,-0.0716330027601127));
#44870=DIRECTION('ref_axis',(0.,-0.587785252292474,-0.809016994374947));
#44871=DIRECTION('center_axis',(-0.992546151641322,-0.0985943699080806,
0.0716330027601127));
#44872=DIRECTION('ref_axis',(0.121869343405147,-0.802986704379283,0.583403990154418));
#44873=DIRECTION('center_axis',(0.121869343405148,-0.802986704379283,0.583403990154418));
#44874=DIRECTION('ref_axis',(0.,0.587785252292473,0.809016994374947));
#44875=DIRECTION('center_axis',(0.992546151641322,0.0985943699080807,-0.0716330027601127));
#44876=DIRECTION('ref_axis',(0.121869343405148,-0.802986704379283,0.583403990154418));
#44877=DIRECTION('center_axis',(-0.992546151641322,-0.0985943699080806,
0.0716330027601127));
#44878=DIRECTION('ref_axis',(0.121869343405147,-0.802986704379283,0.583403990154418));
#44879=DIRECTION('center_axis',(0.992546151641322,0.0985943699080807,-0.0716330027601127));
#44880=DIRECTION('ref_axis',(-0.121869343405147,0.802986704379283,-0.583403990154418));
#44881=DIRECTION('center_axis',(0.992546151641322,0.0985943699080803,-0.0716330027601134));
#44882=DIRECTION('ref_axis',(0.121869343405148,-0.802986704379283,0.583403990154418));
#44883=DIRECTION('center_axis',(0.992546151641322,0.0985943699080803,-0.0716330027601134));
#44884=DIRECTION('ref_axis',(0.121869343405148,-0.802986704379283,0.583403990154418));
#44885=DIRECTION('center_axis',(0.992546151641322,0.0985943699080807,-0.0716330027601127));
#44886=DIRECTION('ref_axis',(0.,-0.587785252292473,-0.809016994374947));
#44887=DIRECTION('center_axis',(-0.992546151641322,-0.0985943699080807,
0.0716330027601127));
#44888=DIRECTION('ref_axis',(0.121869343405147,-0.802986704379283,0.583403990154418));
#44889=DIRECTION('center_axis',(0.121869343405148,-0.802986704379283,0.583403990154418));
#44890=DIRECTION('ref_axis',(0.,0.587785252292473,0.809016994374948));
#44891=DIRECTION('center_axis',(0.992546151641322,0.0985943699080807,-0.0716330027601127));
#44892=DIRECTION('ref_axis',(0.,-0.587785252292473,-0.809016994374947));
#44893=DIRECTION('center_axis',(-0.992546151641322,-0.0985943699080807,
0.0716330027601127));
#44894=DIRECTION('ref_axis',(0.,0.587785252292473,0.809016994374947));
#44895=DIRECTION('center_axis',(0.992546151641322,0.0716330027601126,-0.0985943699080808));
#44896=DIRECTION('ref_axis',(0.,-0.809016994374947,-0.587785252292473));
#44897=DIRECTION('center_axis',(-0.992546151641322,-0.0716330027601125,
0.0985943699080807));
#44898=DIRECTION('ref_axis',(0.121869343405147,-0.583403990154418,0.802986704379283));
#44899=DIRECTION('center_axis',(0.121869343405147,-0.583403990154417,0.802986704379283));
#44900=DIRECTION('ref_axis',(0.,0.809016994374948,0.587785252292473));
#44901=DIRECTION('center_axis',(0.992546151641322,0.0716330027601126,-0.0985943699080808));
#44902=DIRECTION('ref_axis',(0.121869343405147,-0.583403990154418,0.802986704379283));
#44903=DIRECTION('center_axis',(-0.992546151641322,-0.0716330027601125,
0.0985943699080807));
#44904=DIRECTION('ref_axis',(0.121869343405147,-0.583403990154418,0.802986704379283));
#44905=DIRECTION('center_axis',(0.992546151641322,0.0716330027601126,-0.0985943699080808));
#44906=DIRECTION('ref_axis',(-0.121869343405147,0.583403990154418,-0.802986704379283));
#44907=DIRECTION('center_axis',(0.992546151641322,0.071633002760112,-0.0985943699080813));
#44908=DIRECTION('ref_axis',(0.121869343405148,-0.583403990154417,0.802986704379283));
#44909=DIRECTION('center_axis',(0.992546151641322,0.071633002760112,-0.0985943699080813));
#44910=DIRECTION('ref_axis',(0.121869343405148,-0.583403990154417,0.802986704379283));
#44911=DIRECTION('center_axis',(0.992546151641322,0.0716330027601126,-0.0985943699080808));
#44912=DIRECTION('ref_axis',(0.,-0.809016994374948,-0.587785252292473));
#44913=DIRECTION('center_axis',(-0.992546151641322,-0.0716330027601126,
0.0985943699080808));
#44914=DIRECTION('ref_axis',(0.121869343405147,-0.583403990154417,0.802986704379283));
#44915=DIRECTION('center_axis',(0.121869343405147,-0.583403990154418,0.802986704379283));
#44916=DIRECTION('ref_axis',(0.,0.809016994374948,0.587785252292473));
#44917=DIRECTION('center_axis',(0.992546151641322,0.0716330027601126,-0.0985943699080808));
#44918=DIRECTION('ref_axis',(0.,-0.809016994374948,-0.587785252292473));
#44919=DIRECTION('center_axis',(-0.992546151641322,-0.0716330027601126,
0.0985943699080808));
#44920=DIRECTION('ref_axis',(0.,0.809016994374948,0.587785252292473));
#44921=DIRECTION('center_axis',(0.992546151641322,0.037659698205507,-0.115904633182077));
#44922=DIRECTION('ref_axis',(0.,-0.951056516295153,-0.309016994374948));
#44923=DIRECTION('center_axis',(-0.992546151641322,-0.0376596982055068,
0.115904633182077));
#44924=DIRECTION('ref_axis',(0.121869343405147,-0.306713628558622,0.943967485242157));
#44925=DIRECTION('center_axis',(0.121869343405148,-0.306713628558622,0.943967485242157));
#44926=DIRECTION('ref_axis',(0.,0.951056516295154,0.309016994374947));
#44927=DIRECTION('center_axis',(0.992546151641322,0.037659698205507,-0.115904633182077));
#44928=DIRECTION('ref_axis',(0.121869343405148,-0.306713628558622,0.943967485242157));
#44929=DIRECTION('center_axis',(-0.992546151641322,-0.0376596982055068,
0.115904633182077));
#44930=DIRECTION('ref_axis',(0.121869343405147,-0.306713628558622,0.943967485242157));
#44931=DIRECTION('center_axis',(0.992546151641322,0.037659698205507,-0.115904633182077));
#44932=DIRECTION('ref_axis',(-0.121869343405147,0.306713628558622,-0.943967485242157));
#44933=DIRECTION('center_axis',(0.992546151641322,0.0376596982055062,-0.115904633182078));
#44934=DIRECTION('ref_axis',(0.121869343405148,-0.306713628558622,0.943967485242157));
#44935=DIRECTION('center_axis',(0.992546151641322,0.0376596982055062,-0.115904633182078));
#44936=DIRECTION('ref_axis',(0.121869343405148,-0.306713628558622,0.943967485242157));
#44937=DIRECTION('center_axis',(0.992546151641322,0.037659698205507,-0.115904633182077));
#44938=DIRECTION('ref_axis',(0.,-0.951056516295154,-0.309016994374948));
#44939=DIRECTION('center_axis',(-0.992546151641322,-0.037659698205507,0.115904633182077));
#44940=DIRECTION('ref_axis',(0.121869343405147,-0.306713628558622,0.943967485242157));
#44941=DIRECTION('center_axis',(0.121869343405147,-0.306713628558622,0.943967485242157));
#44942=DIRECTION('ref_axis',(0.,0.951056516295154,0.309016994374947));
#44943=DIRECTION('center_axis',(0.992546151641322,0.037659698205507,-0.115904633182077));
#44944=DIRECTION('ref_axis',(0.,-0.951056516295154,-0.309016994374947));
#44945=DIRECTION('center_axis',(-0.992546151641322,-0.037659698205507,0.115904633182077));
#44946=DIRECTION('ref_axis',(0.,0.951056516295154,0.309016994374947));
#44947=DIRECTION('center_axis',(0.992546151641322,-2.23870351972955E-17,
-0.121869343405147));
#44948=DIRECTION('ref_axis',(0.,-1.,0.));
#44949=DIRECTION('center_axis',(-0.992546151641322,1.39526782786796E-16,
0.121869343405147));
#44950=DIRECTION('ref_axis',(0.121869343405147,1.21095430184668E-16,0.992546151641322));
#44951=DIRECTION('center_axis',(0.121869343405147,0.,0.992546151641322));
#44952=DIRECTION('ref_axis',(0.,1.,0.));
#44953=DIRECTION('center_axis',(0.992546151641322,-2.23870351972955E-17,
-0.121869343405147));
#44954=DIRECTION('ref_axis',(0.121869343405148,1.82327770142035E-16,0.992546151641322));
#44955=DIRECTION('center_axis',(-0.992546151641322,1.39526782786796E-16,
0.121869343405147));
#44956=DIRECTION('ref_axis',(0.121869343405147,1.21095430184668E-16,0.992546151641322));
#44957=DIRECTION('center_axis',(0.992546151641322,-2.23870351972955E-17,
-0.121869343405147));
#44958=DIRECTION('ref_axis',(-0.121869343405147,-1.82327770142035E-16,-0.992546151641322));
#44959=DIRECTION('center_axis',(0.992546151641322,-8.54834401489946E-16,
-0.121869343405148));
#44960=DIRECTION('ref_axis',(0.121869343405148,1.21095430184668E-16,0.992546151641322));
#44961=DIRECTION('center_axis',(0.992546151641322,-8.54834401489946E-16,
-0.121869343405148));
#44962=DIRECTION('ref_axis',(0.121869343405148,1.21095430184668E-16,0.992546151641322));
#44963=DIRECTION('center_axis',(0.992546151641322,-2.23870351972955E-17,
-0.121869343405147));
#44964=DIRECTION('ref_axis',(0.,-1.,0.));
#44965=DIRECTION('center_axis',(-0.992546151641322,2.23870351972955E-17,
0.121869343405147));
#44966=DIRECTION('ref_axis',(0.121869343405147,1.82327770142035E-16,0.992546151641322));
#44967=DIRECTION('center_axis',(0.121869343405147,0.,0.992546151641322));
#44968=DIRECTION('ref_axis',(0.,1.,0.));
#44969=DIRECTION('center_axis',(0.992546151641322,-2.23870351972955E-17,
-0.121869343405147));
#44970=DIRECTION('ref_axis',(0.,-1.,1.83697019872103E-16));
#44971=DIRECTION('center_axis',(-0.992546151641322,2.23870351972955E-17,
0.121869343405147));
#44972=DIRECTION('ref_axis',(0.,1.,-1.83697019872103E-16));
#44973=DIRECTION('center_axis',(0.992546151641322,-0.037659698205507,-0.115904633182077));
#44974=DIRECTION('ref_axis',(0.,-0.951056516295153,0.309016994374948));
#44975=DIRECTION('center_axis',(-0.992546151641322,0.0376596982055071,0.115904633182077));
#44976=DIRECTION('ref_axis',(0.121869343405147,0.306713628558622,0.943967485242157));
#44977=DIRECTION('center_axis',(0.121869343405148,0.306713628558622,0.943967485242157));
#44978=DIRECTION('ref_axis',(0.,0.951056516295154,-0.309016994374947));
#44979=DIRECTION('center_axis',(0.992546151641322,-0.037659698205507,-0.115904633182077));
#44980=DIRECTION('ref_axis',(0.121869343405148,0.306713628558622,0.943967485242157));
#44981=DIRECTION('center_axis',(-0.992546151641322,0.0376596982055071,0.115904633182077));
#44982=DIRECTION('ref_axis',(0.121869343405147,0.306713628558622,0.943967485242157));
#44983=DIRECTION('center_axis',(0.992546151641322,-0.037659698205507,-0.115904633182077));
#44984=DIRECTION('ref_axis',(-0.121869343405147,-0.306713628558622,-0.943967485242157));
#44985=DIRECTION('center_axis',(0.992546151641322,-0.0376596982055078,-0.115904633182077));
#44986=DIRECTION('ref_axis',(0.121869343405148,0.306713628558622,0.943967485242157));
#44987=DIRECTION('center_axis',(0.992546151641322,-0.0376596982055078,-0.115904633182077));
#44988=DIRECTION('ref_axis',(0.121869343405148,0.306713628558622,0.943967485242157));
#44989=DIRECTION('center_axis',(0.992546151641322,-0.037659698205507,-0.115904633182077));
#44990=DIRECTION('ref_axis',(0.,-0.951056516295154,0.309016994374948));
#44991=DIRECTION('center_axis',(-0.992546151641322,0.037659698205507,0.115904633182077));
#44992=DIRECTION('ref_axis',(0.121869343405147,0.306713628558622,0.943967485242157));
#44993=DIRECTION('center_axis',(0.121869343405147,0.306713628558623,0.943967485242157));
#44994=DIRECTION('ref_axis',(0.,0.951056516295153,-0.309016994374948));
#44995=DIRECTION('center_axis',(0.992546151641322,-0.037659698205507,-0.115904633182077));
#44996=DIRECTION('ref_axis',(0.,-0.951056516295153,0.309016994374948));
#44997=DIRECTION('center_axis',(-0.992546151641322,0.037659698205507,0.115904633182077));
#44998=DIRECTION('ref_axis',(0.,0.951056516295153,-0.309016994374948));
#44999=DIRECTION('center_axis',(0.992546151641322,-0.0716330027601127,-0.0985943699080807));
#45000=DIRECTION('ref_axis',(0.,-0.809016994374947,0.587785252292473));
#45001=DIRECTION('center_axis',(-0.992546151641322,0.0716330027601127,0.0985943699080806));
#45002=DIRECTION('ref_axis',(0.121869343405147,0.583403990154418,0.802986704379283));
#45003=DIRECTION('center_axis',(0.121869343405148,0.583403990154418,0.802986704379283));
#45004=DIRECTION('ref_axis',(0.,0.809016994374947,-0.587785252292473));
#45005=DIRECTION('center_axis',(0.992546151641322,-0.0716330027601127,-0.0985943699080807));
#45006=DIRECTION('ref_axis',(0.121869343405148,0.583403990154418,0.802986704379283));
#45007=DIRECTION('center_axis',(-0.992546151641322,0.0716330027601127,0.0985943699080806));
#45008=DIRECTION('ref_axis',(0.121869343405147,0.583403990154418,0.802986704379283));
#45009=DIRECTION('center_axis',(0.992546151641322,-0.0716330027601127,-0.0985943699080807));
#45010=DIRECTION('ref_axis',(-0.121869343405147,-0.583403990154418,-0.802986704379283));
#45011=DIRECTION('center_axis',(0.992546151641322,-0.0716330027601134,-0.0985943699080803));
#45012=DIRECTION('ref_axis',(0.121869343405148,0.583403990154418,0.802986704379283));
#45013=DIRECTION('center_axis',(0.992546151641322,-0.0716330027601134,-0.0985943699080803));
#45014=DIRECTION('ref_axis',(0.121869343405148,0.583403990154418,0.802986704379283));
#45015=DIRECTION('center_axis',(0.992546151641322,-0.0716330027601127,-0.0985943699080807));
#45016=DIRECTION('ref_axis',(0.,-0.809016994374947,0.587785252292473));
#45017=DIRECTION('center_axis',(-0.992546151641322,0.0716330027601127,0.0985943699080807));
#45018=DIRECTION('ref_axis',(0.121869343405147,0.583403990154418,0.802986704379283));
#45019=DIRECTION('center_axis',(0.121869343405148,0.583403990154418,0.802986704379283));
#45020=DIRECTION('ref_axis',(0.,0.809016994374948,-0.587785252292473));
#45021=DIRECTION('center_axis',(0.992546151641322,-0.0716330027601127,-0.0985943699080807));
#45022=DIRECTION('ref_axis',(0.,-0.809016994374947,0.587785252292473));
#45023=DIRECTION('center_axis',(-0.992546151641322,0.0716330027601127,0.0985943699080807));
#45024=DIRECTION('ref_axis',(0.,0.809016994374947,-0.587785252292473));
#45025=DIRECTION('center_axis',(0.992546151641322,-0.0985943699080808,-0.0716330027601127));
#45026=DIRECTION('ref_axis',(0.,-0.587785252292473,0.809016994374947));
#45027=DIRECTION('center_axis',(-0.992546151641322,0.0985943699080807,0.0716330027601125));
#45028=DIRECTION('ref_axis',(0.121869343405147,0.802986704379283,0.583403990154418));
#45029=DIRECTION('center_axis',(0.121869343405148,0.802986704379283,0.583403990154418));
#45030=DIRECTION('ref_axis',(0.,0.587785252292473,-0.809016994374947));
#45031=DIRECTION('center_axis',(0.992546151641322,-0.0985943699080808,-0.0716330027601127));
#45032=DIRECTION('ref_axis',(0.121869343405147,0.802986704379283,0.583403990154418));
#45033=DIRECTION('center_axis',(-0.992546151641322,0.0985943699080807,0.0716330027601125));
#45034=DIRECTION('ref_axis',(0.121869343405147,0.802986704379283,0.583403990154418));
#45035=DIRECTION('center_axis',(0.992546151641322,-0.0985943699080808,-0.0716330027601127));
#45036=DIRECTION('ref_axis',(-0.121869343405147,-0.802986704379283,-0.583403990154418));
#45037=DIRECTION('center_axis',(0.992546151641322,-0.0985943699080813,-0.071633002760112));
#45038=DIRECTION('ref_axis',(0.121869343405148,0.802986704379283,0.583403990154418));
#45039=DIRECTION('center_axis',(0.992546151641322,-0.0985943699080813,-0.071633002760112));
#45040=DIRECTION('ref_axis',(0.121869343405148,0.802986704379283,0.583403990154418));
#45041=DIRECTION('center_axis',(0.992546151641322,-0.0985943699080808,-0.0716330027601127));
#45042=DIRECTION('ref_axis',(0.,-0.587785252292473,0.809016994374948));
#45043=DIRECTION('center_axis',(-0.992546151641322,0.0985943699080808,0.0716330027601127));
#45044=DIRECTION('ref_axis',(0.121869343405147,0.802986704379283,0.583403990154418));
#45045=DIRECTION('center_axis',(0.121869343405148,0.802986704379283,0.583403990154418));
#45046=DIRECTION('ref_axis',(0.,0.587785252292473,-0.809016994374948));
#45047=DIRECTION('center_axis',(0.992546151641322,-0.0985943699080808,-0.0716330027601127));
#45048=DIRECTION('ref_axis',(0.,-0.587785252292473,0.809016994374947));
#45049=DIRECTION('center_axis',(-0.992546151641322,0.0985943699080808,0.0716330027601127));
#45050=DIRECTION('ref_axis',(0.,0.587785252292473,-0.809016994374947));
#45051=DIRECTION('center_axis',(0.992546151641322,-0.115904633182077,-0.037659698205507));
#45052=DIRECTION('ref_axis',(0.,-0.309016994374948,0.951056516295153));
#45053=DIRECTION('center_axis',(-0.992546151641322,0.115904633182077,0.0376596982055068));
#45054=DIRECTION('ref_axis',(0.121869343405147,0.943967485242157,0.306713628558622));
#45055=DIRECTION('center_axis',(0.121869343405148,0.943967485242157,0.306713628558622));
#45056=DIRECTION('ref_axis',(0.,0.309016994374947,-0.951056516295154));
#45057=DIRECTION('center_axis',(0.992546151641322,-0.115904633182077,-0.037659698205507));
#45058=DIRECTION('ref_axis',(0.121869343405148,0.943967485242157,0.306713628558622));
#45059=DIRECTION('center_axis',(-0.992546151641322,0.115904633182077,0.0376596982055068));
#45060=DIRECTION('ref_axis',(0.121869343405147,0.943967485242157,0.306713628558622));
#45061=DIRECTION('center_axis',(0.992546151641322,-0.115904633182077,-0.037659698205507));
#45062=DIRECTION('ref_axis',(-0.121869343405147,-0.943967485242157,-0.306713628558622));
#45063=DIRECTION('center_axis',(0.992546151641322,-0.115904633182078,-0.0376596982055062));
#45064=DIRECTION('ref_axis',(0.121869343405148,0.943967485242157,0.306713628558622));
#45065=DIRECTION('center_axis',(0.992546151641322,-0.115904633182078,-0.0376596982055062));
#45066=DIRECTION('ref_axis',(0.121869343405148,0.943967485242157,0.306713628558622));
#45067=DIRECTION('center_axis',(0.992546151641322,-0.115904633182077,-0.037659698205507));
#45068=DIRECTION('ref_axis',(0.,-0.309016994374948,0.951056516295154));
#45069=DIRECTION('center_axis',(-0.992546151641322,0.115904633182077,0.037659698205507));
#45070=DIRECTION('ref_axis',(0.121869343405147,0.943967485242157,0.306713628558622));
#45071=DIRECTION('center_axis',(0.121869343405147,0.943967485242157,0.306713628558622));
#45072=DIRECTION('ref_axis',(0.,0.309016994374947,-0.951056516295154));
#45073=DIRECTION('center_axis',(0.992546151641322,-0.115904633182077,-0.037659698205507));
#45074=DIRECTION('ref_axis',(0.,-0.309016994374947,0.951056516295154));
#45075=DIRECTION('center_axis',(-0.992546151641322,0.115904633182077,0.037659698205507));
#45076=DIRECTION('ref_axis',(0.,0.309016994374947,-0.951056516295154));
#45077=DIRECTION('center_axis',(0.992546151641322,-0.121869343405147,1.49246901315303E-17));
#45078=DIRECTION('ref_axis',(0.,0.,1.));
#45079=DIRECTION('center_axis',(-0.992546151641322,0.121869343405147,-1.32064437721031E-16));
#45080=DIRECTION('ref_axis',(0.121869343405147,0.992546151641322,-6.03195068039891E-17));
#45081=DIRECTION('center_axis',(0.121869343405147,0.992546151641322,0.));
#45082=DIRECTION('ref_axis',(0.,0.,-1.));
#45083=DIRECTION('center_axis',(0.992546151641322,-0.121869343405147,1.49246901315303E-17));
#45084=DIRECTION('ref_axis',(0.121869343405148,0.992546151641322,-1.21551846761357E-16));
#45085=DIRECTION('center_axis',(-0.992546151641322,0.121869343405147,-1.32064437721031E-16));
#45086=DIRECTION('ref_axis',(0.121869343405147,0.992546151641322,-6.03195068039891E-17));
#45087=DIRECTION('center_axis',(0.992546151641322,-0.121869343405147,1.49246901315303E-17));
#45088=DIRECTION('ref_axis',(-0.121869343405147,-0.992546151641322,1.21551846761357E-16));
#45089=DIRECTION('center_axis',(0.992546151641322,-0.121869343405148,8.47372056424181E-16));
#45090=DIRECTION('ref_axis',(0.121869343405148,0.992546151641322,-6.03195068039891E-17));
#45091=DIRECTION('center_axis',(0.992546151641322,-0.121869343405148,8.47372056424181E-16));
#45092=DIRECTION('ref_axis',(0.121869343405148,0.992546151641322,-6.03195068039891E-17));
#45093=DIRECTION('center_axis',(0.992546151641322,-0.121869343405147,1.49246901315303E-17));
#45094=DIRECTION('ref_axis',(0.,0.,1.));
#45095=DIRECTION('center_axis',(-0.992546151641322,0.121869343405147,-1.49246901315303E-17));
#45096=DIRECTION('ref_axis',(0.121869343405147,0.992546151641322,-1.21551846761357E-16));
#45097=DIRECTION('center_axis',(0.121869343405147,0.992546151641322,0.));
#45098=DIRECTION('ref_axis',(0.,0.,-1.));
#45099=DIRECTION('center_axis',(0.992546151641322,-0.121869343405147,1.49246901315303E-17));
#45100=DIRECTION('ref_axis',(0.,1.22464679914735E-16,1.));
#45101=DIRECTION('center_axis',(-0.992546151641322,0.121869343405147,-1.49246901315303E-17));
#45102=DIRECTION('ref_axis',(0.,-1.22464679914735E-16,-1.));
#45103=DIRECTION('center_axis',(0.992546151641322,-0.115904633182077,0.037659698205507));
#45104=DIRECTION('ref_axis',(0.,0.309016994374948,0.951056516295153));
#45105=DIRECTION('center_axis',(-0.992546151641322,0.115904633182077,-0.0376596982055071));
#45106=DIRECTION('ref_axis',(0.121869343405147,0.943967485242157,-0.306713628558622));
#45107=DIRECTION('center_axis',(0.121869343405148,0.943967485242157,-0.306713628558622));
#45108=DIRECTION('ref_axis',(0.,-0.309016994374947,-0.951056516295154));
#45109=DIRECTION('center_axis',(0.992546151641322,-0.115904633182077,0.037659698205507));
#45110=DIRECTION('ref_axis',(0.121869343405148,0.943967485242157,-0.306713628558622));
#45111=DIRECTION('center_axis',(-0.992546151641322,0.115904633182077,-0.0376596982055071));
#45112=DIRECTION('ref_axis',(0.121869343405147,0.943967485242157,-0.306713628558622));
#45113=DIRECTION('center_axis',(0.992546151641322,-0.115904633182077,0.037659698205507));
#45114=DIRECTION('ref_axis',(-0.121869343405147,-0.943967485242157,0.306713628558622));
#45115=DIRECTION('center_axis',(0.992546151641322,-0.115904633182077,0.0376596982055078));
#45116=DIRECTION('ref_axis',(0.121869343405148,0.943967485242157,-0.306713628558622));
#45117=DIRECTION('center_axis',(0.992546151641322,-0.115904633182077,0.0376596982055078));
#45118=DIRECTION('ref_axis',(0.121869343405148,0.943967485242157,-0.306713628558622));
#45119=DIRECTION('center_axis',(0.992546151641322,-0.115904633182077,0.037659698205507));
#45120=DIRECTION('ref_axis',(0.,0.309016994374948,0.951056516295154));
#45121=DIRECTION('center_axis',(-0.992546151641322,0.115904633182077,-0.037659698205507));
#45122=DIRECTION('ref_axis',(0.121869343405147,0.943967485242157,-0.306713628558622));
#45123=DIRECTION('center_axis',(0.121869343405147,0.943967485242157,-0.306713628558623));
#45124=DIRECTION('ref_axis',(0.,-0.309016994374948,-0.951056516295153));
#45125=DIRECTION('center_axis',(0.992546151641322,-0.115904633182077,0.037659698205507));
#45126=DIRECTION('ref_axis',(0.,0.309016994374948,0.951056516295153));
#45127=DIRECTION('center_axis',(-0.992546151641322,0.115904633182077,-0.037659698205507));
#45128=DIRECTION('ref_axis',(0.,-0.309016994374948,-0.951056516295153));
#45129=DIRECTION('center_axis',(0.992546151641322,-0.0985943699080807,0.0716330027601127));
#45130=DIRECTION('ref_axis',(0.,0.587785252292473,0.809016994374947));
#45131=DIRECTION('center_axis',(-0.992546151641322,0.0985943699080806,-0.0716330027601127));
#45132=DIRECTION('ref_axis',(0.121869343405147,0.802986704379283,-0.583403990154418));
#45133=DIRECTION('center_axis',(0.121869343405148,0.802986704379283,-0.583403990154418));
#45134=DIRECTION('ref_axis',(0.,-0.587785252292473,-0.809016994374947));
#45135=DIRECTION('center_axis',(0.992546151641322,-0.0985943699080807,0.0716330027601127));
#45136=DIRECTION('ref_axis',(0.121869343405148,0.802986704379283,-0.583403990154418));
#45137=DIRECTION('center_axis',(-0.992546151641322,0.0985943699080806,-0.0716330027601127));
#45138=DIRECTION('ref_axis',(0.121869343405147,0.802986704379283,-0.583403990154418));
#45139=DIRECTION('center_axis',(0.992546151641322,-0.0985943699080807,0.0716330027601127));
#45140=DIRECTION('ref_axis',(-0.121869343405147,-0.802986704379283,0.583403990154418));
#45141=DIRECTION('center_axis',(0.992546151641322,-0.0985943699080803,0.0716330027601134));
#45142=DIRECTION('ref_axis',(0.121869343405148,0.802986704379283,-0.583403990154418));
#45143=DIRECTION('center_axis',(0.992546151641322,-0.0985943699080803,0.0716330027601134));
#45144=DIRECTION('ref_axis',(0.121869343405148,0.802986704379283,-0.583403990154418));
#45145=DIRECTION('center_axis',(0.992546151641322,-0.0985943699080807,0.0716330027601127));
#45146=DIRECTION('ref_axis',(0.,0.587785252292473,0.809016994374947));
#45147=DIRECTION('center_axis',(-0.992546151641322,0.0985943699080807,-0.0716330027601127));
#45148=DIRECTION('ref_axis',(0.121869343405147,0.802986704379283,-0.583403990154418));
#45149=DIRECTION('center_axis',(0.121869343405148,0.802986704379283,-0.583403990154418));
#45150=DIRECTION('ref_axis',(0.,-0.587785252292473,-0.809016994374948));
#45151=DIRECTION('center_axis',(0.992546151641322,-0.0985943699080807,0.0716330027601127));
#45152=DIRECTION('ref_axis',(0.,0.587785252292473,0.809016994374947));
#45153=DIRECTION('center_axis',(-0.992546151641322,0.0985943699080807,-0.0716330027601127));
#45154=DIRECTION('ref_axis',(0.,-0.587785252292473,-0.809016994374947));
#45155=DIRECTION('center_axis',(0.992546151641322,-0.0716330027601127,0.0985943699080808));
#45156=DIRECTION('ref_axis',(0.,0.809016994374947,0.587785252292473));
#45157=DIRECTION('center_axis',(-0.992546151641322,0.0716330027601125,-0.0985943699080807));
#45158=DIRECTION('ref_axis',(0.121869343405147,0.583403990154418,-0.802986704379283));
#45159=DIRECTION('center_axis',(0.121869343405148,0.583403990154418,-0.802986704379283));
#45160=DIRECTION('ref_axis',(0.,-0.809016994374947,-0.587785252292473));
#45161=DIRECTION('center_axis',(0.992546151641322,-0.0716330027601127,0.0985943699080808));
#45162=DIRECTION('ref_axis',(0.121869343405147,0.583403990154418,-0.802986704379283));
#45163=DIRECTION('center_axis',(-0.992546151641322,0.0716330027601125,-0.0985943699080807));
#45164=DIRECTION('ref_axis',(0.121869343405147,0.583403990154418,-0.802986704379283));
#45165=DIRECTION('center_axis',(0.992546151641322,-0.0716330027601127,0.0985943699080808));
#45166=DIRECTION('ref_axis',(-0.121869343405147,-0.583403990154418,0.802986704379283));
#45167=DIRECTION('center_axis',(0.992546151641322,-0.071633002760112,0.0985943699080813));
#45168=DIRECTION('ref_axis',(0.121869343405148,0.583403990154418,-0.802986704379283));
#45169=DIRECTION('center_axis',(0.992546151641322,-0.071633002760112,0.0985943699080813));
#45170=DIRECTION('ref_axis',(0.121869343405148,0.583403990154418,-0.802986704379283));
#45171=DIRECTION('center_axis',(0.992546151641322,-0.0716330027601127,0.0985943699080808));
#45172=DIRECTION('ref_axis',(0.,0.809016994374948,0.587785252292473));
#45173=DIRECTION('center_axis',(-0.992546151641322,0.0716330027601127,-0.0985943699080808));
#45174=DIRECTION('ref_axis',(0.121869343405147,0.583403990154418,-0.802986704379283));
#45175=DIRECTION('center_axis',(0.121869343405148,0.583403990154418,-0.802986704379283));
#45176=DIRECTION('ref_axis',(0.,-0.809016994374948,-0.587785252292473));
#45177=DIRECTION('center_axis',(0.992546151641322,-0.0716330027601127,0.0985943699080808));
#45178=DIRECTION('ref_axis',(0.,0.809016994374947,0.587785252292473));
#45179=DIRECTION('center_axis',(-0.992546151641322,0.0716330027601127,-0.0985943699080808));
#45180=DIRECTION('ref_axis',(0.,-0.809016994374947,-0.587785252292473));
#45181=DIRECTION('center_axis',(0.992546151641322,-0.037659698205507,0.115904633182077));
#45182=DIRECTION('ref_axis',(0.,0.951056516295153,0.309016994374948));
#45183=DIRECTION('center_axis',(-0.992546151641322,0.0376596982055068,-0.115904633182077));
#45184=DIRECTION('ref_axis',(0.121869343405147,0.306713628558622,-0.943967485242157));
#45185=DIRECTION('center_axis',(0.121869343405148,0.306713628558623,-0.943967485242157));
#45186=DIRECTION('ref_axis',(0.,-0.951056516295153,-0.309016994374948));
#45187=DIRECTION('center_axis',(0.992546151641322,-0.037659698205507,0.115904633182077));
#45188=DIRECTION('ref_axis',(0.121869343405148,0.306713628558622,-0.943967485242157));
#45189=DIRECTION('center_axis',(-0.992546151641322,0.0376596982055068,-0.115904633182077));
#45190=DIRECTION('ref_axis',(0.121869343405147,0.306713628558622,-0.943967485242157));
#45191=DIRECTION('center_axis',(0.992546151641322,-0.037659698205507,0.115904633182077));
#45192=DIRECTION('ref_axis',(-0.121869343405147,-0.306713628558622,0.943967485242157));
#45193=DIRECTION('center_axis',(0.992546151641322,-0.0376596982055062,0.115904633182078));
#45194=DIRECTION('ref_axis',(0.121869343405148,0.306713628558622,-0.943967485242157));
#45195=DIRECTION('center_axis',(0.992546151641322,-0.0376596982055062,0.115904633182078));
#45196=DIRECTION('ref_axis',(0.121869343405148,0.306713628558622,-0.943967485242157));
#45197=DIRECTION('center_axis',(0.992546151641322,-0.037659698205507,0.115904633182077));
#45198=DIRECTION('ref_axis',(0.,0.951056516295154,0.309016994374948));
#45199=DIRECTION('center_axis',(-0.992546151641322,0.037659698205507,-0.115904633182077));
#45200=DIRECTION('ref_axis',(0.121869343405147,0.306713628558622,-0.943967485242157));
#45201=DIRECTION('center_axis',(0.121869343405148,0.306713628558623,-0.943967485242157));
#45202=DIRECTION('ref_axis',(0.,-0.951056516295153,-0.309016994374948));
#45203=DIRECTION('center_axis',(0.992546151641322,-0.037659698205507,0.115904633182077));
#45204=DIRECTION('ref_axis',(0.,0.951056516295154,0.309016994374947));
#45205=DIRECTION('center_axis',(-0.992546151641322,0.037659698205507,-0.115904633182077));
#45206=DIRECTION('ref_axis',(0.,-0.951056516295154,-0.309016994374947));
#45207=DIRECTION('center_axis',(0.992546151641322,7.46234506576517E-18,
0.121869343405147));
#45208=DIRECTION('ref_axis',(0.,1.,0.));
#45209=DIRECTION('center_axis',(-0.992546151641322,-1.24602092655265E-16,
-0.121869343405147));
#45210=DIRECTION('ref_axis',(0.121869343405147,4.56416576689294E-19,-0.992546151641322));
#45211=DIRECTION('center_axis',(0.121869343405147,0.,-0.992546151641322));
#45212=DIRECTION('ref_axis',(0.,-1.,0.));
#45213=DIRECTION('center_axis',(0.992546151641322,7.46234506576517E-18,
0.121869343405147));
#45214=DIRECTION('ref_axis',(0.121869343405148,-6.07759233806784E-17,-0.992546151641322));
#45215=DIRECTION('center_axis',(-0.992546151641322,-1.24602092655265E-16,
-0.121869343405147));
#45216=DIRECTION('ref_axis',(0.121869343405147,4.56416576689294E-19,-0.992546151641322));
#45217=DIRECTION('center_axis',(0.992546151641322,7.46234506576517E-18,
0.121869343405147));
#45218=DIRECTION('ref_axis',(-0.121869343405147,6.07759233806784E-17,0.992546151641322));
#45219=DIRECTION('center_axis',(0.992546151641322,8.39909711358415E-16,
0.121869343405148));
#45220=DIRECTION('ref_axis',(0.121869343405148,4.56416576689272E-19,-0.992546151641322));
#45221=DIRECTION('center_axis',(0.992546151641322,8.39909711358415E-16,
0.121869343405148));
#45222=DIRECTION('ref_axis',(0.121869343405148,4.56416576689272E-19,-0.992546151641322));
#45223=DIRECTION('center_axis',(0.992546151641322,7.46234506576517E-18,
0.121869343405147));
#45224=DIRECTION('ref_axis',(0.,1.,0.));
#45225=DIRECTION('center_axis',(-0.992546151641322,-7.46234506576517E-18,
-0.121869343405147));
#45226=DIRECTION('ref_axis',(0.121869343405147,-6.07759233806784E-17,-0.992546151641322));
#45227=DIRECTION('center_axis',(0.121869343405147,0.,-0.992546151641322));
#45228=DIRECTION('ref_axis',(0.,-1.,0.));
#45229=DIRECTION('center_axis',(0.992546151641322,7.46234506576517E-18,
0.121869343405147));
#45230=DIRECTION('ref_axis',(0.,1.,-6.12323399573677E-17));
#45231=DIRECTION('center_axis',(-0.992546151641322,-7.46234506576517E-18,
-0.121869343405147));
#45232=DIRECTION('ref_axis',(0.,-1.,6.12323399573677E-17));
#45233=DIRECTION('center_axis',(0.992546151641322,0.037659698205507,0.115904633182077));
#45234=DIRECTION('ref_axis',(0.,0.951056516295154,-0.309016994374948));
#45235=DIRECTION('center_axis',(-0.992546151641322,-0.0376596982055071,
-0.115904633182077));
#45236=DIRECTION('ref_axis',(0.121869343405147,-0.306713628558622,-0.943967485242157));
#45237=DIRECTION('center_axis',(0.121869343405148,-0.306713628558622,-0.943967485242157));
#45238=DIRECTION('ref_axis',(0.,-0.951056516295154,0.309016994374947));
#45239=DIRECTION('center_axis',(0.992546151641322,0.037659698205507,0.115904633182077));
#45240=DIRECTION('ref_axis',(0.121869343405147,-0.306713628558622,-0.943967485242157));
#45241=DIRECTION('center_axis',(-0.992546151641322,-0.0376596982055071,
-0.115904633182077));
#45242=DIRECTION('ref_axis',(0.121869343405147,-0.306713628558622,-0.943967485242157));
#45243=DIRECTION('center_axis',(0.992546151641322,0.037659698205507,0.115904633182077));
#45244=DIRECTION('ref_axis',(-0.121869343405147,0.306713628558622,0.943967485242157));
#45245=DIRECTION('center_axis',(0.992546151641322,0.0376596982055078,0.115904633182077));
#45246=DIRECTION('ref_axis',(0.121869343405148,-0.306713628558622,-0.943967485242157));
#45247=DIRECTION('center_axis',(0.992546151641322,0.0376596982055078,0.115904633182077));
#45248=DIRECTION('ref_axis',(0.121869343405148,-0.306713628558622,-0.943967485242157));
#45249=DIRECTION('center_axis',(0.992546151641322,0.037659698205507,0.115904633182077));
#45250=DIRECTION('ref_axis',(0.,0.951056516295154,-0.309016994374948));
#45251=DIRECTION('center_axis',(-0.992546151641322,-0.037659698205507,-0.115904633182077));
#45252=DIRECTION('ref_axis',(0.121869343405147,-0.306713628558622,-0.943967485242157));
#45253=DIRECTION('center_axis',(0.121869343405148,-0.306713628558623,-0.943967485242157));
#45254=DIRECTION('ref_axis',(0.,-0.951056516295153,0.309016994374948));
#45255=DIRECTION('center_axis',(0.992546151641322,0.037659698205507,0.115904633182077));
#45256=DIRECTION('ref_axis',(0.,0.951056516295154,-0.309016994374948));
#45257=DIRECTION('center_axis',(-0.992546151641322,-0.037659698205507,-0.115904633182077));
#45258=DIRECTION('ref_axis',(0.,-0.951056516295154,0.309016994374948));
#45259=DIRECTION('center_axis',(0.992546151641322,0.0716330027601127,0.0985943699080808));
#45260=DIRECTION('ref_axis',(0.,0.809016994374947,-0.587785252292473));
#45261=DIRECTION('center_axis',(-0.992546151641322,-0.0716330027601127,
-0.0985943699080806));
#45262=DIRECTION('ref_axis',(0.121869343405147,-0.583403990154418,-0.802986704379283));
#45263=DIRECTION('center_axis',(0.121869343405147,-0.583403990154417,-0.802986704379283));
#45264=DIRECTION('ref_axis',(0.,-0.809016994374948,0.587785252292473));
#45265=DIRECTION('center_axis',(0.992546151641322,0.0716330027601127,0.0985943699080808));
#45266=DIRECTION('ref_axis',(0.121869343405148,-0.583403990154418,-0.802986704379283));
#45267=DIRECTION('center_axis',(-0.992546151641322,-0.0716330027601127,
-0.0985943699080806));
#45268=DIRECTION('ref_axis',(0.121869343405147,-0.583403990154418,-0.802986704379283));
#45269=DIRECTION('center_axis',(0.992546151641322,0.0716330027601127,0.0985943699080808));
#45270=DIRECTION('ref_axis',(-0.121869343405147,0.583403990154418,0.802986704379283));
#45271=DIRECTION('center_axis',(0.992546151641322,0.0716330027601134,0.0985943699080803));
#45272=DIRECTION('ref_axis',(0.121869343405148,-0.583403990154418,-0.802986704379283));
#45273=DIRECTION('center_axis',(0.992546151641322,0.0716330027601134,0.0985943699080803));
#45274=DIRECTION('ref_axis',(0.121869343405148,-0.583403990154418,-0.802986704379283));
#45275=DIRECTION('center_axis',(0.992546151641322,0.0716330027601127,0.0985943699080808));
#45276=DIRECTION('ref_axis',(0.,0.809016994374947,-0.587785252292473));
#45277=DIRECTION('center_axis',(-0.992546151641322,-0.0716330027601127,
-0.0985943699080808));
#45278=DIRECTION('ref_axis',(0.121869343405147,-0.583403990154418,-0.802986704379283));
#45279=DIRECTION('center_axis',(0.121869343405148,-0.583403990154418,-0.802986704379283));
#45280=DIRECTION('ref_axis',(0.,-0.809016994374948,0.587785252292473));
#45281=DIRECTION('center_axis',(0.992546151641322,0.0716330027601127,0.0985943699080808));
#45282=DIRECTION('ref_axis',(0.,0.809016994374947,-0.587785252292473));
#45283=DIRECTION('center_axis',(-0.992546151641322,-0.0716330027601127,
-0.0985943699080808));
#45284=DIRECTION('ref_axis',(0.,-0.809016994374947,0.587785252292473));
#45285=DIRECTION('center_axis',(0.992546151641322,0.0985943699080808,0.0716330027601127));
#45286=DIRECTION('ref_axis',(0.,0.587785252292473,-0.809016994374947));
#45287=DIRECTION('center_axis',(-0.992546151641322,-0.0985943699080807,
-0.0716330027601125));
#45288=DIRECTION('ref_axis',(0.121869343405147,-0.802986704379283,-0.583403990154418));
#45289=DIRECTION('center_axis',(0.121869343405148,-0.802986704379283,-0.583403990154418));
#45290=DIRECTION('ref_axis',(0.,-0.587785252292473,0.809016994374947));
#45291=DIRECTION('center_axis',(0.992546151641322,0.0985943699080808,0.0716330027601127));
#45292=DIRECTION('ref_axis',(0.121869343405148,-0.802986704379283,-0.583403990154418));
#45293=DIRECTION('center_axis',(-0.992546151641322,-0.0985943699080807,
-0.0716330027601125));
#45294=DIRECTION('ref_axis',(0.121869343405147,-0.802986704379283,-0.583403990154418));
#45295=DIRECTION('center_axis',(0.992546151641322,0.0985943699080808,0.0716330027601127));
#45296=DIRECTION('ref_axis',(-0.121869343405147,0.802986704379283,0.583403990154418));
#45297=DIRECTION('center_axis',(0.992546151641322,0.0985943699080813,0.071633002760112));
#45298=DIRECTION('ref_axis',(0.121869343405148,-0.802986704379283,-0.583403990154418));
#45299=DIRECTION('center_axis',(0.992546151641322,0.0985943699080813,0.071633002760112));
#45300=DIRECTION('ref_axis',(0.121869343405148,-0.802986704379283,-0.583403990154418));
#45301=DIRECTION('center_axis',(0.992546151641322,0.0985943699080808,0.0716330027601127));
#45302=DIRECTION('ref_axis',(0.,0.587785252292473,-0.809016994374948));
#45303=DIRECTION('center_axis',(-0.992546151641322,-0.0985943699080808,
-0.0716330027601127));
#45304=DIRECTION('ref_axis',(0.121869343405147,-0.802986704379283,-0.583403990154418));
#45305=DIRECTION('center_axis',(0.121869343405147,-0.802986704379283,-0.583403990154418));
#45306=DIRECTION('ref_axis',(0.,-0.587785252292474,0.809016994374947));
#45307=DIRECTION('center_axis',(0.992546151641322,0.0985943699080808,0.0716330027601127));
#45308=DIRECTION('ref_axis',(0.,0.587785252292473,-0.809016994374947));
#45309=DIRECTION('center_axis',(-0.992546151641322,-0.0985943699080808,
-0.0716330027601127));
#45310=DIRECTION('ref_axis',(0.,-0.587785252292473,0.809016994374947));
#45311=DIRECTION('center_axis',(0.992546151641322,0.115904633182077,0.037659698205507));
#45312=DIRECTION('ref_axis',(0.,0.309016994374948,-0.951056516295153));
#45313=DIRECTION('center_axis',(-0.992546151641322,-0.115904633182077,-0.0376596982055069));
#45314=DIRECTION('ref_axis',(0.121869343405147,-0.943967485242157,-0.306713628558622));
#45315=DIRECTION('center_axis',(0.121869343405148,-0.943967485242157,-0.306713628558623));
#45316=DIRECTION('ref_axis',(0.,-0.309016994374948,0.951056516295153));
#45317=DIRECTION('center_axis',(0.992546151641322,0.115904633182077,0.037659698205507));
#45318=DIRECTION('ref_axis',(0.121869343405148,-0.943967485242157,-0.306713628558622));
#45319=DIRECTION('center_axis',(-0.992546151641322,-0.115904633182077,-0.0376596982055069));
#45320=DIRECTION('ref_axis',(0.121869343405147,-0.943967485242157,-0.306713628558622));
#45321=DIRECTION('center_axis',(0.992546151641322,0.115904633182077,0.037659698205507));
#45322=DIRECTION('ref_axis',(-0.121869343405147,0.943967485242157,0.306713628558622));
#45323=DIRECTION('center_axis',(0.992546151641322,0.115904633182078,0.0376596982055062));
#45324=DIRECTION('ref_axis',(0.121869343405148,-0.943967485242157,-0.306713628558622));
#45325=DIRECTION('center_axis',(0.992546151641322,0.115904633182078,0.0376596982055062));
#45326=DIRECTION('ref_axis',(0.121869343405148,-0.943967485242157,-0.306713628558622));
#45327=DIRECTION('center_axis',(0.992546151641322,0.115904633182077,0.037659698205507));
#45328=DIRECTION('ref_axis',(0.,0.309016994374948,-0.951056516295154));
#45329=DIRECTION('center_axis',(-0.992546151641322,-0.115904633182077,-0.037659698205507));
#45330=DIRECTION('ref_axis',(0.121869343405147,-0.943967485242157,-0.306713628558622));
#45331=DIRECTION('center_axis',(0.121869343405148,-0.943967485242157,-0.306713628558623));
#45332=DIRECTION('ref_axis',(0.,-0.309016994374948,0.951056516295153));
#45333=DIRECTION('center_axis',(0.992546151641322,0.115904633182077,0.037659698205507));
#45334=DIRECTION('ref_axis',(0.,0.309016994374947,-0.951056516295154));
#45335=DIRECTION('center_axis',(-0.992546151641322,-0.115904633182077,-0.037659698205507));
#45336=DIRECTION('ref_axis',(0.,-0.309016994374947,0.951056516295154));
#45337=DIRECTION('center_axis',(0.992546151641322,0.121869343405147,0.));
#45338=DIRECTION('ref_axis',(0.,0.,-1.));
#45339=DIRECTION('center_axis',(-0.992546151641322,-0.121869343405147,1.171397475895E-16));
#45340=DIRECTION('ref_axis',(0.121869343405147,-0.992546151641322,-6.12323399573677E-17));
#45341=DIRECTION('center_axis',(0.121869343405147,-0.992546151641322,0.));
#45342=DIRECTION('ref_axis',(0.,0.,1.));
#45343=DIRECTION('center_axis',(0.992546151641322,0.121869343405147,0.));
#45344=DIRECTION('ref_axis',(0.121869343405148,-0.992546151641322,0.));
#45345=DIRECTION('center_axis',(-0.992546151641322,-0.121869343405147,1.171397475895E-16));
#45346=DIRECTION('ref_axis',(0.121869343405147,-0.992546151641322,-6.12323399573677E-17));
#45347=DIRECTION('center_axis',(0.992546151641322,0.121869343405147,0.));
#45348=DIRECTION('ref_axis',(-0.121869343405147,0.992546151641322,0.));
#45349=DIRECTION('center_axis',(0.992546151641322,0.121869343405148,-8.3244736629265E-16));
#45350=DIRECTION('ref_axis',(0.121869343405148,-0.992546151641322,-6.12323399573677E-17));
#45351=DIRECTION('center_axis',(0.992546151641322,0.121869343405148,-8.3244736629265E-16));
#45352=DIRECTION('ref_axis',(0.121869343405148,-0.992546151641322,-6.12323399573677E-17));
#45353=DIRECTION('center_axis',(0.992546151641322,0.121869343405147,0.));
#45354=DIRECTION('ref_axis',(0.,0.,-1.));
#45355=DIRECTION('center_axis',(-0.992546151641322,-0.121869343405147,0.));
#45356=DIRECTION('ref_axis',(0.121869343405147,-0.992546151641322,0.));
#45357=DIRECTION('center_axis',(0.121869343405147,-0.992546151641322,0.));
#45358=DIRECTION('ref_axis',(0.,0.,1.));
#45359=DIRECTION('center_axis',(0.992546151641322,0.121869343405147,0.));
#45360=DIRECTION('ref_axis',(0.,0.,-1.));
#45361=DIRECTION('center_axis',(-0.992546151641322,-0.121869343405147,0.));
#45362=DIRECTION('ref_axis',(0.,0.,1.));
#45363=DIRECTION('center_axis',(1.,0.,0.));
#45364=DIRECTION('ref_axis',(0.,1.,0.));
#45365=DIRECTION('',(-0.707106781186549,0.707106781186546,8.65956056235491E-17));
#45366=DIRECTION('center_axis',(1.,0.,0.));
#45367=DIRECTION('ref_axis',(0.,0.,-1.));
#45368=DIRECTION('center_axis',(1.,0.,0.));
#45369=DIRECTION('ref_axis',(0.,1.,0.));
#45370=DIRECTION('',(-0.996194698091746,0.087155742747658,1.0673500138323E-17));
#45371=DIRECTION('',(-0.996194698091746,0.087155742747658,1.0673500138323E-17));
#45372=DIRECTION('center_axis',(-1.,0.,0.));
#45373=DIRECTION('ref_axis',(0.,1.,0.));
#45374=DIRECTION('center_axis',(1.,0.,0.));
#45375=DIRECTION('ref_axis',(0.,0.,-1.));
#45376=DIRECTION('',(-0.707106781186546,-0.707106781186549,-8.65956056235495E-17));
#45377=DIRECTION('center_axis',(1.,0.,0.));
#45378=DIRECTION('ref_axis',(0.,0.,-1.));
#45379=DIRECTION('center_axis',(1.,0.,0.));
#45380=DIRECTION('ref_axis',(0.,0.,-1.));
#45381=DIRECTION('center_axis',(1.,0.,0.));
#45382=DIRECTION('ref_axis',(0.,1.,0.));
#45383=DIRECTION('',(-0.707106781186547,0.707106781186547,8.65956056235493E-17));
#45384=DIRECTION('center_axis',(1.,0.,0.));
#45385=DIRECTION('ref_axis',(0.,0.,-1.));
#45386=DIRECTION('center_axis',(1.,0.,0.));
#45387=DIRECTION('ref_axis',(0.,1.,0.));
#45388=DIRECTION('',(-1.,0.,0.));
#45389=DIRECTION('center_axis',(1.,0.,0.));
#45390=DIRECTION('ref_axis',(0.,0.,-1.));
#45391=DIRECTION('center_axis',(-1.,0.,0.));
#45392=DIRECTION('ref_axis',(0.,1.,0.));
#45393=DIRECTION('',(-0.707106781186547,-0.707106781186548,-8.65956056235494E-17));
#45394=DIRECTION('center_axis',(1.,0.,0.));
#45395=DIRECTION('ref_axis',(0.,0.,-1.));
#45396=DIRECTION('center_axis',(-1.,0.,0.));
#45397=DIRECTION('ref_axis',(0.,0.,1.));
#45398=DIRECTION('axis',(0.,0.,1.));
#45399=DIRECTION('refdir',(1.,0.,0.));
#45400=DIRECTION('center_axis',(0.707106781186548,0.,0.707106781186548));
#45401=DIRECTION('ref_axis',(0.707106781186548,0.,-0.707106781186548));
#45402=DIRECTION('',(0.707106781186547,0.,-0.707106781186547));
#45403=DIRECTION('',(0.,1.,0.));
#45404=DIRECTION('',(-0.707106781186547,0.,0.707106781186547));
#45405=DIRECTION('',(0.,-1.,0.));
#45406=DIRECTION('center_axis',(0.,-1.,0.));
#45407=DIRECTION('ref_axis',(0.,0.,-1.));
#45408=DIRECTION('',(1.,0.,0.));
#45409=DIRECTION('',(0.707106781186547,0.,0.707106781186548));
#45410=DIRECTION('',(0.,0.,-1.));
#45411=DIRECTION('',(-1.,0.,0.));
#45412=DIRECTION('',(0.,0.,-1.));
#45413=DIRECTION('center_axis',(0.,0.,1.));
#45414=DIRECTION('ref_axis',(0.,-1.,0.));
#45415=DIRECTION('',(1.,0.,0.));
#45416=DIRECTION('',(0.,1.,0.));
#45417=DIRECTION('center_axis',(-0.707106781186548,0.,0.707106781186547));
#45418=DIRECTION('ref_axis',(0.707106781186547,0.,0.707106781186548));
#45419=DIRECTION('',(-0.707106781186547,0.,-0.707106781186548));
#45420=DIRECTION('',(0.,-1.,0.));
#45421=DIRECTION('center_axis',(0.,1.,0.));
#45422=DIRECTION('ref_axis',(0.,0.,1.));
#45423=DIRECTION('',(0.,0.,1.));
#45424=DIRECTION('',(1.,0.,0.));
#45425=DIRECTION('',(0.,0.,1.));
#45426=DIRECTION('center_axis',(1.,0.,0.));
#45427=DIRECTION('ref_axis',(0.,0.,-1.));
#45428=DIRECTION('center_axis',(1.,0.,0.));
#45429=DIRECTION('ref_axis',(0.,0.,-1.));
#45430=DIRECTION('center_axis',(1.,0.,0.));
#45431=DIRECTION('ref_axis',(0.,0.,-1.));
#45432=DIRECTION('center_axis',(1.,0.,0.));
#45433=DIRECTION('ref_axis',(0.,6.12323399573677E-17,1.));
#45434=DIRECTION('center_axis',(1.,0.,0.));
#45435=DIRECTION('ref_axis',(0.,0.,-1.));
#45436=DIRECTION('center_axis',(-1.,0.,0.));
#45437=DIRECTION('ref_axis',(0.,0.,1.));
#45438=DIRECTION('center_axis',(1.,0.,0.));
#45439=DIRECTION('ref_axis',(0.,0.,-1.));
#45440=DIRECTION('center_axis',(1.,0.,0.));
#45441=DIRECTION('ref_axis',(0.,1.,0.));
#45442=DIRECTION('center_axis',(1.,0.,0.));
#45443=DIRECTION('ref_axis',(0.,0.,-1.));
#45444=DIRECTION('',(-0.554700196225232,0.832050294337842,1.01896772969045E-16));
#45445=DIRECTION('center_axis',(1.,0.,0.));
#45446=DIRECTION('ref_axis',(0.,1.,0.));
#45447=DIRECTION('center_axis',(1.,0.,0.));
#45448=DIRECTION('ref_axis',(0.,0.,-1.));
#45449=DIRECTION('',(-1.,0.,0.));
#45450=DIRECTION('center_axis',(-1.,0.,0.));
#45451=DIRECTION('ref_axis',(0.,1.,0.));
#45452=DIRECTION('',(-0.554700196225231,-0.832050294337843,-1.01896772969045E-16));
#45453=DIRECTION('axis',(0.,0.,1.));
#45454=DIRECTION('refdir',(1.,0.,0.));
#45455=DIRECTION('center_axis',(0.707106781186547,0.353553390593274,0.612372435695795));
#45456=DIRECTION('ref_axis',(0.654653670707978,0.,-0.755928946018454));
#45457=DIRECTION('',(0.,0.866025403784439,-0.5));
#45458=DIRECTION('',(-0.532735444826016,-0.303096428117156,0.790142709318164));
#45459=DIRECTION('',(0.,-0.866025403784439,0.5));
#45460=DIRECTION('center_axis',(1.,0.,0.));
#45461=DIRECTION('ref_axis',(0.,0.,-1.));
#45462=DIRECTION('center_axis',(1.,0.,0.));
#45463=DIRECTION('ref_axis',(0.,1.,0.));
#45464=DIRECTION('',(0.,-0.866025403784439,-0.5));
#45465=DIRECTION('center_axis',(1.,0.,0.));
#45466=DIRECTION('ref_axis',(0.,0.,-1.));
#45467=DIRECTION('center_axis',(-1.,0.,0.));
#45468=DIRECTION('ref_axis',(0.,-1.,1.22464679914735E-16));
#45469=DIRECTION('center_axis',(0.,-0.5,-0.866025403784439));
#45470=DIRECTION('ref_axis',(0.,-0.866025403784439,0.5));
#45471=DIRECTION('',(1.,0.,0.));
#45472=DIRECTION('',(0.,-0.866025403784439,0.5));
#45473=DIRECTION('',(-0.654653670707977,-0.654653670707977,0.377964473009227));
#45474=DIRECTION('',(-1.,0.,0.));
#45475=DIRECTION('center_axis',(0.,-0.5,0.866025403784438));
#45476=DIRECTION('ref_axis',(1.,0.,0.));
#45477=DIRECTION('',(0.654653670707977,0.654653670707977,0.377964473009228));
#45478=DIRECTION('',(1.,0.,0.));
#45479=DIRECTION('center_axis',(0.,-0.500000000000004,-0.866025403784436));
#45480=DIRECTION('ref_axis',(-1.,0.,0.));
#45481=DIRECTION('',(1.,0.,0.));
#45482=DIRECTION('',(-1.,0.,0.));
#45483=DIRECTION('',(0.654653670707977,0.654653670707975,-0.377964473009231));
#45484=DIRECTION('center_axis',(0.707106781186548,-0.707106781186548,-1.49012597864166E-16));
#45485=DIRECTION('ref_axis',(-2.10735636863952E-16,0.,-1.));
#45486=DIRECTION('',(0.,2.10735636863952E-16,-1.));
#45487=DIRECTION('',(0.447213595499958,0.447213595499958,-0.774596669241483));
#45488=DIRECTION('',(0.654653670707976,0.654653670707976,0.37796447300923));
#45489=DIRECTION('',(0.,-2.10735636863952E-16,1.));
#45490=DIRECTION('',(-0.654653670707977,-0.654653670707977,-0.377964473009227));
#45491=DIRECTION('center_axis',(0.,-0.5,0.866025403784439));
#45492=DIRECTION('ref_axis',(0.,0.866025403784439,0.5));
#45493=DIRECTION('',(0.,0.866025403784439,0.5));
#45494=DIRECTION('',(-1.,0.,0.));
#45495=DIRECTION('',(0.,0.866025403784439,0.5));
#45496=DIRECTION('center_axis',(-1.,0.,0.));
#45497=DIRECTION('ref_axis',(0.,-0.866025403784439,-0.5));
#45498=DIRECTION('',(0.,-0.866025403784439,0.5));
#45499=DIRECTION('',(0.,-0.866025403784439,-0.5));
#45500=DIRECTION('center_axis',(1.,0.,0.));
#45501=DIRECTION('ref_axis',(0.,0.,-1.));
#45502=DIRECTION('center_axis',(0.707106781186549,-0.353553390593273,-0.612372435695793));
#45503=DIRECTION('ref_axis',(-0.654653670707976,0.,-0.755928946018456));
#45504=DIRECTION('',(-0.447213595499956,0.447213595499958,-0.774596669241484));
#45505=DIRECTION('',(0.,0.866025403784439,-0.5));
#45506=DIRECTION('',(-0.654653670707975,-3.35699888340127E-15,-0.755928946018457));
#45507=DIRECTION('',(0.654653670707976,0.654653670707978,0.377964473009228));
#45508=DIRECTION('center_axis',(0.707106781186546,0.353553390593274,-0.612372435695796));
#45509=DIRECTION('ref_axis',(-0.654653670707979,0.,-0.755928946018453));
#45510=DIRECTION('',(0.532735444826017,0.303096428117156,0.790142709318163));
#45511=DIRECTION('center_axis',(1.,0.,0.));
#45512=DIRECTION('ref_axis',(0.,0.,-1.));
#45513=DIRECTION('center_axis',(-1.,0.,0.));
#45514=DIRECTION('ref_axis',(0.,0.,-1.));
#45515=DIRECTION('center_axis',(0.,-0.866025403784437,0.500000000000003));
#45516=DIRECTION('ref_axis',(1.,0.,0.));
#45517=DIRECTION('',(-0.447213595499955,0.447213595499962,0.774596669241483));
#45518=DIRECTION('',(-1.,0.,0.));
#45519=DIRECTION('',(1.,0.,0.));
#45520=DIRECTION('',(0.44721359549996,0.44721359549996,0.774596669241481));
#45521=DIRECTION('center_axis',(0.,-0.5,0.866025403784439));
#45522=DIRECTION('ref_axis',(0.,-0.866025403784439,-0.5));
#45523=DIRECTION('',(0.,-0.866025403784439,-0.5));
#45524=DIRECTION('',(-1.,0.,0.));
#45525=DIRECTION('',(1.,0.,0.));
#45526=DIRECTION('',(0.,-0.866025403784439,-0.5));
#45527=DIRECTION('',(1.,0.,0.));
#45528=DIRECTION('center_axis',(0.707106781186549,-0.353553390593273,0.612372435695794));
#45529=DIRECTION('ref_axis',(0.654653670707976,0.,-0.755928946018455));
#45530=DIRECTION('',(-0.654653670707977,-0.654653670707977,0.377964473009228));
#45531=DIRECTION('',(0.,0.866025403784439,0.5));
#45532=DIRECTION('',(-0.654653670707976,-0.654653670707978,0.377964473009228));
#45533=DIRECTION('',(0.654653670707976,0.,-0.755928946018455));
#45534=DIRECTION('center_axis',(0.707106781186548,-0.707106781186548,-1.49012597864166E-16));
#45535=DIRECTION('ref_axis',(-2.10735636863952E-16,0.,-1.));
#45536=DIRECTION('',(0.,2.10735636863952E-16,-1.));
#45537=DIRECTION('',(0.,-2.10735636863952E-16,1.));
#45538=DIRECTION('center_axis',(0.707106781186547,-0.353553390593274,0.612372435695795));
#45539=DIRECTION('ref_axis',(0.654653670707978,0.,-0.755928946018454));
#45540=DIRECTION('',(0.,0.866025403784439,0.5));
#45541=DIRECTION('',(-0.532735444826014,-0.835831872943173,0.132582148113298));
#45542=DIRECTION('',(0.,-0.866025403784439,-0.5));
#45543=DIRECTION('center_axis',(1.,0.,0.));
#45544=DIRECTION('ref_axis',(0.,0.,-1.));
#45545=DIRECTION('center_axis',(1.,0.,0.));
#45546=DIRECTION('ref_axis',(0.,0.,-1.));
#45547=DIRECTION('center_axis',(-1.,0.,0.));
#45548=DIRECTION('ref_axis',(0.,0.,-1.));
#45549=DIRECTION('center_axis',(1.,0.,0.));
#45550=DIRECTION('ref_axis',(0.,0.,-1.));
#45551=DIRECTION('center_axis',(1.,0.,0.));
#45552=DIRECTION('ref_axis',(0.,1.,0.));
#45553=DIRECTION('',(0.,-1.22464679914735E-16,-1.));
#45554=DIRECTION('center_axis',(-1.,0.,0.));
#45555=DIRECTION('ref_axis',(0.,1.,0.));
#45556=DIRECTION('center_axis',(0.,-1.,0.));
#45557=DIRECTION('ref_axis',(0.,0.,-1.));
#45558=DIRECTION('',(1.,0.,0.));
#45559=DIRECTION('',(-1.,0.,0.));
#45560=DIRECTION('center_axis',(0.,-0.866025403784439,-0.5));
#45561=DIRECTION('ref_axis',(-1.,0.,0.));
#45562=DIRECTION('',(-1.,0.,0.));
#45563=DIRECTION('',(1.,0.,0.));
#45564=DIRECTION('center_axis',(0.,-0.5,-0.866025403784439));
#45565=DIRECTION('ref_axis',(0.,0.866025403784439,-0.5));
#45566=DIRECTION('',(-1.,0.,0.));
#45567=DIRECTION('',(0.,0.866025403784439,-0.5));
#45568=DIRECTION('',(-1.,0.,0.));
#45569=DIRECTION('center_axis',(1.,0.,0.));
#45570=DIRECTION('ref_axis',(0.,1.,0.));
#45571=DIRECTION('center_axis',(-1.,0.,0.));
#45572=DIRECTION('ref_axis',(0.,1.,0.));
#45573=DIRECTION('',(0.360399279202162,-0.932798134405597,-1.14234824955044E-16));
#45574=DIRECTION('center_axis',(0.707106781186547,-0.707106781186548,8.65956056235494E-17));
#45575=DIRECTION('ref_axis',(1.22464679914735E-16,0.,-1.));
#45576=DIRECTION('',(0.,1.22464679914735E-16,1.));
#45577=DIRECTION('',(-0.532735444826015,-0.532735444826014,-0.657560561204865));
#45578=DIRECTION('',(0.,-1.22464679914735E-16,-1.));
#45579=DIRECTION('center_axis',(1.,0.,0.));
#45580=DIRECTION('ref_axis',(0.,0.,-1.));
#45581=DIRECTION('center_axis',(1.,0.,0.));
#45582=DIRECTION('ref_axis',(0.,1.,0.));
#45583=DIRECTION('',(0.,0.866025403784438,-0.5));
#45584=DIRECTION('center_axis',(1.,0.,0.));
#45585=DIRECTION('ref_axis',(0.,0.,-1.));
#45586=DIRECTION('center_axis',(-1.,0.,0.));
#45587=DIRECTION('ref_axis',(0.,1.,0.));
#45588=DIRECTION('center_axis',(0.,1.,-1.22464679914735E-16));
#45589=DIRECTION('ref_axis',(0.,-1.22464679914735E-16,-1.));
#45590=DIRECTION('',(1.,0.,0.));
#45591=DIRECTION('',(0.,-1.22464679914735E-16,-1.));
#45592=DIRECTION('',(0.65465367070798,9.2574596412433E-17,0.755928946018452));
#45593=DIRECTION('',(-1.,0.,0.));
#45594=DIRECTION('center_axis',(0.,-0.499999999999999,-0.866025403784439));
#45595=DIRECTION('ref_axis',(-1.,0.,0.));
#45596=DIRECTION('',(1.,0.,0.));
#45597=DIRECTION('',(-0.654653670707979,0.654653670707976,-0.377964473009225));
#45598=DIRECTION('center_axis',(0.547750005235848,5.84175495892749E-17,
-0.836642057133233));
#45599=DIRECTION('ref_axis',(-0.836642057133233,0.,-0.547750005235848));
#45600=DIRECTION('',(0.,-1.,0.));
#45601=DIRECTION('',(-0.677497944020813,0.586730430533744,-0.443558268701259));
#45602=DIRECTION('',(0.677497944020809,0.586730430533752,0.443558268701256));
#45603=DIRECTION('center_axis',(0.707106781186545,0.353553390593275,-0.612372435695797));
#45604=DIRECTION('ref_axis',(-0.65465367070798,0.,-0.755928946018452));
#45605=DIRECTION('',(0.,-0.866025403784439,-0.5));
#45606=DIRECTION('',(0.,0.866025403784439,0.5));
#45607=DIRECTION('center_axis',(0.,0.500000000000003,-0.866025403784437));
#45608=DIRECTION('ref_axis',(-1.,0.,0.));
#45609=DIRECTION('',(1.,0.,0.));
#45610=DIRECTION('',(0.654653670707977,0.654653670707975,0.377964473009231));
#45611=DIRECTION('center_axis',(0.707106781186548,-0.353553390593274,-0.612372435695794));
#45612=DIRECTION('ref_axis',(-0.654653670707977,0.,-0.755928946018455));
#45613=DIRECTION('',(0.,-0.866025403784439,0.5));
#45614=DIRECTION('',(-0.654653670707977,-9.25745964124333E-17,-0.755928946018455));
#45615=DIRECTION('center_axis',(0.,0.,-1.));
#45616=DIRECTION('ref_axis',(-1.,0.,0.));
#45617=DIRECTION('',(1.,0.,0.));
#45618=DIRECTION('center_axis',(0.,0.5,-0.866025403784439));
#45619=DIRECTION('ref_axis',(0.,0.866025403784439,0.5));
#45620=DIRECTION('',(-1.,0.,0.));
#45621=DIRECTION('',(0.,0.866025403784439,0.5));
#45622=DIRECTION('',(-1.,0.,0.));
#45623=DIRECTION('center_axis',(0.707106781186547,0.707106781186548,-8.65956056235494E-17));
#45624=DIRECTION('ref_axis',(-1.22464679914735E-16,0.,-1.));
#45625=DIRECTION('',(0.,1.22464679914735E-16,1.));
#45626=DIRECTION('',(0.532735444826015,-0.532735444826015,0.657560561204864));
#45627=DIRECTION('center_axis',(0.,1.,0.));
#45628=DIRECTION('ref_axis',(0.,0.,1.));
#45629=DIRECTION('',(1.,0.,0.));
#45630=DIRECTION('',(0.654653670707976,0.,0.755928946018455));
#45631=DIRECTION('center_axis',(0.707106781186547,0.353553390593274,-0.612372435695795));
#45632=DIRECTION('ref_axis',(-0.654653670707978,0.,-0.755928946018454));
#45633=DIRECTION('',(0.447213595499961,0.447213595499955,0.774596669241484));
#45634=DIRECTION('',(0.654653670707978,-0.654653670707975,0.377964473009229));
#45635=DIRECTION('',(0.,-0.866025403784439,-0.5));
#45636=DIRECTION('',(-0.654653670707977,0.654653670707977,-0.377964473009227));
#45637=DIRECTION('center_axis',(0.,-0.5,-0.866025403784438));
#45638=DIRECTION('ref_axis',(0.,-0.866025403784438,0.5));
#45639=DIRECTION('',(0.,-0.866025403784438,0.5));
#45640=DIRECTION('',(-1.,0.,0.));
#45641=DIRECTION('',(0.,-0.866025403784438,0.5));
#45642=DIRECTION('center_axis',(-1.,0.,0.));
#45643=DIRECTION('ref_axis',(0.,0.866025403784438,-0.5));
#45644=DIRECTION('',(0.,-3.16103455295928E-16,-1.));
#45645=DIRECTION('',(0.,0.866025403784438,-0.5));
#45646=DIRECTION('center_axis',(1.,0.,0.));
#45647=DIRECTION('ref_axis',(0.,0.,-1.));
#45648=DIRECTION('center_axis',(0.707106781186546,0.707106781186549,-2.2351889679625E-16));
#45649=DIRECTION('ref_axis',(-3.1610345529593E-16,0.,-1.));
#45650=DIRECTION('',(-0.447213595499957,0.447213595499956,0.774596669241486));
#45651=DIRECTION('',(0.,3.16103455295928E-16,1.));
#45652=DIRECTION('',(-0.65465367070798,0.654653670707975,0.377964473009226));
#45653=DIRECTION('',(0.654653670707979,-0.654653670707976,0.377964473009227));
#45654=DIRECTION('center_axis',(0.707106781186547,0.353553390593275,0.612372435695795));
#45655=DIRECTION('ref_axis',(0.654653670707978,0.,-0.755928946018454));
#45656=DIRECTION('',(0.532735444826016,-0.835831872943172,-0.132582148113299));
#45657=DIRECTION('center_axis',(1.,0.,0.));
#45658=DIRECTION('ref_axis',(0.,0.,-1.));
#45659=DIRECTION('center_axis',(-1.,0.,0.));
#45660=DIRECTION('ref_axis',(0.,0.,-1.));
#45661=DIRECTION('center_axis',(0.707106781186549,-0.353553390593273,0.612372435695793));
#45662=DIRECTION('ref_axis',(0.654653670707976,0.,-0.755928946018456));
#45663=DIRECTION('',(-0.447213595499957,-0.894427190999917,0.));
#45664=DIRECTION('',(-0.654653670707977,-0.654653670707975,0.377964473009231));
#45665=DIRECTION('',(-0.654653670707976,0.,0.755928946018456));
#45666=DIRECTION('',(0.,0.866025403784439,0.5));
#45667=DIRECTION('',(-0.654653670707977,-2.93737402297611E-15,0.755928946018455));
#45668=DIRECTION('center_axis',(0.,0.,1.));
#45669=DIRECTION('ref_axis',(1.,0.,0.));
#45670=DIRECTION('',(-0.447213595499958,0.894427190999916,0.));
#45671=DIRECTION('',(-1.,0.,0.));
#45672=DIRECTION('center_axis',(0.,-1.,0.));
#45673=DIRECTION('ref_axis',(0.,0.,-1.));
#45674=DIRECTION('',(1.,0.,0.));
#45675=DIRECTION('center_axis',(-1.,0.,0.));
#45676=DIRECTION('ref_axis',(0.,1.,0.));
#45677=DIRECTION('center_axis',(1.,0.,0.));
#45678=DIRECTION('ref_axis',(0.,1.,0.));
#45679=DIRECTION('center_axis',(0.,0.5,0.866025403784439));
#45680=DIRECTION('ref_axis',(0.,0.866025403784439,-0.5));
#45681=DIRECTION('',(0.,0.866025403784439,-0.5));
#45682=DIRECTION('',(-1.,0.,0.));
#45683=DIRECTION('',(0.,0.866025403784439,-0.5));
#45684=DIRECTION('center_axis',(-1.,0.,0.));
#45685=DIRECTION('ref_axis',(0.,-0.866025403784439,0.5));
#45686=DIRECTION('center_axis',(1.,0.,0.));
#45687=DIRECTION('ref_axis',(0.,0.,1.));
#45688=DIRECTION('center_axis',(0.,0.5,0.866025403784439));
#45689=DIRECTION('ref_axis',(0.,-0.866025403784439,0.5));
#45690=DIRECTION('',(0.,-0.866025403784439,0.5));
#45691=DIRECTION('',(-1.,0.,0.));
#45692=DIRECTION('',(1.,0.,0.));
#45693=DIRECTION('',(0.,-0.866025403784439,0.5));
#45694=DIRECTION('',(1.,0.,0.));
#45695=DIRECTION('center_axis',(0.707106781186547,0.353553390593274,0.612372435695795));
#45696=DIRECTION('ref_axis',(0.654653670707978,0.,-0.755928946018454));
#45697=DIRECTION('',(0.,0.866025403784439,-0.5));
#45698=DIRECTION('',(0.654653670707978,0.,-0.755928946018454));
#45699=DIRECTION('',(-0.654653670707979,0.654653670707974,0.37796447300923));
#45700=DIRECTION('center_axis',(0.,-0.500000000000005,0.866025403784436));
#45701=DIRECTION('ref_axis',(1.,0.,0.));
#45702=DIRECTION('',(1.,0.,0.));
#45703=DIRECTION('center_axis',(0.,1.,0.));
#45704=DIRECTION('ref_axis',(0.,0.,-1.));
#45705=DIRECTION('',(0.,0.,-1.));
#45706=DIRECTION('',(-1.,0.,0.));
#45707=DIRECTION('',(0.,0.,-1.));
#45708=DIRECTION('center_axis',(0.,0.500000000000005,0.866025403784436));
#45709=DIRECTION('ref_axis',(1.,0.,0.));
#45710=DIRECTION('',(-1.,0.,0.));
#45711=DIRECTION('center_axis',(0.,-1.,0.));
#45712=DIRECTION('ref_axis',(0.,0.,1.));
#45713=DIRECTION('',(0.,0.,1.));
#45714=DIRECTION('',(1.,0.,0.));
#45715=DIRECTION('',(0.,0.,1.));
#45716=DIRECTION('center_axis',(0.707106781186547,0.707106781186548,0.));
#45717=DIRECTION('ref_axis',(0.,0.,-1.));
#45718=DIRECTION('',(0.,0.,-1.));
#45719=DIRECTION('',(-0.532735444826015,0.532735444826015,0.657560561204864));
#45720=DIRECTION('center_axis',(1.,0.,0.));
#45721=DIRECTION('ref_axis',(0.,0.,1.));
#45722=DIRECTION('center_axis',(1.,0.,0.));
#45723=DIRECTION('ref_axis',(0.,0.,1.));
#45724=DIRECTION('center_axis',(-1.,0.,0.));
#45725=DIRECTION('ref_axis',(0.,0.,1.));
#45726=DIRECTION('center_axis',(1.,0.,0.));
#45727=DIRECTION('ref_axis',(0.,0.,-1.));
#45728=DIRECTION('',(0.,-0.866025403784439,0.5));
#45729=DIRECTION('center_axis',(0.550547030005201,0.13078400442267,-0.824495913840465));
#45730=DIRECTION('ref_axis',(-0.831638955930086,0.,-0.555316708716312));
#45731=DIRECTION('',(0.,-0.987651911521988,-0.1566642960823));
#45732=DIRECTION('',(0.701026414838316,0.463839941019002,0.541677463823654));
#45733=DIRECTION('center_axis',(0.707106781186545,-0.353553390593275,-0.612372435695796));
#45734=DIRECTION('ref_axis',(-0.654653670707979,0.,-0.755928946018453));
#45735=DIRECTION('center_axis',(0.,0.1566642960823,-0.987651911521988));
#45736=DIRECTION('ref_axis',(-1.,0.,0.));
#45737=DIRECTION('',(1.,0.,0.));
#45738=DIRECTION('center_axis',(0.,0.933663793515453,0.358150695487714));
#45739=DIRECTION('ref_axis',(0.,-0.358150695487714,0.933663793515453));
#45740=DIRECTION('',(-1.,0.,0.));
#45741=DIRECTION('center_axis',(0.,0.933663793515453,-0.358150695487715));
#45742=DIRECTION('ref_axis',(0.,0.358150695487715,0.933663793515453));
#45743=DIRECTION('',(1.,0.,0.));
#45744=DIRECTION('center_axis',(0.,0.776999497433153,0.629501216034272));
#45745=DIRECTION('ref_axis',(1.,0.,0.));
#45746=DIRECTION('',(-1.,0.,0.));
#45747=DIRECTION('',(1.,0.,0.));
#45748=DIRECTION('center_axis',(0.,-0.776999497433154,0.629501216034272));
#45749=DIRECTION('ref_axis',(1.,0.,0.));
#45750=DIRECTION('',(-1.,0.,0.));
#45751=DIRECTION('center_axis',(0.,-0.156664296082299,0.987651911521989));
#45752=DIRECTION('ref_axis',(1.,0.,0.));
#45753=DIRECTION('',(1.,0.,0.));
#45754=DIRECTION('center_axis',(0.,-0.933663793515451,-0.358150695487721));
#45755=DIRECTION('ref_axis',(0.,0.358150695487721,-0.933663793515451));
#45756=DIRECTION('',(1.,0.,0.));
#45757=DIRECTION('',(0.532735444826014,-0.303096428117161,0.790142709318163));
#45758=DIRECTION('',(-1.,0.,0.));
#45759=DIRECTION('center_axis',(1.,0.,0.));
#45760=DIRECTION('ref_axis',(0.,0.,-1.));
#45761=DIRECTION('center_axis',(-1.,0.,0.));
#45762=DIRECTION('ref_axis',(0.,0.,-1.));
#45763=DIRECTION('center_axis',(1.,0.,0.));
#45764=DIRECTION('ref_axis',(0.,0.,-1.));
#45765=DIRECTION('center_axis',(1.,0.,0.));
#45766=DIRECTION('ref_axis',(0.,0.,-1.));
#45767=DIRECTION('center_axis',(-1.,0.,0.));
#45768=DIRECTION('ref_axis',(0.,0.,-1.));
#45769=DIRECTION('center_axis',(0.,0.156664296082297,0.987651911521989));
#45770=DIRECTION('ref_axis',(1.,0.,0.));
#45771=DIRECTION('',(-1.,0.,0.));
#45772=DIRECTION('',(1.,0.,0.));
#45773=DIRECTION('center_axis',(1.,0.,0.));
#45774=DIRECTION('ref_axis',(0.,0.,-1.));
#45775=DIRECTION('center_axis',(-1.,0.,0.));
#45776=DIRECTION('ref_axis',(0.,0.,-1.));
#45777=DIRECTION('center_axis',(1.,0.,0.));
#45778=DIRECTION('ref_axis',(0.,0.,1.));
#45779=DIRECTION('center_axis',(-1.,0.,0.));
#45780=DIRECTION('ref_axis',(0.,0.,1.));
#45781=DIRECTION('center_axis',(0.,0.776999497433153,-0.629501216034272));
#45782=DIRECTION('ref_axis',(-1.,0.,0.));
#45783=DIRECTION('',(-1.,0.,0.));
#45784=DIRECTION('center_axis',(1.,0.,0.));
#45785=DIRECTION('ref_axis',(0.,0.,-1.));
#45786=DIRECTION('center_axis',(-1.,0.,0.));
#45787=DIRECTION('ref_axis',(0.,0.,-1.));
#45788=DIRECTION('',(1.,0.,0.));
#45789=DIRECTION('center_axis',(-1.,0.,0.));
#45790=DIRECTION('ref_axis',(0.,0.,1.));
#45791=DIRECTION('',(-1.,0.,0.));
#45792=DIRECTION('center_axis',(-1.,0.,0.));
#45793=DIRECTION('ref_axis',(0.,0.,1.));
#45794=DIRECTION('',(1.,0.,0.));
#45795=DIRECTION('center_axis',(-1.,0.,0.));
#45796=DIRECTION('ref_axis',(0.,0.,1.));
#45797=DIRECTION('',(-1.,0.,0.));
#45798=DIRECTION('center_axis',(-1.,0.,0.));
#45799=DIRECTION('ref_axis',(0.,0.,-1.));
#45800=DIRECTION('center_axis',(-1.,0.,0.));
#45801=DIRECTION('ref_axis',(0.,0.,-1.));
#45802=DIRECTION('center_axis',(-1.,0.,0.));
#45803=DIRECTION('ref_axis',(0.,0.,1.));
#45804=DIRECTION('center_axis',(1.,0.,0.));
#45805=DIRECTION('ref_axis',(0.,0.,-1.));
#45806=DIRECTION('center_axis',(1.,0.,0.));
#45807=DIRECTION('ref_axis',(0.,0.,-1.));
#45808=DIRECTION('center_axis',(0.707106781186546,-0.353553390593275,-0.612372435695796));
#45809=DIRECTION('ref_axis',(-0.654653670707979,0.,-0.755928946018453));
#45810=DIRECTION('',(0.,0.866025403784438,-0.5));
#45811=DIRECTION('',(0.,-0.866025403784438,0.5));
#45812=DIRECTION('center_axis',(0.,0.5,-0.866025403784438));
#45813=DIRECTION('ref_axis',(-1.,0.,0.));
#45814=DIRECTION('',(1.,0.,0.));
#45815=DIRECTION('',(-1.,0.,0.));
#45816=DIRECTION('center_axis',(0.,0.86602540378444,-0.499999999999997));
#45817=DIRECTION('ref_axis',(0.,0.499999999999997,0.86602540378444));
#45818=DIRECTION('',(1.,0.,0.));
#45819=DIRECTION('center_axis',(-1.,0.,0.));
#45820=DIRECTION('ref_axis',(0.,1.,0.));
#45821=DIRECTION('center_axis',(1.,0.,0.));
#45822=DIRECTION('ref_axis',(0.,1.,0.));
#45823=DIRECTION('center_axis',(0.,1.,-3.16103455295928E-16));
#45824=DIRECTION('ref_axis',(0.,3.16103455295928E-16,1.));
#45825=DIRECTION('',(-1.,0.,0.));
#45826=DIRECTION('',(0.,3.16103455295928E-16,1.));
#45827=DIRECTION('',(-1.,0.,0.));
#45828=DIRECTION('center_axis',(0.550547030005203,-0.648642404490973,-0.525510227158919));
#45829=DIRECTION('ref_axis',(-0.690467539500804,0.,-0.723363378182574));
#45830=DIRECTION('',(0.,-0.629501216034272,0.776999497433153));
#45831=DIRECTION('',(0.701026414838314,0.701026414838313,-0.130858440300507));
#45832=DIRECTION('center_axis',(0.550547030005205,-0.130784004422669,-0.824495913840462));
#45833=DIRECTION('ref_axis',(-0.831638955930083,0.,-0.555316708716316));
#45834=DIRECTION('',(0.,-0.987651911521988,0.156664296082301));
#45835=DIRECTION('',(-0.701026414838315,0.463839941019,-0.541677463823657));
#45836=DIRECTION('center_axis',(0.,-0.156664296082301,-0.987651911521988));
#45837=DIRECTION('ref_axis',(-1.,0.,0.));
#45838=DIRECTION('',(1.,0.,0.));
#45839=DIRECTION('center_axis',(0.550547030005202,-0.77942640891364,0.298985686681551));
#45840=DIRECTION('ref_axis',(0.477236470436039,0.,-0.878774915029868));
#45841=DIRECTION('',(0.,0.358150695487721,0.93366379351545));
#45842=DIRECTION('',(0.701026414838314,0.237186473819303,-0.672535904124163));
#45843=DIRECTION('center_axis',(0.707106781186546,-0.353553390593274,0.612372435695796));
#45844=DIRECTION('ref_axis',(0.654653670707978,0.,-0.755928946018453));
#45845=DIRECTION('',(0.,-0.866025403784439,-0.499999999999999));
#45846=DIRECTION('',(0.,0.866025403784439,0.499999999999999));
#45847=DIRECTION('center_axis',(0.,-0.933663793515451,0.358150695487721));
#45848=DIRECTION('ref_axis',(0.,-0.358150695487721,-0.93366379351545));
#45849=DIRECTION('',(-1.,0.,0.));
#45850=DIRECTION('center_axis',(1.,0.,0.));
#45851=DIRECTION('ref_axis',(0.,0.,1.));
#45852=DIRECTION('center_axis',(1.,0.,0.));
#45853=DIRECTION('ref_axis',(0.,0.,1.));
#45854=DIRECTION('center_axis',(0.707106781186547,0.353553390593274,-0.612372435695795));
#45855=DIRECTION('ref_axis',(-0.654653670707978,0.,-0.755928946018454));
#45856=DIRECTION('',(0.,-0.866025403784439,-0.499999999999999));
#45857=DIRECTION('',(0.,0.866025403784439,0.499999999999999));
#45858=DIRECTION('center_axis',(1.,0.,0.));
#45859=DIRECTION('ref_axis',(0.,0.,1.));
#45860=DIRECTION('center_axis',(1.,0.,0.));
#45861=DIRECTION('ref_axis',(0.,0.,1.));
#45862=DIRECTION('center_axis',(0.707106781186547,-0.707106781186548,0.));
#45863=DIRECTION('ref_axis',(0.,0.,-1.));
#45864=DIRECTION('',(0.,0.,1.));
#45865=DIRECTION('center_axis',(0.,-0.776999497433153,-0.629501216034272));
#45866=DIRECTION('ref_axis',(-1.,0.,0.));
#45867=DIRECTION('center_axis',(1.,0.,0.));
#45868=DIRECTION('ref_axis',(0.,0.,1.));
#45869=DIRECTION('center_axis',(1.,0.,0.));
#45870=DIRECTION('ref_axis',(0.,0.,1.));
#45871=DIRECTION('center_axis',(0.,0.5,0.866025403784438));
#45872=DIRECTION('ref_axis',(0.,0.866025403784438,-0.5));
#45873=DIRECTION('center_axis',(-1.,0.,0.));
#45874=DIRECTION('ref_axis',(0.,0.,1.));
#45875=DIRECTION('center_axis',(0.,1.,4.44089209850062E-15));
#45876=DIRECTION('ref_axis',(0.,-4.44089209850062E-15,1.));
#45877=DIRECTION('',(-1.,0.,0.));
#45878=DIRECTION('',(-0.654653670707976,-3.35699888340126E-15,0.755928946018456));
#45879=DIRECTION('center_axis',(0.54775000523585,0.72455327535185,0.418321028566618));
#45880=DIRECTION('ref_axis',(0.60694953464716,0.,-0.794740374205058));
#45881=DIRECTION('',(0.,0.500000000000002,-0.866025403784437));
#45882=DIRECTION('',(-0.67749794402081,0.0907675134870587,0.729902592366236));
#45883=DIRECTION('',(0.677497944020809,-0.677497944020809,0.286344323664976));
#45884=DIRECTION('center_axis',(0.707106781186547,0.353553390593274,0.612372435695795));
#45885=DIRECTION('ref_axis',(0.654653670707978,0.,-0.755928946018454));
#45886=DIRECTION('',(0.,0.866025403784439,-0.5));
#45887=DIRECTION('',(0.654653670707978,-0.654653670707977,-0.377964473009226));
#45888=DIRECTION('center_axis',(0.,0.499999999999999,0.866025403784439));
#45889=DIRECTION('ref_axis',(1.,0.,0.));
#45890=DIRECTION('',(1.,0.,0.));
#45891=DIRECTION('',(0.654653670707977,-0.654653670707977,0.377964473009228));
#45892=DIRECTION('center_axis',(0.707106781186548,0.707106781186548,-2.2351889679625E-16));
#45893=DIRECTION('ref_axis',(-3.16103455295928E-16,0.,-1.));
#45894=DIRECTION('',(0.,-3.16103455295928E-16,-1.));
#45895=DIRECTION('',(-0.654653670707977,0.654653670707977,0.377964473009227));
#45896=DIRECTION('center_axis',(0.,0.866025403784437,0.500000000000002));
#45897=DIRECTION('ref_axis',(1.,0.,0.));
#45898=DIRECTION('center_axis',(-1.,0.,0.));
#45899=DIRECTION('ref_axis',(0.,1.,0.));
#45900=DIRECTION('center_axis',(1.,0.,0.));
#45901=DIRECTION('ref_axis',(0.,1.,0.));
#45902=DIRECTION('center_axis',(-1.,0.,0.));
#45903=DIRECTION('ref_axis',(0.,1.,0.));
#45904=DIRECTION('center_axis',(1.,0.,0.));
#45905=DIRECTION('ref_axis',(0.,1.,0.));
#45906=DIRECTION('',(0.732793491626298,0.680451099367279,8.33312260816436E-17));
#45907=DIRECTION('center_axis',(0.,0.499999999999999,-0.866025403784439));
#45908=DIRECTION('ref_axis',(0.,-0.866025403784439,-0.499999999999999));
#45909=DIRECTION('',(0.,-0.866025403784439,-0.499999999999999));
#45910=DIRECTION('center_axis',(0.,-0.499999999999999,0.866025403784439));
#45911=DIRECTION('ref_axis',(0.,0.866025403784439,0.499999999999999));
#45912=DIRECTION('',(0.,0.866025403784439,0.499999999999999));
#45913=DIRECTION('center_axis',(-1.,0.,0.));
#45914=DIRECTION('ref_axis',(0.,0.866025403784439,0.499999999999999));
#45915=DIRECTION('center_axis',(1.,0.,0.));
#45916=DIRECTION('ref_axis',(0.,0.,-1.));
#45917=DIRECTION('center_axis',(1.,0.,0.));
#45918=DIRECTION('ref_axis',(0.,0.,-1.));
#45919=DIRECTION('center_axis',(0.,-1.,1.22464679914735E-16));
#45920=DIRECTION('ref_axis',(0.,1.22464679914735E-16,1.));
#45921=DIRECTION('',(0.,1.22464679914735E-16,1.));
#45922=DIRECTION('center_axis',(-1.,0.,0.));
#45923=DIRECTION('ref_axis',(0.,-1.22464679914735E-16,-1.));
#45924=DIRECTION('center_axis',(0.,0.5,-0.866025403784439));
#45925=DIRECTION('ref_axis',(0.,-0.866025403784439,-0.5));
#45926=DIRECTION('center_axis',(0.,-1.,-2.10735636863952E-16));
#45927=DIRECTION('ref_axis',(0.,2.10735636863952E-16,-1.));
#45928=DIRECTION('center_axis',(1.,0.,0.));
#45929=DIRECTION('ref_axis',(0.,0.,-1.));
#45930=DIRECTION('axis',(0.,0.,1.));
#45931=DIRECTION('refdir',(1.,0.,0.));
#45932=DIRECTION('center_axis',(0.,0.,-1.));
#45933=DIRECTION('ref_axis',(-1.,-9.30527706900849E-13,0.));
#45934=DIRECTION('center_axis',(0.,0.,1.));
#45935=DIRECTION('ref_axis',(-2.22044604925031E-16,1.,0.));
#45936=DIRECTION('center_axis',(0.,0.,1.));
#45937=DIRECTION('ref_axis',(-2.22044604925031E-16,1.,0.));
#45938=DIRECTION('center_axis',(0.,0.,-1.));
#45939=DIRECTION('ref_axis',(-2.22044604925031E-16,1.,0.));
#45940=DIRECTION('center_axis',(0.,0.,1.));
#45941=DIRECTION('ref_axis',(-2.22044604925031E-16,1.,0.));
#45942=DIRECTION('',(0.,0.,-1.));
#45943=DIRECTION('center_axis',(0.,0.,1.));
#45944=DIRECTION('ref_axis',(-2.22044604925031E-16,1.,0.));
#45945=DIRECTION('',(0.,0.,1.));
#45946=DIRECTION('center_axis',(0.,0.,-1.));
#45947=DIRECTION('ref_axis',(-2.22044604925031E-16,1.,0.));
#45948=DIRECTION('',(0.,0.,-1.));
#45949=DIRECTION('center_axis',(0.,0.,1.));
#45950=DIRECTION('ref_axis',(-2.22044604925031E-16,1.,0.));
#45951=DIRECTION('',(0.,0.,1.));
#45952=DIRECTION('center_axis',(0.,0.,-1.));
#45953=DIRECTION('ref_axis',(-2.22044604925031E-16,1.,0.));
#45954=DIRECTION('',(0.,0.,-1.));
#45955=DIRECTION('center_axis',(0.,0.,1.));
#45956=DIRECTION('ref_axis',(-2.22044604925031E-16,1.,0.));
#45957=DIRECTION('center_axis',(-0.660321146702944,-0.750983344167439,0.));
#45958=DIRECTION('ref_axis',(0.,0.,1.));
#45959=DIRECTION('',(0.750983344167439,-0.660321146702944,0.));
#45960=DIRECTION('',(0.,0.,-1.));
#45961=DIRECTION('',(0.600503115876144,-0.528007590519368,-0.600503115876158));
#45962=DIRECTION('center_axis',(0.,0.,1.));
#45963=DIRECTION('ref_axis',(-2.22044604925031E-16,1.,0.));
#45964=DIRECTION('center_axis',(0.,0.,1.));
#45965=DIRECTION('ref_axis',(-2.22044604925031E-16,1.,0.));
#45966=DIRECTION('center_axis',(-0.707106781186555,0.,-0.70710678118654));
#45967=DIRECTION('ref_axis',(-0.70710678118654,0.,0.707106781186555));
#45968=DIRECTION('',(0.,1.,0.));
#45969=DIRECTION('',(-0.600503115876144,-0.528007590519368,0.600503115876158));
#45970=DIRECTION('',(0.,-1.,0.));
#45971=DIRECTION('center_axis',(1.,0.,0.));
#45972=DIRECTION('ref_axis',(0.,0.,-1.));
#45973=DIRECTION('',(0.,1.,0.));
#45974=DIRECTION('',(0.,0.,1.));
#45975=DIRECTION('center_axis',(0.660321146702944,-0.750983344167439,0.));
#45976=DIRECTION('ref_axis',(0.,0.,-1.));
#45977=DIRECTION('',(0.600503115876144,0.528007590519368,0.600503115876158));
#45978=DIRECTION('',(0.,0.,1.));
#45979=DIRECTION('',(0.750983344167439,0.660321146702944,0.));
#45980=DIRECTION('center_axis',(-1.,0.,0.));
#45981=DIRECTION('ref_axis',(0.,0.,1.));
#45982=DIRECTION('',(0.,-1.,0.));
#45983=DIRECTION('',(0.,0.,-1.));
#45984=DIRECTION('',(0.,-1.,0.));
#45985=DIRECTION('center_axis',(0.707106781186555,0.,-0.70710678118654));
#45986=DIRECTION('ref_axis',(-0.70710678118654,0.,-0.707106781186555));
#45987=DIRECTION('',(0.,1.,0.));
#45988=DIRECTION('',(-0.600503115876144,0.528007590519368,-0.600503115876158));
#45989=DIRECTION('center_axis',(0.660321146702944,0.750983344167439,0.));
#45990=DIRECTION('ref_axis',(0.,0.,-1.));
#45991=DIRECTION('',(-0.750983344167439,0.660321146702944,0.));
#45992=DIRECTION('center_axis',(-0.660321146702944,0.750983344167439,0.));
#45993=DIRECTION('ref_axis',(0.,0.,1.));
#45994=DIRECTION('',(-0.750983344167439,-0.660321146702944,0.));
#45995=DIRECTION('center_axis',(0.,0.,1.));
#45996=DIRECTION('ref_axis',(-2.22044604925031E-16,1.,0.));
#45997=DIRECTION('center_axis',(0.,0.,1.));
#45998=DIRECTION('ref_axis',(-2.22044604925031E-16,1.,0.));
#45999=DIRECTION('center_axis',(0.,0.,1.));
#46000=DIRECTION('ref_axis',(-2.22044604925031E-16,1.,0.));
#46001=DIRECTION('center_axis',(0.,0.,1.));
#46002=DIRECTION('ref_axis',(-2.22044604925031E-16,1.,0.));
#46003=DIRECTION('center_axis',(0.,0.,1.));
#46004=DIRECTION('ref_axis',(1.,0.,0.));
#46005=DIRECTION('center_axis',(0.,-1.,0.));
#46006=DIRECTION('ref_axis',(0.,0.,-1.));
#46007=DIRECTION('center_axis',(-1.,0.,0.));
#46008=DIRECTION('ref_axis',(0.,0.,1.));
#46009=DIRECTION('center_axis',(0.,1.,0.));
#46010=DIRECTION('ref_axis',(0.,0.,-1.));
#46011=DIRECTION('center_axis',(0.,0.,1.));
#46012=DIRECTION('ref_axis',(-2.22044604925031E-16,1.,0.));
#46013=DIRECTION('axis',(0.,0.,1.));
#46014=DIRECTION('refdir',(1.,0.,0.));
#46015=DIRECTION('center_axis',(-1.,0.,-2.35987854673648E-16));
#46016=DIRECTION('ref_axis',(0.,-1.,-6.12323399573677E-17));
#46017=DIRECTION('center_axis',(-1.,0.,0.));
#46018=DIRECTION('ref_axis',(0.,-1.,-6.12323399573677E-17));
#46019=DIRECTION('center_axis',(-1.,0.,0.));
#46020=DIRECTION('ref_axis',(0.,-1.,-6.12323399573677E-17));
#46021=DIRECTION('',(-0.251155487883568,0.967946755201941,1.18539289550312E-16));
#46022=DIRECTION('center_axis',(1.,0.,0.));
#46023=DIRECTION('ref_axis',(0.,-1.,-6.12323399573677E-17));
#46024=DIRECTION('center_axis',(1.,0.,0.));
#46025=DIRECTION('ref_axis',(0.,-1.,-6.12323399573677E-17));
#46026=DIRECTION('center_axis',(-1.,0.,0.));
#46027=DIRECTION('ref_axis',(0.,1.,0.));
#46028=DIRECTION('',(-0.378632845720504,-0.925546956205677,-1.13346811737786E-16));
#46029=DIRECTION('center_axis',(-1.,0.,0.));
#46030=DIRECTION('ref_axis',(0.,-1.,-6.12323399573677E-17));
#46031=DIRECTION('center_axis',(-1.,0.,0.));
#46032=DIRECTION('ref_axis',(0.,-1.,-6.12323399573677E-17));
#46033=DIRECTION('center_axis',(-1.,0.,0.));
#46034=DIRECTION('ref_axis',(0.,1.,0.));
#46035=DIRECTION('center_axis',(1.,0.,0.));
#46036=DIRECTION('ref_axis',(0.,0.,-1.));
#46037=DIRECTION('',(-0.119145220618432,-0.992876838486922,-1.21592344220055E-16));
#46038=DIRECTION('center_axis',(-1.,0.,-9.20765957170186E-17));
#46039=DIRECTION('ref_axis',(0.,-1.,-6.12323399573676E-17));
#46040=DIRECTION('',(-0.553747832388229,0.832684416886336,1.01974430583973E-16));
#46041=DIRECTION('center_axis',(1.,0.,0.));
#46042=DIRECTION('ref_axis',(0.,-1.,-6.12323399573676E-17));
#46043=DIRECTION('center_axis',(1.,0.,0.));
#46044=DIRECTION('ref_axis',(0.,-1.,-6.12323399573676E-17));
#46045=DIRECTION('center_axis',(-1.,0.,0.));
#46046=DIRECTION('ref_axis',(0.,1.,0.));
#46047=DIRECTION('',(-0.707106781186548,-0.707106781186548,-8.65956056235494E-17));
#46048=DIRECTION('center_axis',(-1.,0.,0.));
#46049=DIRECTION('ref_axis',(0.,-1.,-6.12323399573677E-17));
#46050=DIRECTION('center_axis',(-1.,0.,0.));
#46051=DIRECTION('ref_axis',(0.,-1.,-6.12323399573677E-17));
#46052=DIRECTION('center_axis',(-1.,0.,-3.89966131806063E-17));
#46053=DIRECTION('ref_axis',(0.,-1.,-6.12323399573677E-17));
#46054=DIRECTION('',(-0.843470647186707,0.537175266867749,6.57849971150714E-17));
#46055=DIRECTION('center_axis',(1.,0.,0.));
#46056=DIRECTION('ref_axis',(0.,-1.,-6.12323399573676E-17));
#46057=DIRECTION('center_axis',(1.,0.,0.));
#46058=DIRECTION('ref_axis',(0.,-1.,-6.12323399573676E-17));
#46059=DIRECTION('center_axis',(-1.,0.,0.));
#46060=DIRECTION('ref_axis',(0.,1.,0.));
#46061=DIRECTION('',(-0.939793423488437,-0.341743063086705,-4.18514548339945E-17));
#46062=DIRECTION('center_axis',(-1.,0.,0.));
#46063=DIRECTION('ref_axis',(0.,-1.,-6.12323399573677E-17));
#46064=DIRECTION('center_axis',(-1.,0.,0.));
#46065=DIRECTION('ref_axis',(0.,-1.,-6.12323399573677E-17));
#46066=DIRECTION('center_axis',(-1.,0.,1.60541325725285E-15));
#46067=DIRECTION('ref_axis',(0.,-1.,-3.05136514366029E-17));
#46068=DIRECTION('',(-0.984833342116431,0.173502992065788,1.60760670182904E-15));
#46069=DIRECTION('center_axis',(1.,0.,0.));
#46070=DIRECTION('ref_axis',(0.,-1.,0.));
#46071=DIRECTION('center_axis',(1.,0.,0.));
#46072=DIRECTION('ref_axis',(0.,-1.,0.));
#46073=DIRECTION('center_axis',(1.,0.,0.));
#46074=DIRECTION('ref_axis',(0.,1.,0.));
#46075=DIRECTION('',(-1.,0.,0.));
#46076=DIRECTION('center_axis',(1.,0.,0.));
#46077=DIRECTION('ref_axis',(0.,0.,-1.));
#46078=DIRECTION('center_axis',(-1.,0.,0.));
#46079=DIRECTION('ref_axis',(0.,0.,1.));
#46080=DIRECTION('center_axis',(1.,0.,0.));
#46081=DIRECTION('ref_axis',(0.,0.,-1.));
#46082=DIRECTION('center_axis',(1.,0.,0.));
#46083=DIRECTION('ref_axis',(0.,0.,-1.));
#46084=DIRECTION('center_axis',(1.,0.,0.));
#46085=DIRECTION('ref_axis',(0.,1.,0.));
#46086=DIRECTION('center_axis',(1.,0.,0.));
#46087=DIRECTION('ref_axis',(0.,0.,-1.));
#46088=DIRECTION('',(-0.707106781186547,0.707106781186547,8.65956056235493E-17));
#46089=DIRECTION('center_axis',(1.,0.,0.));
#46090=DIRECTION('ref_axis',(0.,1.,0.));
#46091=DIRECTION('center_axis',(1.,0.,0.));
#46092=DIRECTION('ref_axis',(0.,0.,-1.));
#46093=DIRECTION('',(-1.,0.,0.));
#46094=DIRECTION('center_axis',(-1.,0.,0.));
#46095=DIRECTION('ref_axis',(0.,0.,1.));
#46096=DIRECTION('center_axis',(1.,0.,0.));
#46097=DIRECTION('ref_axis',(0.,0.,-1.));
#46098=DIRECTION('center_axis',(1.,0.,0.));
#46099=DIRECTION('ref_axis',(0.,1.,0.));
#46100=DIRECTION('center_axis',(1.,0.,0.));
#46101=DIRECTION('ref_axis',(0.,0.,-1.));
#46102=DIRECTION('',(-1.,0.,0.));
#46103=DIRECTION('center_axis',(-1.,0.,0.));
#46104=DIRECTION('ref_axis',(0.,1.,0.));
#46105=DIRECTION('',(-0.316227766016838,-0.948683298050514,-1.16180196436212E-16));
#46106=DIRECTION('center_axis',(1.,0.,0.));
#46107=DIRECTION('ref_axis',(0.,0.,-1.));
#46108=DIRECTION('center_axis',(-1.,0.,0.));
#46109=DIRECTION('ref_axis',(0.,0.,1.));
#46110=DIRECTION('center_axis',(1.,0.,0.));
#46111=DIRECTION('ref_axis',(0.,0.,-1.));
#46112=DIRECTION('center_axis',(-1.,0.,0.));
#46113=DIRECTION('ref_axis',(0.,1.,0.));
#46114=DIRECTION('',(-0.129339184067768,-0.991600411186222,-1.21436026959241E-16));
#46115=DIRECTION('center_axis',(1.,0.,0.));
#46116=DIRECTION('ref_axis',(0.,0.,-1.));
#46117=DIRECTION('center_axis',(-1.,0.,0.));
#46118=DIRECTION('ref_axis',(0.,1.,0.));
#46119=DIRECTION('',(-0.388057000058132,-0.921635375138065,-1.1286778121438E-16));
#46120=DIRECTION('center_axis',(1.,0.,0.));
#46121=DIRECTION('ref_axis',(0.,0.,-1.));
#46122=DIRECTION('center_axis',(-1.,0.,0.));
#46123=DIRECTION('ref_axis',(0.,1.,0.));
#46124=DIRECTION('',(-0.73105526824287,-0.68231825036001,-8.35598861303209E-17));
#46125=DIRECTION('center_axis',(1.,0.,0.));
#46126=DIRECTION('ref_axis',(0.,0.,-1.));
#46127=DIRECTION('center_axis',(-1.,0.,0.));
#46128=DIRECTION('ref_axis',(0.,1.,0.));
#46129=DIRECTION('',(-0.913811548620257,-0.406138466053448,-4.97376172462971E-17));
#46130=DIRECTION('center_axis',(1.,0.,0.));
#46131=DIRECTION('ref_axis',(0.,0.,-1.));
#46132=DIRECTION('center_axis',(1.,0.,0.));
#46133=DIRECTION('ref_axis',(0.,1.,0.));
#46134=DIRECTION('',(-0.999652397241505,0.0263644588283474,3.22871501153878E-18));
#46135=DIRECTION('center_axis',(1.,0.,0.));
#46136=DIRECTION('ref_axis',(0.,0.,-1.));
#46137=DIRECTION('center_axis',(1.,0.,0.));
#46138=DIRECTION('ref_axis',(0.,1.,0.));
#46139=DIRECTION('',(-1.,0.,0.));
#46140=DIRECTION('axis',(0.,0.,1.));
#46141=DIRECTION('refdir',(1.,0.,0.));
#46142=DIRECTION('center_axis',(1.,0.,0.));
#46143=DIRECTION('ref_axis',(0.,1.,0.));
#46144=DIRECTION('',(-1.,0.,0.));
#46145=DIRECTION('center_axis',(-1.,0.,0.));
#46146=DIRECTION('ref_axis',(0.,1.,0.));
#46147=DIRECTION('center_axis',(1.,0.,0.));
#46148=DIRECTION('ref_axis',(0.,1.,0.));
#46149=DIRECTION('',(-1.,0.,0.));
#46150=DIRECTION('center_axis',(1.,0.,0.));
#46151=DIRECTION('ref_axis',(0.,1.,0.));
#46152=DIRECTION('',(-1.,0.,0.));
#46153=DIRECTION('center_axis',(1.,0.,0.));
#46154=DIRECTION('ref_axis',(0.,1.,0.));
#46155=DIRECTION('',(-1.,0.,0.));
#46156=DIRECTION('center_axis',(1.,0.,0.));
#46157=DIRECTION('ref_axis',(0.,1.,0.));
#46158=DIRECTION('',(-1.,0.,0.));
#46159=DIRECTION('center_axis',(1.,0.,0.));
#46160=DIRECTION('ref_axis',(0.,1.,0.));
#46161=DIRECTION('',(-1.,0.,0.));
#46162=DIRECTION('center_axis',(1.,0.,0.));
#46163=DIRECTION('ref_axis',(0.,1.,0.));
#46164=DIRECTION('',(-1.,0.,0.));
#46165=DIRECTION('center_axis',(1.,0.,0.));
#46166=DIRECTION('ref_axis',(0.,1.,0.));
#46167=DIRECTION('',(-1.,0.,0.));
#46168=DIRECTION('center_axis',(1.,0.,0.));
#46169=DIRECTION('ref_axis',(0.,1.,0.));
#46170=DIRECTION('',(-1.,0.,0.));
#46171=DIRECTION('center_axis',(1.,0.,0.));
#46172=DIRECTION('ref_axis',(0.,1.,0.));
#46173=DIRECTION('',(-1.,0.,0.));
#46174=DIRECTION('center_axis',(1.,0.,0.));
#46175=DIRECTION('ref_axis',(0.,1.,0.));
#46176=DIRECTION('',(-1.,0.,0.));
#46177=DIRECTION('center_axis',(1.,0.,0.));
#46178=DIRECTION('ref_axis',(0.,1.,0.));
#46179=DIRECTION('',(-1.,0.,0.));
#46180=DIRECTION('center_axis',(1.,0.,0.));
#46181=DIRECTION('ref_axis',(0.,1.,0.));
#46182=DIRECTION('',(-1.,0.,0.));
#46183=DIRECTION('center_axis',(1.,0.,0.));
#46184=DIRECTION('ref_axis',(0.,1.,0.));
#46185=DIRECTION('',(-1.,0.,0.));
#46186=DIRECTION('center_axis',(1.,0.,0.));
#46187=DIRECTION('ref_axis',(0.,1.,0.));
#46188=DIRECTION('',(-1.,0.,0.));
#46189=DIRECTION('center_axis',(1.,0.,0.));
#46190=DIRECTION('ref_axis',(0.,1.,0.));
#46191=DIRECTION('',(-1.,0.,0.));
#46192=DIRECTION('center_axis',(1.,0.,0.));
#46193=DIRECTION('ref_axis',(0.,1.,0.));
#46194=DIRECTION('',(-1.,0.,0.));
#46195=DIRECTION('center_axis',(1.,0.,0.));
#46196=DIRECTION('ref_axis',(0.,1.,0.));
#46197=DIRECTION('',(-1.,0.,0.));
#46198=DIRECTION('center_axis',(1.,0.,0.));
#46199=DIRECTION('ref_axis',(0.,1.,0.));
#46200=DIRECTION('',(-1.,0.,0.));
#46201=DIRECTION('center_axis',(1.,0.,0.));
#46202=DIRECTION('ref_axis',(0.,1.,0.));
#46203=DIRECTION('',(-1.,0.,0.));
#46204=DIRECTION('center_axis',(1.,0.,0.));
#46205=DIRECTION('ref_axis',(0.,1.,0.));
#46206=DIRECTION('',(-1.,0.,0.));
#46207=DIRECTION('center_axis',(1.,0.,0.));
#46208=DIRECTION('ref_axis',(0.,1.,0.));
#46209=DIRECTION('',(-1.,0.,0.));
#46210=DIRECTION('center_axis',(1.,0.,0.));
#46211=DIRECTION('ref_axis',(0.,1.,0.));
#46212=DIRECTION('',(-1.,0.,0.));
#46213=DIRECTION('center_axis',(1.,0.,0.));
#46214=DIRECTION('ref_axis',(0.,1.,0.));
#46215=DIRECTION('',(-1.,0.,0.));
#46216=DIRECTION('center_axis',(1.,0.,0.));
#46217=DIRECTION('ref_axis',(0.,1.,0.));
#46218=DIRECTION('',(-1.,0.,0.));
#46219=DIRECTION('center_axis',(1.,0.,0.));
#46220=DIRECTION('ref_axis',(0.,1.,0.));
#46221=DIRECTION('',(-1.,0.,0.));
#46222=DIRECTION('center_axis',(1.,0.,0.));
#46223=DIRECTION('ref_axis',(0.,1.,0.));
#46224=DIRECTION('',(-1.,0.,0.));
#46225=DIRECTION('center_axis',(1.,0.,0.));
#46226=DIRECTION('ref_axis',(0.,1.,0.));
#46227=DIRECTION('',(-1.,0.,0.));
#46228=DIRECTION('center_axis',(1.,0.,0.));
#46229=DIRECTION('ref_axis',(0.,1.,0.));
#46230=DIRECTION('',(-1.,0.,0.));
#46231=DIRECTION('center_axis',(1.,0.,0.));
#46232=DIRECTION('ref_axis',(0.,1.,-9.17622152879152E-14));
#46233=DIRECTION('',(1.,0.,0.));
#46234=DIRECTION('center_axis',(1.,0.,0.));
#46235=DIRECTION('ref_axis',(0.,1.,-9.17622152879152E-14));
#46236=DIRECTION('center_axis',(1.,0.,0.));
#46237=DIRECTION('ref_axis',(0.,1.,-9.17622152879152E-14));
#46238=DIRECTION('',(1.,0.,0.));
#46239=DIRECTION('center_axis',(1.,0.,0.));
#46240=DIRECTION('ref_axis',(0.,1.,-9.17622152879152E-14));
#46241=DIRECTION('center_axis',(1.,0.,0.));
#46242=DIRECTION('ref_axis',(0.,1.,-9.17622152879152E-14));
#46243=DIRECTION('',(1.,0.,0.));
#46244=DIRECTION('center_axis',(1.,0.,0.));
#46245=DIRECTION('ref_axis',(0.,1.,-9.17622152879152E-14));
#46246=DIRECTION('',(1.,0.,0.));
#46247=DIRECTION('center_axis',(1.,0.,0.));
#46248=DIRECTION('ref_axis',(0.,1.,-9.17622152879152E-14));
#46249=DIRECTION('',(1.,0.,0.));
#46250=DIRECTION('center_axis',(1.,0.,0.));
#46251=DIRECTION('ref_axis',(0.,1.,-9.17622152879152E-14));
#46252=DIRECTION('',(1.,0.,0.));
#46253=DIRECTION('center_axis',(1.,0.,0.));
#46254=DIRECTION('ref_axis',(0.,1.,-9.17622152879152E-14));
#46255=DIRECTION('',(1.,0.,0.));
#46256=DIRECTION('center_axis',(1.,0.,0.));
#46257=DIRECTION('ref_axis',(0.,1.,-9.17622152879152E-14));
#46258=DIRECTION('',(1.,0.,0.));
#46259=DIRECTION('center_axis',(1.,0.,0.));
#46260=DIRECTION('ref_axis',(0.,1.,-9.17622152879152E-14));
#46261=DIRECTION('',(1.,0.,0.));
#46262=DIRECTION('center_axis',(1.,0.,0.));
#46263=DIRECTION('ref_axis',(0.,1.,-9.17622152879152E-14));
#46264=DIRECTION('',(1.,0.,0.));
#46265=DIRECTION('center_axis',(1.,0.,0.));
#46266=DIRECTION('ref_axis',(0.,1.,-9.17622152879152E-14));
#46267=DIRECTION('',(1.,0.,0.));
#46268=DIRECTION('center_axis',(1.,0.,0.));
#46269=DIRECTION('ref_axis',(0.,1.,-9.17622152879152E-14));
#46270=DIRECTION('',(1.,0.,0.));
#46271=DIRECTION('center_axis',(1.,0.,0.));
#46272=DIRECTION('ref_axis',(0.,1.,-9.17622152879152E-14));
#46273=DIRECTION('',(1.,0.,0.));
#46274=DIRECTION('center_axis',(1.,0.,0.));
#46275=DIRECTION('ref_axis',(0.,1.,-9.17622152879152E-14));
#46276=DIRECTION('',(1.,0.,0.));
#46277=DIRECTION('center_axis',(1.,0.,0.));
#46278=DIRECTION('ref_axis',(0.,1.,-9.17622152879152E-14));
#46279=DIRECTION('',(1.,0.,0.));
#46280=DIRECTION('center_axis',(1.,0.,0.));
#46281=DIRECTION('ref_axis',(0.,1.,-9.17622152879152E-14));
#46282=DIRECTION('',(1.,0.,0.));
#46283=DIRECTION('center_axis',(1.,0.,0.));
#46284=DIRECTION('ref_axis',(0.,1.,-9.17622152879152E-14));
#46285=DIRECTION('',(1.,0.,0.));
#46286=DIRECTION('center_axis',(1.,0.,0.));
#46287=DIRECTION('ref_axis',(0.,1.,-9.17622152879152E-14));
#46288=DIRECTION('',(1.,0.,0.));
#46289=DIRECTION('center_axis',(1.,0.,0.));
#46290=DIRECTION('ref_axis',(0.,1.,-9.17622152879152E-14));
#46291=DIRECTION('',(1.,0.,0.));
#46292=DIRECTION('center_axis',(1.,0.,0.));
#46293=DIRECTION('ref_axis',(0.,1.,-9.17622152879152E-14));
#46294=DIRECTION('',(1.,0.,0.));
#46295=DIRECTION('center_axis',(1.,0.,0.));
#46296=DIRECTION('ref_axis',(0.,1.,-9.17622152879152E-14));
#46297=DIRECTION('',(1.,0.,0.));
#46298=DIRECTION('center_axis',(1.,0.,0.));
#46299=DIRECTION('ref_axis',(0.,1.,-9.17622152879152E-14));
#46300=DIRECTION('',(1.,0.,0.));
#46301=DIRECTION('center_axis',(1.,0.,0.));
#46302=DIRECTION('ref_axis',(0.,1.,-9.17622152879152E-14));
#46303=DIRECTION('',(1.,0.,0.));
#46304=DIRECTION('center_axis',(1.,0.,0.));
#46305=DIRECTION('ref_axis',(0.,1.,-9.17622152879152E-14));
#46306=DIRECTION('',(1.,0.,0.));
#46307=DIRECTION('center_axis',(1.,0.,0.));
#46308=DIRECTION('ref_axis',(0.,1.,-9.17622152879152E-14));
#46309=DIRECTION('',(1.,0.,0.));
#46310=DIRECTION('center_axis',(1.,0.,0.));
#46311=DIRECTION('ref_axis',(0.,1.,-9.17622152879152E-14));
#46312=DIRECTION('',(1.,0.,0.));
#46313=DIRECTION('center_axis',(1.,0.,0.));
#46314=DIRECTION('ref_axis',(0.,1.,-9.17622152879152E-14));
#46315=DIRECTION('',(1.,0.,0.));
#46316=DIRECTION('center_axis',(1.,0.,0.));
#46317=DIRECTION('ref_axis',(0.,1.,-9.17622152879152E-14));
#46318=DIRECTION('',(1.,0.,0.));
#46319=DIRECTION('center_axis',(1.,0.,0.));
#46320=DIRECTION('ref_axis',(0.,1.,-9.17622152879152E-14));
#46321=DIRECTION('',(1.,0.,0.));
#46322=DIRECTION('center_axis',(-1.,0.,-1.02244356237877E-15));
#46323=DIRECTION('ref_axis',(0.,-1.,-3.30019287147236E-17));
#46324=DIRECTION('center_axis',(-1.,0.,0.));
#46325=DIRECTION('ref_axis',(0.,-1.,0.));
#46326=DIRECTION('',(-0.382683432365087,0.923879532511288,-2.47639794148994E-16));
#46327=DIRECTION('center_axis',(1.,0.,0.));
#46328=DIRECTION('ref_axis',(0.,-1.,-6.12323399573677E-17));
#46329=DIRECTION('center_axis',(1.,0.,0.));
#46330=DIRECTION('ref_axis',(0.,-1.,-6.12323399573677E-17));
#46331=DIRECTION('center_axis',(-1.,0.,0.));
#46332=DIRECTION('ref_axis',(0.,1.,0.));
#46333=DIRECTION('',(-0.707106781186544,-0.707106781186551,-8.65956056235498E-17));
#46334=DIRECTION('center_axis',(-1.,0.,0.));
#46335=DIRECTION('ref_axis',(0.,1.,0.));
#46336=DIRECTION('center_axis',(-1.,0.,0.));
#46337=DIRECTION('ref_axis',(0.,1.,0.));
#46338=DIRECTION('center_axis',(-1.,0.,0.));
#46339=DIRECTION('ref_axis',(0.,1.,0.));
#46340=DIRECTION('center_axis',(1.,0.,0.));
#46341=DIRECTION('ref_axis',(0.,0.,-1.));
#46342=DIRECTION('center_axis',(0.707106781186548,0.707106781186547,0.));
#46343=DIRECTION('ref_axis',(0.,0.,-1.));
#46344=DIRECTION('',(0.,0.,-1.));
#46345=DIRECTION('',(-0.344817162976176,0.344817162976177,0.873041951016171));
#46346=DIRECTION('',(0.,0.,1.));
#46347=DIRECTION('',(0.344817162976176,-0.344817162976177,0.873041951016171));
#46348=DIRECTION('center_axis',(1.,0.,0.));
#46349=DIRECTION('ref_axis',(0.,0.,-1.));
#46350=DIRECTION('center_axis',(1.,0.,0.));
#46351=DIRECTION('ref_axis',(0.,0.,-1.));
#46352=DIRECTION('center_axis',(1.,0.,0.));
#46353=DIRECTION('ref_axis',(0.,0.,-1.));
#46354=DIRECTION('center_axis',(0.,0.930084132110489,0.367346576404733));
#46355=DIRECTION('ref_axis',(0.,-0.367346576404732,0.930084132110489));
#46356=DIRECTION('',(-1.,0.,0.));
#46357=DIRECTION('',(-0.344817162976176,-0.344817162976177,0.873041951016171));
#46358=DIRECTION('',(1.,0.,0.));
#46359=DIRECTION('center_axis',(1.,0.,0.));
#46360=DIRECTION('ref_axis',(0.,-1.,1.22464679914735E-16));
#46361=DIRECTION('center_axis',(1.,0.,0.));
#46362=DIRECTION('ref_axis',(0.,0.,-1.));
#46363=DIRECTION('',(-1.,0.,0.));
#46364=DIRECTION('center_axis',(1.,0.,0.));
#46365=DIRECTION('ref_axis',(0.,0.,-1.));
#46366=DIRECTION('center_axis',(1.,0.,0.));
#46367=DIRECTION('ref_axis',(0.,-1.,5.66553889764798E-16));
#46368=DIRECTION('center_axis',(1.,0.,0.));
#46369=DIRECTION('ref_axis',(0.,0.,-1.));
#46370=DIRECTION('center_axis',(-0.707106781186548,0.707106781186547,0.));
#46371=DIRECTION('ref_axis',(0.,0.,1.));
#46372=DIRECTION('',(0.,0.,-1.));
#46373=DIRECTION('',(-0.344817162976176,-0.344817162976177,-0.873041951016171));
#46374=DIRECTION('',(0.,0.,1.));
#46375=DIRECTION('center_axis',(0.,-1.,0.));
#46376=DIRECTION('ref_axis',(0.,0.,1.));
#46377=DIRECTION('',(1.,0.,0.));
#46378=DIRECTION('center_axis',(-1.,0.,0.));
#46379=DIRECTION('ref_axis',(0.,0.,1.));
#46380=DIRECTION('center_axis',(0.,0.930084132110489,-0.367346576404733));
#46381=DIRECTION('ref_axis',(0.,0.367346576404732,0.930084132110489));
#46382=DIRECTION('center_axis',(-1.,0.,0.));
#46383=DIRECTION('ref_axis',(0.,-1.,-1.22464679914735E-16));
#46384=DIRECTION('center_axis',(1.,0.,0.));
#46385=DIRECTION('ref_axis',(0.,0.,-1.));
#46386=DIRECTION('center_axis',(1.,0.,0.));
#46387=DIRECTION('ref_axis',(0.,0.,-1.));
#46388=DIRECTION('center_axis',(-1.,0.,0.));
#46389=DIRECTION('ref_axis',(0.,1.,0.));
#46390=DIRECTION('center_axis',(-1.,0.,0.));
#46391=DIRECTION('ref_axis',(0.,1.,0.));
#46392=DIRECTION('center_axis',(-1.,0.,0.));
#46393=DIRECTION('ref_axis',(0.,1.,-9.17622152879152E-14));
#46394=DIRECTION('center_axis',(1.,0.,0.));
#46395=DIRECTION('ref_axis',(0.,0.899731237029652,0.436444384902695));
#46396=DIRECTION('center_axis',(1.,0.,0.));
#46397=DIRECTION('ref_axis',(0.,1.,0.));
#46398=DIRECTION('center_axis',(0.,-0.497058334900004,0.86771712654899));
#46399=DIRECTION('ref_axis',(0.,-0.86771712654899,-0.497058334900004));
#46400=DIRECTION('',(-1.,0.,0.));
#46401=DIRECTION('',(0.,-0.86771712654899,-0.497058334900004));
#46402=DIRECTION('',(1.,0.,0.));
#46403=DIRECTION('',(0.,-0.86771712654899,-0.497058334900004));
#46404=DIRECTION('center_axis',(1.,0.,0.));
#46405=DIRECTION('ref_axis',(0.,-0.17364817766693,-0.984807753012208));
#46406=DIRECTION('center_axis',(-1.,0.,0.));
#46407=DIRECTION('ref_axis',(0.,1.,0.));
#46408=DIRECTION('',(0.,0.64538341780392,-0.763858785394087));
#46409=DIRECTION('center_axis',(0.,-0.763858785394087,-0.645383417803921));
#46410=DIRECTION('ref_axis',(0.,0.64538341780392,-0.763858785394087));
#46411=DIRECTION('',(1.,0.,0.));
#46412=DIRECTION('',(0.,0.64538341780392,-0.763858785394087));
#46413=DIRECTION('center_axis',(1.,0.,0.));
#46414=DIRECTION('ref_axis',(0.,-0.17364817766693,-0.984807753012208));
#46415=DIRECTION('center_axis',(1.,0.,0.));
#46416=DIRECTION('ref_axis',(0.,1.,0.));
#46417=DIRECTION('center_axis',(0.,-0.338829404153244,0.940847827696465));
#46418=DIRECTION('ref_axis',(0.,-0.940847827696465,-0.338829404153244));
#46419=DIRECTION('',(-1.,0.,0.));
#46420=DIRECTION('',(0.,-0.940847827696465,-0.338829404153244));
#46421=DIRECTION('',(1.,0.,0.));
#46422=DIRECTION('',(0.,-0.940847827696465,-0.338829404153244));
#46423=DIRECTION('center_axis',(1.,0.,0.));
#46424=DIRECTION('ref_axis',(0.,-0.342020143325669,-0.939692620785908));
#46425=DIRECTION('center_axis',(-1.,0.,0.));
#46426=DIRECTION('ref_axis',(0.,1.,0.));
#46427=DIRECTION('',(0.,0.502935907440259,-0.864323708460692));
#46428=DIRECTION('center_axis',(0.,-0.864323708460692,-0.502935907440259));
#46429=DIRECTION('ref_axis',(0.,0.502935907440259,-0.864323708460692));
#46430=DIRECTION('',(1.,0.,0.));
#46431=DIRECTION('',(0.,0.502935907440259,-0.864323708460692));
#46432=DIRECTION('center_axis',(1.,0.,0.));
#46433=DIRECTION('ref_axis',(0.,-0.342020143325669,-0.939692620785908));
#46434=DIRECTION('center_axis',(1.,0.,0.));
#46435=DIRECTION('ref_axis',(0.,1.,0.));
#46436=DIRECTION('center_axis',(0.,-0.170305313417241,0.985391343691356));
#46437=DIRECTION('ref_axis',(0.,-0.985391343691356,-0.170305313417241));
#46438=DIRECTION('',(-1.,0.,0.));
#46439=DIRECTION('',(0.,-0.985391343691356,-0.170305313417241));
#46440=DIRECTION('',(1.,0.,0.));
#46441=DIRECTION('',(0.,-0.985391343691356,-0.170305313417241));
#46442=DIRECTION('center_axis',(1.,0.,0.));
#46443=DIRECTION('ref_axis',(0.,-0.5,-0.866025403784438));
#46444=DIRECTION('center_axis',(-1.,0.,0.));
#46445=DIRECTION('ref_axis',(0.,1.,0.));
#46446=DIRECTION('',(0.,0.345206944026876,-0.938526593014618));
#46447=DIRECTION('center_axis',(0.,-0.938526593014618,-0.345206944026876));
#46448=DIRECTION('ref_axis',(0.,0.345206944026876,-0.938526593014618));
#46449=DIRECTION('',(1.,0.,0.));
#46450=DIRECTION('',(0.,0.345206944026876,-0.938526593014618));
#46451=DIRECTION('center_axis',(1.,0.,0.));
#46452=DIRECTION('ref_axis',(0.,-0.5,-0.866025403784438));
#46453=DIRECTION('center_axis',(1.,0.,0.));
#46454=DIRECTION('ref_axis',(0.,1.,0.));
#46455=DIRECTION('center_axis',(0.,0.00339341808829885,0.999994242340264));
#46456=DIRECTION('ref_axis',(0.,-0.999994242340264,0.00339341808829885));
#46457=DIRECTION('',(-1.,0.,0.));
#46458=DIRECTION('',(0.,-0.999994242340264,0.00339341808829885));
#46459=DIRECTION('',(1.,0.,0.));
#46460=DIRECTION('',(0.,-0.999994242340264,0.00339341808829885));
#46461=DIRECTION('center_axis',(1.,0.,0.));
#46462=DIRECTION('ref_axis',(0.,-0.64278760968654,-0.766044443118978));
#46463=DIRECTION('center_axis',(-1.,0.,0.));
#46464=DIRECTION('ref_axis',(0.,1.,0.));
#46465=DIRECTION('',(0.,0.176989042302377,-0.984212821957166));
#46466=DIRECTION('center_axis',(0.,-0.984212821957166,-0.176989042302377));
#46467=DIRECTION('ref_axis',(0.,0.176989042302377,-0.984212821957166));
#46468=DIRECTION('',(1.,0.,0.));
#46469=DIRECTION('',(0.,0.176989042302377,-0.984212821957166));
#46470=DIRECTION('center_axis',(1.,0.,0.));
#46471=DIRECTION('ref_axis',(0.,-0.64278760968654,-0.766044443118978));
#46472=DIRECTION('center_axis',(1.,0.,0.));
#46473=DIRECTION('ref_axis',(0.,1.,0.));
#46474=DIRECTION('center_axis',(0.,0.176989042302378,0.984212821957166));
#46475=DIRECTION('ref_axis',(0.,-0.984212821957165,0.176989042302378));
#46476=DIRECTION('',(-1.,0.,0.));
#46477=DIRECTION('',(0.,-0.984212821957165,0.176989042302378));
#46478=DIRECTION('',(1.,0.,0.));
#46479=DIRECTION('',(0.,-0.984212821957165,0.176989042302378));
#46480=DIRECTION('center_axis',(1.,0.,0.));
#46481=DIRECTION('ref_axis',(0.,-0.766044443118978,-0.642787609686539));
#46482=DIRECTION('center_axis',(-1.,0.,0.));
#46483=DIRECTION('ref_axis',(0.,1.,0.));
#46484=DIRECTION('',(0.,0.00339341808829835,-0.999994242340264));
#46485=DIRECTION('center_axis',(0.,-0.999994242340264,-0.00339341808829835));
#46486=DIRECTION('ref_axis',(0.,0.00339341808829835,-0.999994242340264));
#46487=DIRECTION('',(1.,0.,0.));
#46488=DIRECTION('',(0.,0.00339341808829835,-0.999994242340264));
#46489=DIRECTION('center_axis',(1.,0.,0.));
#46490=DIRECTION('ref_axis',(0.,-0.766044443118978,-0.642787609686539));
#46491=DIRECTION('center_axis',(1.,0.,0.));
#46492=DIRECTION('ref_axis',(0.,1.,0.));
#46493=DIRECTION('center_axis',(0.,0.345206944026876,0.938526593014618));
#46494=DIRECTION('ref_axis',(0.,-0.938526593014617,0.345206944026876));
#46495=DIRECTION('',(-1.,0.,0.));
#46496=DIRECTION('',(0.,-0.938526593014617,0.345206944026876));
#46497=DIRECTION('',(1.,0.,0.));
#46498=DIRECTION('',(0.,-0.938526593014617,0.345206944026876));
#46499=DIRECTION('center_axis',(1.,0.,0.));
#46500=DIRECTION('ref_axis',(0.,-0.866025403784439,-0.5));
#46501=DIRECTION('center_axis',(-1.,0.,0.));
#46502=DIRECTION('ref_axis',(0.,1.,0.));
#46503=DIRECTION('',(0.,-0.170305313417241,-0.985391343691356));
#46504=DIRECTION('center_axis',(0.,-0.985391343691356,0.170305313417241));
#46505=DIRECTION('ref_axis',(0.,-0.170305313417241,-0.985391343691356));
#46506=DIRECTION('',(1.,0.,0.));
#46507=DIRECTION('',(0.,-0.170305313417241,-0.985391343691356));
#46508=DIRECTION('center_axis',(1.,0.,0.));
#46509=DIRECTION('ref_axis',(0.,-0.866025403784439,-0.5));
#46510=DIRECTION('center_axis',(1.,0.,0.));
#46511=DIRECTION('ref_axis',(0.,1.,0.));
#46512=DIRECTION('center_axis',(0.,0.502935907440261,0.864323708460691));
#46513=DIRECTION('ref_axis',(0.,-0.864323708460691,0.502935907440261));
#46514=DIRECTION('',(-1.,0.,0.));
#46515=DIRECTION('',(0.,-0.864323708460691,0.502935907440261));
#46516=DIRECTION('',(1.,0.,0.));
#46517=DIRECTION('',(0.,-0.864323708460691,0.502935907440261));
#46518=DIRECTION('center_axis',(1.,0.,0.));
#46519=DIRECTION('ref_axis',(0.,-0.939692620785909,-0.342020143325668));
#46520=DIRECTION('center_axis',(-1.,0.,0.));
#46521=DIRECTION('ref_axis',(0.,1.,0.));
#46522=DIRECTION('',(0.,-0.338829404153245,-0.940847827696465));
#46523=DIRECTION('center_axis',(0.,-0.940847827696465,0.338829404153246));
#46524=DIRECTION('ref_axis',(0.,-0.338829404153245,-0.940847827696465));
#46525=DIRECTION('',(1.,0.,0.));
#46526=DIRECTION('',(0.,-0.338829404153245,-0.940847827696465));
#46527=DIRECTION('center_axis',(1.,0.,0.));
#46528=DIRECTION('ref_axis',(0.,-0.939692620785909,-0.342020143325668));
#46529=DIRECTION('center_axis',(1.,0.,0.));
#46530=DIRECTION('ref_axis',(0.,1.,0.));
#46531=DIRECTION('center_axis',(0.,0.645383417803921,0.763858785394087));
#46532=DIRECTION('ref_axis',(0.,-0.763858785394087,0.645383417803921));
#46533=DIRECTION('',(-1.,0.,0.));
#46534=DIRECTION('',(0.,-0.763858785394087,0.645383417803921));
#46535=DIRECTION('',(1.,0.,0.));
#46536=DIRECTION('',(0.,-0.763858785394087,0.645383417803921));
#46537=DIRECTION('center_axis',(1.,0.,0.));
#46538=DIRECTION('ref_axis',(0.,-0.984807753012208,-0.17364817766693));
#46539=DIRECTION('center_axis',(-1.,0.,0.));
#46540=DIRECTION('ref_axis',(0.,1.,0.));
#46541=DIRECTION('',(0.,-0.497058334900004,-0.86771712654899));
#46542=DIRECTION('center_axis',(0.,-0.86771712654899,0.497058334900004));
#46543=DIRECTION('ref_axis',(0.,-0.497058334900004,-0.86771712654899));
#46544=DIRECTION('',(1.,0.,0.));
#46545=DIRECTION('',(0.,-0.497058334900004,-0.86771712654899));
#46546=DIRECTION('center_axis',(1.,0.,0.));
#46547=DIRECTION('ref_axis',(0.,-0.984807753012208,-0.17364817766693));
#46548=DIRECTION('center_axis',(1.,0.,0.));
#46549=DIRECTION('ref_axis',(0.,1.,0.));
#46550=DIRECTION('center_axis',(0.,0.768221279597376,0.640184399664479));
#46551=DIRECTION('ref_axis',(0.,-0.640184399664479,0.768221279597376));
#46552=DIRECTION('',(-1.,0.,0.));
#46553=DIRECTION('',(0.,-0.640184399664479,0.768221279597376));
#46554=DIRECTION('',(1.,0.,0.));
#46555=DIRECTION('',(0.,-0.640184399664479,0.768221279597376));
#46556=DIRECTION('center_axis',(1.,0.,0.));
#46557=DIRECTION('ref_axis',(0.,-1.,1.83697019872103E-16));
#46558=DIRECTION('center_axis',(-1.,0.,0.));
#46559=DIRECTION('ref_axis',(0.,1.,0.));
#46560=DIRECTION('',(0.,-0.64018439966448,-0.768221279597376));
#46561=DIRECTION('center_axis',(0.,-0.768221279597376,0.64018439966448));
#46562=DIRECTION('ref_axis',(0.,-0.64018439966448,-0.768221279597376));
#46563=DIRECTION('',(1.,0.,0.));
#46564=DIRECTION('',(0.,-0.64018439966448,-0.768221279597376));
#46565=DIRECTION('center_axis',(1.,0.,0.));
#46566=DIRECTION('ref_axis',(0.,-1.,1.83697019872103E-16));
#46567=DIRECTION('center_axis',(1.,0.,0.));
#46568=DIRECTION('ref_axis',(0.,1.,0.));
#46569=DIRECTION('center_axis',(0.,0.86771712654899,0.497058334900004));
#46570=DIRECTION('ref_axis',(0.,-0.497058334900004,0.86771712654899));
#46571=DIRECTION('',(-1.,0.,0.));
#46572=DIRECTION('',(0.,-0.497058334900004,0.86771712654899));
#46573=DIRECTION('',(1.,0.,0.));
#46574=DIRECTION('',(0.,-0.497058334900004,0.86771712654899));
#46575=DIRECTION('center_axis',(1.,0.,0.));
#46576=DIRECTION('ref_axis',(0.,-0.984807753012208,0.17364817766693));
#46577=DIRECTION('center_axis',(-1.,0.,0.));
#46578=DIRECTION('ref_axis',(0.,1.,0.));
#46579=DIRECTION('',(0.,-0.763858785394087,-0.645383417803921));
#46580=DIRECTION('center_axis',(0.,-0.645383417803921,0.763858785394087));
#46581=DIRECTION('ref_axis',(0.,-0.763858785394087,-0.645383417803921));
#46582=DIRECTION('',(1.,0.,0.));
#46583=DIRECTION('',(0.,-0.763858785394087,-0.645383417803921));
#46584=DIRECTION('center_axis',(1.,0.,0.));
#46585=DIRECTION('ref_axis',(0.,-0.984807753012208,0.17364817766693));
#46586=DIRECTION('center_axis',(1.,0.,0.));
#46587=DIRECTION('ref_axis',(0.,1.,0.));
#46588=DIRECTION('center_axis',(0.,0.940847827696465,0.338829404153244));
#46589=DIRECTION('ref_axis',(0.,-0.338829404153244,0.940847827696465));
#46590=DIRECTION('',(-1.,0.,0.));
#46591=DIRECTION('',(0.,-0.338829404153244,0.940847827696465));
#46592=DIRECTION('',(1.,0.,0.));
#46593=DIRECTION('',(0.,-0.338829404153244,0.940847827696465));
#46594=DIRECTION('center_axis',(1.,0.,0.));
#46595=DIRECTION('ref_axis',(0.,-0.939692620785908,0.342020143325669));
#46596=DIRECTION('center_axis',(-1.,0.,0.));
#46597=DIRECTION('ref_axis',(0.,1.,0.));
#46598=DIRECTION('',(0.,-0.864323708460692,-0.50293590744026));
#46599=DIRECTION('center_axis',(0.,-0.50293590744026,0.864323708460692));
#46600=DIRECTION('ref_axis',(0.,-0.864323708460692,-0.50293590744026));
#46601=DIRECTION('',(1.,0.,0.));
#46602=DIRECTION('',(0.,-0.864323708460692,-0.50293590744026));
#46603=DIRECTION('center_axis',(1.,0.,0.));
#46604=DIRECTION('ref_axis',(0.,-0.939692620785908,0.342020143325669));
#46605=DIRECTION('center_axis',(1.,0.,0.));
#46606=DIRECTION('ref_axis',(0.,1.,0.));
#46607=DIRECTION('center_axis',(0.,0.985391343691356,0.170305313417241));
#46608=DIRECTION('ref_axis',(0.,-0.170305313417241,0.985391343691356));
#46609=DIRECTION('',(-1.,0.,0.));
#46610=DIRECTION('',(0.,-0.170305313417241,0.985391343691356));
#46611=DIRECTION('',(1.,0.,0.));
#46612=DIRECTION('',(0.,-0.170305313417241,0.985391343691356));
#46613=DIRECTION('center_axis',(1.,0.,0.));
#46614=DIRECTION('ref_axis',(0.,-0.866025403784438,0.5));
#46615=DIRECTION('center_axis',(-1.,0.,0.));
#46616=DIRECTION('ref_axis',(0.,1.,0.));
#46617=DIRECTION('',(0.,-0.938526593014618,-0.345206944026876));
#46618=DIRECTION('center_axis',(0.,-0.345206944026876,0.938526593014618));
#46619=DIRECTION('ref_axis',(0.,-0.938526593014618,-0.345206944026876));
#46620=DIRECTION('',(1.,0.,0.));
#46621=DIRECTION('',(0.,-0.938526593014618,-0.345206944026876));
#46622=DIRECTION('center_axis',(1.,0.,0.));
#46623=DIRECTION('ref_axis',(0.,-0.866025403784438,0.5));
#46624=DIRECTION('center_axis',(1.,0.,0.));
#46625=DIRECTION('ref_axis',(0.,1.,0.));
#46626=DIRECTION('center_axis',(0.,0.999994242340264,-0.00339341808829868));
#46627=DIRECTION('ref_axis',(0.,0.00339341808829868,0.999994242340264));
#46628=DIRECTION('',(-1.,0.,0.));
#46629=DIRECTION('',(0.,0.00339341808829868,0.999994242340264));
#46630=DIRECTION('',(1.,0.,0.));
#46631=DIRECTION('',(0.,0.00339341808829868,0.999994242340264));
#46632=DIRECTION('center_axis',(1.,0.,0.));
#46633=DIRECTION('ref_axis',(0.,-0.766044443118978,0.642787609686539));
#46634=DIRECTION('center_axis',(-1.,0.,0.));
#46635=DIRECTION('ref_axis',(0.,1.,0.));
#46636=DIRECTION('',(0.,-0.984212821957166,-0.176989042302378));
#46637=DIRECTION('center_axis',(0.,-0.176989042302378,0.984212821957166));
#46638=DIRECTION('ref_axis',(0.,-0.984212821957166,-0.176989042302378));
#46639=DIRECTION('',(1.,0.,0.));
#46640=DIRECTION('',(0.,-0.984212821957166,-0.176989042302378));
#46641=DIRECTION('center_axis',(1.,0.,0.));
#46642=DIRECTION('ref_axis',(0.,-0.766044443118978,0.642787609686539));
#46643=DIRECTION('center_axis',(1.,0.,0.));
#46644=DIRECTION('ref_axis',(0.,1.,0.));
#46645=DIRECTION('center_axis',(0.,0.984212821957166,-0.176989042302378));
#46646=DIRECTION('ref_axis',(0.,0.176989042302378,0.984212821957166));
#46647=DIRECTION('',(-1.,0.,0.));
#46648=DIRECTION('',(0.,0.176989042302378,0.984212821957166));
#46649=DIRECTION('',(1.,0.,0.));
#46650=DIRECTION('',(0.,0.176989042302378,0.984212821957166));
#46651=DIRECTION('center_axis',(1.,0.,0.));
#46652=DIRECTION('ref_axis',(0.,-0.642787609686539,0.766044443118978));
#46653=DIRECTION('center_axis',(-1.,0.,0.));
#46654=DIRECTION('ref_axis',(0.,1.,0.));
#46655=DIRECTION('',(0.,-0.999994242340264,-0.00339341808829846));
#46656=DIRECTION('center_axis',(0.,-0.00339341808829846,0.999994242340264));
#46657=DIRECTION('ref_axis',(0.,-0.999994242340264,-0.00339341808829846));
#46658=DIRECTION('',(1.,0.,0.));
#46659=DIRECTION('',(0.,-0.999994242340264,-0.00339341808829846));
#46660=DIRECTION('center_axis',(1.,0.,0.));
#46661=DIRECTION('ref_axis',(0.,-0.642787609686539,0.766044443118978));
#46662=DIRECTION('center_axis',(1.,0.,0.));
#46663=DIRECTION('ref_axis',(0.,1.,0.));
#46664=DIRECTION('center_axis',(0.,0.938526593014617,-0.345206944026876));
#46665=DIRECTION('ref_axis',(0.,0.345206944026876,0.938526593014617));
#46666=DIRECTION('',(-1.,0.,0.));
#46667=DIRECTION('',(0.,0.345206944026876,0.938526593014617));
#46668=DIRECTION('',(1.,0.,0.));
#46669=DIRECTION('',(0.,0.345206944026876,0.938526593014617));
#46670=DIRECTION('center_axis',(1.,0.,0.));
#46671=DIRECTION('ref_axis',(0.,-0.5,0.866025403784439));
#46672=DIRECTION('center_axis',(-1.,0.,0.));
#46673=DIRECTION('ref_axis',(0.,1.,0.));
#46674=DIRECTION('',(0.,-0.985391343691356,0.170305313417242));
#46675=DIRECTION('center_axis',(0.,0.170305313417242,0.985391343691356));
#46676=DIRECTION('ref_axis',(0.,-0.985391343691356,0.170305313417242));
#46677=DIRECTION('',(1.,0.,0.));
#46678=DIRECTION('',(0.,-0.985391343691356,0.170305313417242));
#46679=DIRECTION('center_axis',(1.,0.,0.));
#46680=DIRECTION('ref_axis',(0.,-0.5,0.866025403784439));
#46681=DIRECTION('center_axis',(1.,0.,0.));
#46682=DIRECTION('ref_axis',(0.,1.,0.));
#46683=DIRECTION('center_axis',(0.,0.864323708460691,-0.50293590744026));
#46684=DIRECTION('ref_axis',(0.,0.50293590744026,0.864323708460691));
#46685=DIRECTION('',(-1.,0.,0.));
#46686=DIRECTION('',(0.,0.50293590744026,0.864323708460691));
#46687=DIRECTION('',(1.,0.,0.));
#46688=DIRECTION('',(0.,0.50293590744026,0.864323708460691));
#46689=DIRECTION('center_axis',(1.,0.,0.));
#46690=DIRECTION('ref_axis',(0.,-0.342020143325669,0.939692620785909));
#46691=DIRECTION('center_axis',(-1.,0.,0.));
#46692=DIRECTION('ref_axis',(0.,1.,0.));
#46693=DIRECTION('',(0.,-0.940847827696465,0.338829404153245));
#46694=DIRECTION('center_axis',(0.,0.338829404153245,0.940847827696465));
#46695=DIRECTION('ref_axis',(0.,-0.940847827696465,0.338829404153245));
#46696=DIRECTION('',(1.,0.,0.));
#46697=DIRECTION('',(0.,-0.940847827696465,0.338829404153245));
#46698=DIRECTION('center_axis',(1.,0.,0.));
#46699=DIRECTION('ref_axis',(0.,-0.342020143325669,0.939692620785909));
#46700=DIRECTION('center_axis',(1.,0.,0.));
#46701=DIRECTION('ref_axis',(0.,1.,0.));
#46702=DIRECTION('center_axis',(0.,0.763858785394087,-0.645383417803921));
#46703=DIRECTION('ref_axis',(0.,0.645383417803921,0.763858785394087));
#46704=DIRECTION('',(-1.,0.,0.));
#46705=DIRECTION('',(0.,0.645383417803921,0.763858785394087));
#46706=DIRECTION('',(1.,0.,0.));
#46707=DIRECTION('',(0.,0.645383417803921,0.763858785394087));
#46708=DIRECTION('center_axis',(1.,0.,0.));
#46709=DIRECTION('ref_axis',(0.,-0.17364817766693,0.984807753012208));
#46710=DIRECTION('center_axis',(-1.,0.,0.));
#46711=DIRECTION('ref_axis',(0.,1.,0.));
#46712=DIRECTION('',(0.,-0.86771712654899,0.497058334900004));
#46713=DIRECTION('center_axis',(0.,0.497058334900004,0.86771712654899));
#46714=DIRECTION('ref_axis',(0.,-0.86771712654899,0.497058334900004));
#46715=DIRECTION('',(1.,0.,0.));
#46716=DIRECTION('',(0.,-0.86771712654899,0.497058334900004));
#46717=DIRECTION('center_axis',(1.,0.,0.));
#46718=DIRECTION('ref_axis',(0.,-0.17364817766693,0.984807753012208));
#46719=DIRECTION('center_axis',(1.,0.,0.));
#46720=DIRECTION('ref_axis',(0.,1.,0.));
#46721=DIRECTION('center_axis',(0.,0.640184399664479,-0.768221279597376));
#46722=DIRECTION('ref_axis',(0.,0.768221279597376,0.640184399664479));
#46723=DIRECTION('',(-1.,0.,0.));
#46724=DIRECTION('',(0.,0.768221279597376,0.640184399664479));
#46725=DIRECTION('',(1.,0.,0.));
#46726=DIRECTION('',(0.,0.768221279597376,0.640184399664479));
#46727=DIRECTION('center_axis',(1.,0.,0.));
#46728=DIRECTION('ref_axis',(0.,1.22464679914735E-16,1.));
#46729=DIRECTION('center_axis',(-1.,0.,0.));
#46730=DIRECTION('ref_axis',(0.,1.,0.));
#46731=DIRECTION('',(0.,-0.768221279597376,0.64018439966448));
#46732=DIRECTION('center_axis',(-1.,0.,0.));
#46733=DIRECTION('ref_axis',(0.,1.,0.));
#46734=DIRECTION('center_axis',(0.,0.64018439966448,0.768221279597376));
#46735=DIRECTION('ref_axis',(0.,-0.768221279597376,0.64018439966448));
#46736=DIRECTION('',(1.,0.,0.));
#46737=DIRECTION('',(0.,-0.768221279597376,0.64018439966448));
#46738=DIRECTION('center_axis',(1.,0.,0.));
#46739=DIRECTION('ref_axis',(0.,1.22464679914735E-16,1.));
#46740=DIRECTION('center_axis',(1.,0.,0.));
#46741=DIRECTION('ref_axis',(0.,1.,0.));
#46742=DIRECTION('center_axis',(1.,0.,0.));
#46743=DIRECTION('ref_axis',(0.,1.,0.));
#46744=DIRECTION('center_axis',(0.,0.497058334900004,-0.86771712654899));
#46745=DIRECTION('ref_axis',(0.,0.86771712654899,0.497058334900003));
#46746=DIRECTION('',(-1.,0.,0.));
#46747=DIRECTION('',(0.,0.86771712654899,0.497058334900003));
#46748=DIRECTION('',(1.,0.,0.));
#46749=DIRECTION('',(0.,0.86771712654899,0.497058334900003));
#46750=DIRECTION('center_axis',(1.,0.,0.));
#46751=DIRECTION('ref_axis',(0.,0.173648177666931,0.984807753012208));
#46752=DIRECTION('center_axis',(-1.,0.,0.));
#46753=DIRECTION('ref_axis',(0.,1.,0.));
#46754=DIRECTION('',(0.,-0.64538341780392,0.763858785394087));
#46755=DIRECTION('center_axis',(0.,0.763858785394087,0.64538341780392));
#46756=DIRECTION('ref_axis',(0.,-0.64538341780392,0.763858785394087));
#46757=DIRECTION('',(1.,0.,0.));
#46758=DIRECTION('',(0.,-0.64538341780392,0.763858785394087));
#46759=DIRECTION('center_axis',(1.,0.,0.));
#46760=DIRECTION('ref_axis',(0.,0.173648177666931,0.984807753012208));
#46761=DIRECTION('center_axis',(1.,0.,0.));
#46762=DIRECTION('ref_axis',(0.,1.,0.));
#46763=DIRECTION('center_axis',(0.,0.338829404153245,-0.940847827696465));
#46764=DIRECTION('ref_axis',(0.,0.940847827696465,0.338829404153245));
#46765=DIRECTION('',(-1.,0.,0.));
#46766=DIRECTION('',(0.,0.940847827696465,0.338829404153245));
#46767=DIRECTION('',(1.,0.,0.));
#46768=DIRECTION('',(0.,0.940847827696465,0.338829404153245));
#46769=DIRECTION('center_axis',(1.,0.,0.));
#46770=DIRECTION('ref_axis',(0.,0.342020143325669,0.939692620785908));
#46771=DIRECTION('center_axis',(-1.,0.,0.));
#46772=DIRECTION('ref_axis',(0.,1.,0.));
#46773=DIRECTION('',(0.,-0.50293590744026,0.864323708460692));
#46774=DIRECTION('center_axis',(0.,0.864323708460692,0.50293590744026));
#46775=DIRECTION('ref_axis',(0.,-0.50293590744026,0.864323708460692));
#46776=DIRECTION('',(1.,0.,0.));
#46777=DIRECTION('',(0.,-0.50293590744026,0.864323708460692));
#46778=DIRECTION('center_axis',(1.,0.,0.));
#46779=DIRECTION('ref_axis',(0.,0.342020143325669,0.939692620785908));
#46780=DIRECTION('center_axis',(1.,0.,0.));
#46781=DIRECTION('ref_axis',(0.,1.,0.));
#46782=DIRECTION('center_axis',(0.,0.170305313417241,-0.985391343691356));
#46783=DIRECTION('ref_axis',(0.,0.985391343691356,0.170305313417241));
#46784=DIRECTION('',(-1.,0.,0.));
#46785=DIRECTION('',(0.,0.985391343691356,0.170305313417241));
#46786=DIRECTION('',(1.,0.,0.));
#46787=DIRECTION('',(0.,0.985391343691356,0.170305313417241));
#46788=DIRECTION('center_axis',(1.,0.,0.));
#46789=DIRECTION('ref_axis',(0.,0.5,0.866025403784439));
#46790=DIRECTION('center_axis',(-1.,0.,0.));
#46791=DIRECTION('ref_axis',(0.,1.,0.));
#46792=DIRECTION('',(0.,-0.345206944026876,0.938526593014617));
#46793=DIRECTION('center_axis',(0.,0.938526593014617,0.345206944026876));
#46794=DIRECTION('ref_axis',(0.,-0.345206944026876,0.938526593014617));
#46795=DIRECTION('',(1.,0.,0.));
#46796=DIRECTION('',(0.,-0.345206944026876,0.938526593014617));
#46797=DIRECTION('center_axis',(1.,0.,0.));
#46798=DIRECTION('ref_axis',(0.,0.5,0.866025403784439));
#46799=DIRECTION('center_axis',(1.,0.,0.));
#46800=DIRECTION('ref_axis',(0.,1.,0.));
#46801=DIRECTION('center_axis',(0.,-0.00339341808829868,-0.999994242340264));
#46802=DIRECTION('ref_axis',(0.,0.999994242340264,-0.00339341808829868));
#46803=DIRECTION('',(-1.,0.,0.));
#46804=DIRECTION('',(0.,0.999994242340264,-0.00339341808829868));
#46805=DIRECTION('',(1.,0.,0.));
#46806=DIRECTION('',(0.,0.999994242340264,-0.00339341808829868));
#46807=DIRECTION('center_axis',(1.,0.,0.));
#46808=DIRECTION('ref_axis',(0.,0.642787609686539,0.766044443118978));
#46809=DIRECTION('center_axis',(-1.,0.,0.));
#46810=DIRECTION('ref_axis',(0.,1.,0.));
#46811=DIRECTION('',(0.,-0.176989042302378,0.984212821957166));
#46812=DIRECTION('center_axis',(0.,0.984212821957166,0.176989042302378));
#46813=DIRECTION('ref_axis',(0.,-0.176989042302378,0.984212821957166));
#46814=DIRECTION('',(1.,0.,0.));
#46815=DIRECTION('',(0.,-0.176989042302378,0.984212821957166));
#46816=DIRECTION('center_axis',(1.,0.,0.));
#46817=DIRECTION('ref_axis',(0.,0.642787609686539,0.766044443118978));
#46818=DIRECTION('center_axis',(1.,0.,0.));
#46819=DIRECTION('ref_axis',(0.,1.,0.));
#46820=DIRECTION('center_axis',(0.,-0.176989042302378,-0.984212821957166));
#46821=DIRECTION('ref_axis',(0.,0.984212821957166,-0.176989042302378));
#46822=DIRECTION('',(-1.,0.,0.));
#46823=DIRECTION('',(0.,0.984212821957166,-0.176989042302378));
#46824=DIRECTION('',(1.,0.,0.));
#46825=DIRECTION('',(0.,0.984212821957166,-0.176989042302378));
#46826=DIRECTION('center_axis',(1.,0.,0.));
#46827=DIRECTION('ref_axis',(0.,0.766044443118978,0.642787609686539));
#46828=DIRECTION('center_axis',(-1.,0.,0.));
#46829=DIRECTION('ref_axis',(0.,1.,0.));
#46830=DIRECTION('',(0.,-0.00339341808829857,0.999994242340264));
#46831=DIRECTION('center_axis',(0.,0.999994242340264,0.00339341808829857));
#46832=DIRECTION('ref_axis',(0.,-0.00339341808829857,0.999994242340264));
#46833=DIRECTION('',(1.,0.,0.));
#46834=DIRECTION('',(0.,-0.00339341808829857,0.999994242340264));
#46835=DIRECTION('center_axis',(1.,0.,0.));
#46836=DIRECTION('ref_axis',(0.,0.766044443118978,0.642787609686539));
#46837=DIRECTION('center_axis',(1.,0.,0.));
#46838=DIRECTION('ref_axis',(0.,1.,0.));
#46839=DIRECTION('center_axis',(0.,-0.345206944026876,-0.938526593014617));
#46840=DIRECTION('ref_axis',(0.,0.938526593014617,-0.345206944026876));
#46841=DIRECTION('',(-1.,0.,0.));
#46842=DIRECTION('',(0.,0.938526593014617,-0.345206944026876));
#46843=DIRECTION('',(1.,0.,0.));
#46844=DIRECTION('',(0.,0.938526593014617,-0.345206944026876));
#46845=DIRECTION('center_axis',(1.,0.,0.));
#46846=DIRECTION('ref_axis',(0.,0.866025403784439,0.5));
#46847=DIRECTION('center_axis',(-1.,0.,0.));
#46848=DIRECTION('ref_axis',(0.,1.,0.));
#46849=DIRECTION('',(0.,0.170305313417242,0.985391343691356));
#46850=DIRECTION('center_axis',(0.,0.985391343691356,-0.170305313417242));
#46851=DIRECTION('ref_axis',(0.,0.170305313417242,0.985391343691356));
#46852=DIRECTION('',(1.,0.,0.));
#46853=DIRECTION('',(0.,0.170305313417242,0.985391343691356));
#46854=DIRECTION('center_axis',(1.,0.,0.));
#46855=DIRECTION('ref_axis',(0.,0.866025403784439,0.5));
#46856=DIRECTION('center_axis',(1.,0.,0.));
#46857=DIRECTION('ref_axis',(0.,1.,0.));
#46858=DIRECTION('center_axis',(0.,-0.50293590744026,-0.864323708460692));
#46859=DIRECTION('ref_axis',(0.,0.864323708460691,-0.50293590744026));
#46860=DIRECTION('',(-1.,0.,0.));
#46861=DIRECTION('',(0.,0.864323708460691,-0.50293590744026));
#46862=DIRECTION('',(1.,0.,0.));
#46863=DIRECTION('',(0.,0.864323708460691,-0.50293590744026));
#46864=DIRECTION('center_axis',(1.,0.,0.));
#46865=DIRECTION('ref_axis',(0.,0.939692620785908,0.342020143325669));
#46866=DIRECTION('center_axis',(-1.,0.,0.));
#46867=DIRECTION('ref_axis',(0.,1.,0.));
#46868=DIRECTION('',(0.,0.338829404153245,0.940847827696465));
#46869=DIRECTION('center_axis',(0.,0.940847827696465,-0.338829404153245));
#46870=DIRECTION('ref_axis',(0.,0.338829404153245,0.940847827696465));
#46871=DIRECTION('',(1.,0.,0.));
#46872=DIRECTION('',(0.,0.338829404153245,0.940847827696465));
#46873=DIRECTION('center_axis',(1.,0.,0.));
#46874=DIRECTION('ref_axis',(0.,0.939692620785908,0.342020143325669));
#46875=DIRECTION('center_axis',(1.,0.,0.));
#46876=DIRECTION('ref_axis',(0.,1.,0.));
#46877=DIRECTION('center_axis',(0.,-0.645383417803921,-0.763858785394087));
#46878=DIRECTION('ref_axis',(0.,0.763858785394087,-0.645383417803921));
#46879=DIRECTION('',(-1.,0.,0.));
#46880=DIRECTION('',(0.,0.763858785394087,-0.645383417803921));
#46881=DIRECTION('',(1.,0.,0.));
#46882=DIRECTION('',(0.,0.763858785394087,-0.645383417803921));
#46883=DIRECTION('center_axis',(1.,0.,0.));
#46884=DIRECTION('ref_axis',(0.,0.984807753012208,0.17364817766693));
#46885=DIRECTION('center_axis',(-1.,0.,0.));
#46886=DIRECTION('ref_axis',(0.,1.,0.));
#46887=DIRECTION('',(0.,0.497058334900004,0.86771712654899));
#46888=DIRECTION('center_axis',(0.,0.86771712654899,-0.497058334900004));
#46889=DIRECTION('ref_axis',(0.,0.497058334900004,0.86771712654899));
#46890=DIRECTION('',(1.,0.,0.));
#46891=DIRECTION('',(0.,0.497058334900004,0.86771712654899));
#46892=DIRECTION('center_axis',(1.,0.,0.));
#46893=DIRECTION('ref_axis',(0.,0.984807753012208,0.17364817766693));
#46894=DIRECTION('center_axis',(1.,0.,0.));
#46895=DIRECTION('ref_axis',(0.,1.,0.));
#46896=DIRECTION('center_axis',(0.,-0.768221279597376,-0.64018439966448));
#46897=DIRECTION('ref_axis',(0.,0.640184399664479,-0.768221279597376));
#46898=DIRECTION('',(-1.,0.,0.));
#46899=DIRECTION('',(0.,0.640184399664479,-0.768221279597376));
#46900=DIRECTION('',(1.,0.,0.));
#46901=DIRECTION('',(0.,0.640184399664479,-0.768221279597376));
#46902=DIRECTION('center_axis',(1.,0.,0.));
#46903=DIRECTION('ref_axis',(0.,1.,-6.12323399573677E-17));
#46904=DIRECTION('center_axis',(-1.,0.,0.));
#46905=DIRECTION('ref_axis',(0.,1.,0.));
#46906=DIRECTION('',(0.,0.640184399664479,0.768221279597376));
#46907=DIRECTION('center_axis',(0.,0.768221279597376,-0.64018439966448));
#46908=DIRECTION('ref_axis',(0.,0.640184399664479,0.768221279597376));
#46909=DIRECTION('',(1.,0.,0.));
#46910=DIRECTION('',(0.,0.640184399664479,0.768221279597376));
#46911=DIRECTION('center_axis',(1.,0.,0.));
#46912=DIRECTION('ref_axis',(0.,1.,-6.12323399573677E-17));
#46913=DIRECTION('center_axis',(1.,0.,0.));
#46914=DIRECTION('ref_axis',(0.,1.,0.));
#46915=DIRECTION('center_axis',(0.,-0.86771712654899,-0.497058334900004));
#46916=DIRECTION('ref_axis',(0.,0.497058334900004,-0.86771712654899));
#46917=DIRECTION('',(-1.,0.,0.));
#46918=DIRECTION('',(0.,0.497058334900004,-0.86771712654899));
#46919=DIRECTION('',(1.,0.,0.));
#46920=DIRECTION('',(0.,0.497058334900004,-0.86771712654899));
#46921=DIRECTION('center_axis',(1.,0.,0.));
#46922=DIRECTION('ref_axis',(0.,0.984807753012208,-0.17364817766693));
#46923=DIRECTION('center_axis',(-1.,0.,0.));
#46924=DIRECTION('ref_axis',(0.,1.,0.));
#46925=DIRECTION('',(0.,0.763858785394087,0.64538341780392));
#46926=DIRECTION('center_axis',(0.,0.645383417803921,-0.763858785394087));
#46927=DIRECTION('ref_axis',(0.,0.763858785394087,0.64538341780392));
#46928=DIRECTION('',(1.,0.,0.));
#46929=DIRECTION('',(0.,0.763858785394087,0.64538341780392));
#46930=DIRECTION('center_axis',(1.,0.,0.));
#46931=DIRECTION('ref_axis',(0.,0.984807753012208,-0.17364817766693));
#46932=DIRECTION('center_axis',(1.,0.,0.));
#46933=DIRECTION('ref_axis',(0.,1.,0.));
#46934=DIRECTION('center_axis',(0.,-0.940847827696465,-0.338829404153245));
#46935=DIRECTION('ref_axis',(0.,0.338829404153245,-0.940847827696465));
#46936=DIRECTION('',(-1.,0.,0.));
#46937=DIRECTION('',(0.,0.338829404153245,-0.940847827696465));
#46938=DIRECTION('',(1.,0.,0.));
#46939=DIRECTION('',(0.,0.338829404153245,-0.940847827696465));
#46940=DIRECTION('center_axis',(1.,0.,0.));
#46941=DIRECTION('ref_axis',(0.,0.939692620785908,-0.342020143325669));
#46942=DIRECTION('center_axis',(-1.,0.,0.));
#46943=DIRECTION('ref_axis',(0.,1.,0.));
#46944=DIRECTION('',(0.,0.864323708460692,0.50293590744026));
#46945=DIRECTION('center_axis',(0.,0.50293590744026,-0.864323708460692));
#46946=DIRECTION('ref_axis',(0.,0.864323708460692,0.50293590744026));
#46947=DIRECTION('',(1.,0.,0.));
#46948=DIRECTION('',(0.,0.864323708460692,0.50293590744026));
#46949=DIRECTION('center_axis',(1.,0.,0.));
#46950=DIRECTION('ref_axis',(0.,0.939692620785908,-0.342020143325669));
#46951=DIRECTION('center_axis',(1.,0.,0.));
#46952=DIRECTION('ref_axis',(0.,1.,0.));
#46953=DIRECTION('center_axis',(0.,-0.985391343691356,-0.170305313417241));
#46954=DIRECTION('ref_axis',(0.,0.170305313417241,-0.985391343691356));
#46955=DIRECTION('',(-1.,0.,0.));
#46956=DIRECTION('',(0.,0.170305313417241,-0.985391343691356));
#46957=DIRECTION('',(1.,0.,0.));
#46958=DIRECTION('',(0.,0.170305313417241,-0.985391343691356));
#46959=DIRECTION('center_axis',(1.,0.,0.));
#46960=DIRECTION('ref_axis',(0.,0.866025403784439,-0.5));
#46961=DIRECTION('center_axis',(-1.,0.,0.));
#46962=DIRECTION('ref_axis',(0.,1.,0.));
#46963=DIRECTION('',(0.,0.938526593014617,0.345206944026876));
#46964=DIRECTION('center_axis',(0.,0.345206944026876,-0.938526593014618));
#46965=DIRECTION('ref_axis',(0.,0.938526593014617,0.345206944026876));
#46966=DIRECTION('',(1.,0.,0.));
#46967=DIRECTION('',(0.,0.938526593014617,0.345206944026876));
#46968=DIRECTION('center_axis',(1.,0.,0.));
#46969=DIRECTION('ref_axis',(0.,0.866025403784439,-0.5));
#46970=DIRECTION('center_axis',(1.,0.,0.));
#46971=DIRECTION('ref_axis',(0.,1.,0.));
#46972=DIRECTION('center_axis',(0.,-0.999994242340264,0.00339341808829857));
#46973=DIRECTION('ref_axis',(0.,-0.00339341808829857,-0.999994242340264));
#46974=DIRECTION('',(-1.,0.,0.));
#46975=DIRECTION('',(0.,-0.00339341808829857,-0.999994242340264));
#46976=DIRECTION('',(1.,0.,0.));
#46977=DIRECTION('',(0.,-0.00339341808829857,-0.999994242340264));
#46978=DIRECTION('center_axis',(1.,0.,0.));
#46979=DIRECTION('ref_axis',(0.,0.766044443118978,-0.642787609686539));
#46980=DIRECTION('center_axis',(-1.,0.,0.));
#46981=DIRECTION('ref_axis',(0.,1.,0.));
#46982=DIRECTION('',(0.,0.984212821957166,0.176989042302378));
#46983=DIRECTION('center_axis',(0.,0.176989042302378,-0.984212821957166));
#46984=DIRECTION('ref_axis',(0.,0.984212821957166,0.176989042302378));
#46985=DIRECTION('',(1.,0.,0.));
#46986=DIRECTION('',(0.,0.984212821957166,0.176989042302378));
#46987=DIRECTION('center_axis',(1.,0.,0.));
#46988=DIRECTION('ref_axis',(0.,0.766044443118978,-0.642787609686539));
#46989=DIRECTION('center_axis',(1.,0.,0.));
#46990=DIRECTION('ref_axis',(0.,1.,0.));
#46991=DIRECTION('center_axis',(0.,-0.984212821957166,0.176989042302378));
#46992=DIRECTION('ref_axis',(0.,-0.176989042302378,-0.984212821957166));
#46993=DIRECTION('',(-1.,0.,0.));
#46994=DIRECTION('',(0.,-0.176989042302378,-0.984212821957166));
#46995=DIRECTION('',(1.,0.,0.));
#46996=DIRECTION('',(0.,-0.176989042302378,-0.984212821957166));
#46997=DIRECTION('center_axis',(1.,0.,0.));
#46998=DIRECTION('ref_axis',(0.,0.642787609686539,-0.766044443118978));
#46999=DIRECTION('center_axis',(-1.,0.,0.));
#47000=DIRECTION('ref_axis',(0.,1.,0.));
#47001=DIRECTION('',(0.,0.999994242340264,0.00339341808829846));
#47002=DIRECTION('center_axis',(0.,0.00339341808829846,-0.999994242340264));
#47003=DIRECTION('ref_axis',(0.,0.999994242340264,0.00339341808829846));
#47004=DIRECTION('',(1.,0.,0.));
#47005=DIRECTION('',(0.,0.999994242340264,0.00339341808829846));
#47006=DIRECTION('center_axis',(1.,0.,0.));
#47007=DIRECTION('ref_axis',(0.,0.642787609686539,-0.766044443118978));
#47008=DIRECTION('center_axis',(1.,0.,0.));
#47009=DIRECTION('ref_axis',(0.,1.,0.));
#47010=DIRECTION('center_axis',(0.,-0.938526593014617,0.345206944026876));
#47011=DIRECTION('ref_axis',(0.,-0.345206944026876,-0.938526593014617));
#47012=DIRECTION('',(-1.,0.,0.));
#47013=DIRECTION('',(0.,-0.345206944026876,-0.938526593014617));
#47014=DIRECTION('',(1.,0.,0.));
#47015=DIRECTION('',(0.,-0.345206944026876,-0.938526593014617));
#47016=DIRECTION('center_axis',(1.,0.,0.));
#47017=DIRECTION('ref_axis',(0.,0.5,-0.866025403784439));
#47018=DIRECTION('center_axis',(-1.,0.,0.));
#47019=DIRECTION('ref_axis',(0.,1.,0.));
#47020=DIRECTION('',(0.,0.985391343691356,-0.170305313417241));
#47021=DIRECTION('center_axis',(0.,-0.170305313417241,-0.985391343691356));
#47022=DIRECTION('ref_axis',(0.,0.985391343691356,-0.170305313417241));
#47023=DIRECTION('',(1.,0.,0.));
#47024=DIRECTION('',(0.,0.985391343691356,-0.170305313417241));
#47025=DIRECTION('center_axis',(1.,0.,0.));
#47026=DIRECTION('ref_axis',(0.,0.5,-0.866025403784439));
#47027=DIRECTION('center_axis',(1.,0.,0.));
#47028=DIRECTION('ref_axis',(0.,1.,0.));
#47029=DIRECTION('center_axis',(0.,-0.864323708460692,0.50293590744026));
#47030=DIRECTION('ref_axis',(0.,-0.50293590744026,-0.864323708460691));
#47031=DIRECTION('',(-1.,0.,0.));
#47032=DIRECTION('',(0.,-0.50293590744026,-0.864323708460691));
#47033=DIRECTION('',(1.,0.,0.));
#47034=DIRECTION('',(0.,-0.50293590744026,-0.864323708460691));
#47035=DIRECTION('center_axis',(1.,0.,0.));
#47036=DIRECTION('ref_axis',(0.,0.342020143325669,-0.939692620785908));
#47037=DIRECTION('center_axis',(-1.,0.,0.));
#47038=DIRECTION('ref_axis',(0.,1.,0.));
#47039=DIRECTION('',(0.,0.940847827696465,-0.338829404153245));
#47040=DIRECTION('center_axis',(0.,-0.338829404153245,-0.940847827696465));
#47041=DIRECTION('ref_axis',(0.,0.940847827696465,-0.338829404153245));
#47042=DIRECTION('',(1.,0.,0.));
#47043=DIRECTION('',(0.,0.940847827696465,-0.338829404153245));
#47044=DIRECTION('center_axis',(1.,0.,0.));
#47045=DIRECTION('ref_axis',(0.,0.342020143325669,-0.939692620785908));
#47046=DIRECTION('center_axis',(1.,0.,0.));
#47047=DIRECTION('ref_axis',(0.,1.,0.));
#47048=DIRECTION('center_axis',(0.,-0.763858785394087,0.645383417803921));
#47049=DIRECTION('ref_axis',(0.,-0.645383417803921,-0.763858785394087));
#47050=DIRECTION('',(-1.,0.,0.));
#47051=DIRECTION('',(0.,-0.645383417803921,-0.763858785394087));
#47052=DIRECTION('',(1.,0.,0.));
#47053=DIRECTION('',(0.,-0.645383417803921,-0.763858785394087));
#47054=DIRECTION('center_axis',(1.,0.,0.));
#47055=DIRECTION('ref_axis',(0.,0.17364817766693,-0.984807753012208));
#47056=DIRECTION('center_axis',(-1.,0.,0.));
#47057=DIRECTION('ref_axis',(0.,1.,0.));
#47058=DIRECTION('',(0.,0.86771712654899,-0.497058334900004));
#47059=DIRECTION('center_axis',(0.,-0.497058334900004,-0.86771712654899));
#47060=DIRECTION('ref_axis',(0.,0.86771712654899,-0.497058334900004));
#47061=DIRECTION('',(1.,0.,0.));
#47062=DIRECTION('',(0.,0.86771712654899,-0.497058334900004));
#47063=DIRECTION('center_axis',(1.,0.,0.));
#47064=DIRECTION('ref_axis',(0.,0.17364817766693,-0.984807753012208));
#47065=DIRECTION('center_axis',(1.,0.,0.));
#47066=DIRECTION('ref_axis',(0.,1.,0.));
#47067=DIRECTION('center_axis',(0.,-0.64018439966448,0.768221279597376));
#47068=DIRECTION('ref_axis',(0.,-0.768221279597376,-0.640184399664479));
#47069=DIRECTION('',(-1.,0.,0.));
#47070=DIRECTION('',(0.,-0.768221279597376,-0.640184399664479));
#47071=DIRECTION('',(1.,0.,0.));
#47072=DIRECTION('',(0.,-0.768221279597376,-0.640184399664479));
#47073=DIRECTION('center_axis',(1.,0.,0.));
#47074=DIRECTION('ref_axis',(0.,0.,-1.));
#47075=DIRECTION('center_axis',(-1.,0.,0.));
#47076=DIRECTION('ref_axis',(0.,1.,0.));
#47077=DIRECTION('',(0.,0.768221279597376,-0.640184399664479));
#47078=DIRECTION('center_axis',(0.,-0.64018439966448,-0.768221279597376));
#47079=DIRECTION('ref_axis',(0.,0.768221279597376,-0.640184399664479));
#47080=DIRECTION('',(1.,0.,0.));
#47081=DIRECTION('',(0.,0.768221279597376,-0.640184399664479));
#47082=DIRECTION('center_axis',(1.,0.,0.));
#47083=DIRECTION('ref_axis',(0.,0.,-1.));
#47084=DIRECTION('center_axis',(1.,0.,0.));
#47085=DIRECTION('ref_axis',(0.,1.,0.));
#47086=DIRECTION('center_axis',(1.,0.,0.));
#47087=DIRECTION('ref_axis',(0.,1.,0.));
#47088=DIRECTION('center_axis',(1.,0.,0.));
#47089=DIRECTION('ref_axis',(0.,0.,-1.));
#47090=DIRECTION('',(-1.,0.,0.));
#47091=DIRECTION('',(-1.,0.,0.));
#47092=DIRECTION('center_axis',(-1.,0.,0.));
#47093=DIRECTION('ref_axis',(0.,1.,0.));
#47094=DIRECTION('',(-0.698323852075328,-0.71578194837721,-8.76580071967607E-17));
#47095=DIRECTION('axis',(0.,0.,1.));
#47096=DIRECTION('refdir',(1.,0.,0.));
#47097=DIRECTION('center_axis',(-1.,0.,-2.15639575486977E-15));
#47098=DIRECTION('ref_axis',(0.,1.,3.2200311221276E-17));
#47099=DIRECTION('center_axis',(-1.,0.,0.));
#47100=DIRECTION('ref_axis',(0.,1.,0.));
#47101=DIRECTION('',(-0.277278884798545,-0.960789477484467,-7.46523506113315E-16));
#47102=DIRECTION('center_axis',(1.,0.,0.));
#47103=DIRECTION('ref_axis',(0.,1.,6.12323399573676E-17));
#47104=DIRECTION('center_axis',(1.,0.,0.));
#47105=DIRECTION('ref_axis',(0.,1.,6.12323399573676E-17));
#47106=DIRECTION('center_axis',(1.,0.,0.));
#47107=DIRECTION('ref_axis',(0.,1.,6.12323399573676E-17));
#47108=DIRECTION('center_axis',(1.,0.,0.));
#47109=DIRECTION('ref_axis',(0.,1.,6.12323399573676E-17));
#47110=DIRECTION('center_axis',(1.,0.,0.));
#47111=DIRECTION('ref_axis',(0.,1.,6.12323399573676E-17));
#47112=DIRECTION('center_axis',(1.,0.,0.));
#47113=DIRECTION('ref_axis',(0.,1.,6.12323399573676E-17));
#47114=DIRECTION('center_axis',(-1.,0.,0.));
#47115=DIRECTION('ref_axis',(0.,1.,0.));
#47116=DIRECTION('center_axis',(-1.,0.,0.));
#47117=DIRECTION('ref_axis',(0.,1.,0.));
#47118=DIRECTION('center_axis',(-1.,0.,0.));
#47119=DIRECTION('ref_axis',(0.,1.,0.));
#47120=DIRECTION('center_axis',(-1.,0.,0.));
#47121=DIRECTION('ref_axis',(0.,1.,0.));
#47122=DIRECTION('center_axis',(-1.,0.,0.));
#47123=DIRECTION('ref_axis',(0.,1.,0.));
#47124=DIRECTION('center_axis',(-1.,0.,0.));
#47125=DIRECTION('ref_axis',(0.,1.,0.));
#47126=DIRECTION('center_axis',(1.,0.,0.));
#47127=DIRECTION('ref_axis',(0.,0.,-1.));
#47128=DIRECTION('center_axis',(-1.,0.,0.));
#47129=DIRECTION('ref_axis',(0.,1.,0.));
#47130=DIRECTION('center_axis',(-0.547750005235851,-0.724553275351849,0.418321028566617));
#47131=DIRECTION('ref_axis',(0.606949534647158,0.,0.79474037420506));
#47132=DIRECTION('',(0.,-0.5,-0.866025403784439));
#47133=DIRECTION('',(0.677497944020808,-0.0907675134870585,0.729902592366238));
#47134=DIRECTION('',(-0.677497944020809,0.67749794402081,0.286344323664976));
#47135=DIRECTION('center_axis',(-0.547750005235851,0.,0.836642057133231));
#47136=DIRECTION('ref_axis',(0.836642057133231,0.,0.547750005235851));
#47137=DIRECTION('',(0.,-1.,0.));
#47138=DIRECTION('',(0.67749794402081,0.586730430533746,0.443558268701261));
#47139=DIRECTION('',(-0.677497944020808,0.58673043053375,-0.443558268701259));
#47140=DIRECTION('center_axis',(-0.547750005235851,-0.72455327535185,-0.418321028566616));
#47141=DIRECTION('ref_axis',(-0.606949534647158,0.,0.79474037420506));
#47142=DIRECTION('',(0.,0.499999999999999,-0.866025403784439));
#47143=DIRECTION('',(0.677497944020809,-0.677497944020809,0.286344323664978));
#47144=DIRECTION('',(-0.67749794402081,0.0907675134870618,0.729902592366236));
#47145=DIRECTION('center_axis',(-0.707106781186548,-0.707106781186547,0.));
#47146=DIRECTION('ref_axis',(0.,0.,1.));
#47147=DIRECTION('',(0.,0.,1.));
#47148=DIRECTION('',(0.,0.,-1.));
#47149=DIRECTION('center_axis',(0.353397121838513,-0.810143725338629,0.467736697908881));
#47150=DIRECTION('ref_axis',(0.797870555551687,0.,-0.602828812005234));
#47151=DIRECTION('',(2.56395024851141E-15,0.5,0.866025403784439));
#47152=DIRECTION('center_axis',(-0.547750005235851,0.72455327535185,0.418321028566616));
#47153=DIRECTION('ref_axis',(0.606949534647158,0.,0.79474037420506));
#47154=DIRECTION('',(0.,-0.500000000000001,0.866025403784438));
#47155=DIRECTION('',(0.677497944020809,0.677497944020809,-0.286344323664978));
#47156=DIRECTION('',(-0.677497944020809,-0.0907675134870602,-0.729902592366237));
#47157=DIRECTION('center_axis',(0.353397121838516,2.02674207780683E-12,
0.935473395814255));
#47158=DIRECTION('ref_axis',(0.935473395814254,0.,-0.353397121838516));
#47159=DIRECTION('',(0.,1.,0.));
#47160=DIRECTION('center_axis',(-0.547750005235851,0.,-0.836642057133231));
#47161=DIRECTION('ref_axis',(-0.836642057133231,0.,0.547750005235851));
#47162=DIRECTION('',(0.,1.,0.));
#47163=DIRECTION('',(0.677497944020809,-0.586730430533748,-0.44355826870126));
#47164=DIRECTION('',(-0.67749794402081,-0.586730430533747,0.44355826870126));
#47165=DIRECTION('center_axis',(-0.707106781186548,-0.353553390593274,-0.612372435695794));
#47166=DIRECTION('ref_axis',(-0.654653670707977,0.,0.755928946018455));
#47167=DIRECTION('',(0.,-0.866025403784439,0.5));
#47168=DIRECTION('',(0.,0.866025403784439,-0.5));
#47169=DIRECTION('center_axis',(0.353397121838512,-0.810143725340653,-0.467736697905376));
#47170=DIRECTION('ref_axis',(-0.797870555549515,0.,-0.602828812008109));
#47171=DIRECTION('',(7.69185074553426E-15,-0.499999999999999,0.866025403784439));
#47172=DIRECTION('center_axis',(-0.547750005235851,0.72455327535185,-0.418321028566616));
#47173=DIRECTION('ref_axis',(-0.606949534647157,0.,0.79474037420506));
#47174=DIRECTION('',(0.677497944020809,0.0907675134870632,-0.729902592366237));
#47175=DIRECTION('',(-0.677497944020809,-0.677497944020809,-0.286344323664978));
#47176=DIRECTION('',(0.,0.5,0.866025403784439));
#47177=DIRECTION('center_axis',(-0.707106781186548,0.707106781186547,-2.14132276458349E-16));
#47178=DIRECTION('ref_axis',(-3.02828769509222E-16,0.,1.));
#47179=DIRECTION('',(0.,-3.02828769509223E-16,-1.));
#47180=DIRECTION('',(0.,3.02828769509223E-16,1.));
#47181=DIRECTION('center_axis',(0.353397121838516,0.810143725340652,0.467736697905373));
#47182=DIRECTION('ref_axis',(0.79787055554951,0.,-0.602828812008115));
#47183=DIRECTION('',(0.,0.500000000000001,-0.866025403784438));
#47184=DIRECTION('center_axis',(0.353397121838512,-2.0243364797534E-12,
-0.935473395814256));
#47185=DIRECTION('ref_axis',(-0.935473395814256,0.,-0.353397121838512));
#47186=DIRECTION('',(-2.56395024851142E-15,-1.,0.));
#47187=DIRECTION('center_axis',(0.353397121838513,0.810143725338629,-0.46773669790888));
#47188=DIRECTION('ref_axis',(-0.797870555551687,0.,-0.602828812005235));
#47189=DIRECTION('',(0.,-0.5,-0.866025403784439));
#47190=DIRECTION('center_axis',(0.,0.866025403784439,-0.5));
#47191=DIRECTION('ref_axis',(-1.,0.,0.));
#47192=DIRECTION('',(-1.,0.,0.));
#47193=DIRECTION('',(1.,0.,0.));
#47194=DIRECTION('center_axis',(0.,0.,-1.));
#47195=DIRECTION('ref_axis',(-1.,0.,0.));
#47196=DIRECTION('',(-1.,0.,0.));
#47197=DIRECTION('',(1.,0.,0.));
#47198=DIRECTION('center_axis',(0.,0.866025403784438,0.500000000000001));
#47199=DIRECTION('ref_axis',(1.,0.,0.));
#47200=DIRECTION('',(-1.,0.,0.));
#47201=DIRECTION('',(1.,0.,0.));
#47202=DIRECTION('center_axis',(-0.707106781186547,0.353553390593274,-0.612372435695795));
#47203=DIRECTION('ref_axis',(-0.654653670707977,0.,0.755928946018454));
#47204=DIRECTION('',(0.,-0.866025403784439,-0.5));
#47205=DIRECTION('',(0.,0.866025403784439,0.5));
#47206=DIRECTION('center_axis',(0.,-0.866025403784439,-0.499999999999999));
#47207=DIRECTION('ref_axis',(0.,0.499999999999999,-0.866025403784439));
#47208=DIRECTION('',(-1.,0.,0.));
#47209=DIRECTION('',(1.,0.,0.));
#47210=DIRECTION('center_axis',(0.,0.,1.));
#47211=DIRECTION('ref_axis',(1.,0.,0.));
#47212=DIRECTION('',(-1.,0.,0.));
#47213=DIRECTION('',(1.,0.,0.));
#47214=DIRECTION('center_axis',(-0.707106781186548,0.353553390593274,0.612372435695794));
#47215=DIRECTION('ref_axis',(0.654653670707977,0.,0.755928946018455));
#47216=DIRECTION('',(0.,0.866025403784439,-0.5));
#47217=DIRECTION('',(0.,-0.866025403784439,0.5));
#47218=DIRECTION('center_axis',(0.,-0.866025403784439,0.5));
#47219=DIRECTION('ref_axis',(1.,0.,0.));
#47220=DIRECTION('',(-1.,0.,0.));
#47221=DIRECTION('',(1.,0.,0.));
#47222=DIRECTION('center_axis',(-0.707106781186548,-0.353553390593273,0.612372435695794));
#47223=DIRECTION('ref_axis',(0.654653670707976,0.,0.755928946018455));
#47224=DIRECTION('',(0.,0.866025403784439,0.5));
#47225=DIRECTION('',(0.,-0.866025403784439,-0.5));
#47226=DIRECTION('center_axis',(0.,1.,-3.02828769509223E-16));
#47227=DIRECTION('ref_axis',(0.,3.02828769509223E-16,1.));
#47228=DIRECTION('center_axis',(1.,0.,0.));
#47229=DIRECTION('ref_axis',(0.,0.,-1.));
#47230=DIRECTION('center_axis',(1.,0.,0.));
#47231=DIRECTION('ref_axis',(0.,1.,0.));
#47232=DIRECTION('center_axis',(0.,0.5,-0.866025403784439));
#47233=DIRECTION('ref_axis',(0.,0.866025403784439,0.5));
#47234=DIRECTION('center_axis',(0.,-0.5,-0.866025403784439));
#47235=DIRECTION('ref_axis',(0.,0.866025403784439,-0.5));
#47236=DIRECTION('center_axis',(0.,0.5,0.866025403784439));
#47237=DIRECTION('ref_axis',(0.,-0.866025403784439,0.5));
#47238=DIRECTION('center_axis',(0.,-1.,0.));
#47239=DIRECTION('ref_axis',(0.,0.,-1.));
#47240=DIRECTION('center_axis',(0.,-0.5,0.866025403784439));
#47241=DIRECTION('ref_axis',(0.,-0.866025403784439,-0.5));
#47242=DIRECTION('center_axis',(1.,0.,0.));
#47243=DIRECTION('ref_axis',(0.,1.,0.));
#47244=DIRECTION('center_axis',(1.,0.,0.));
#47245=DIRECTION('ref_axis',(0.,0.,-1.));
#47246=DIRECTION('',(0.707106781186547,-0.707106781186548,-8.65956056235494E-17));
#47247=DIRECTION('center_axis',(1.,0.,0.));
#47248=DIRECTION('ref_axis',(0.,0.,-1.));
#47249=DIRECTION('center_axis',(1.,0.,0.));
#47250=DIRECTION('ref_axis',(0.,1.,0.));
#47251=DIRECTION('',(-0.866906303057535,0.498471124258083,6.10451066790044E-17));
#47252=DIRECTION('center_axis',(1.,0.,0.));
#47253=DIRECTION('ref_axis',(0.,0.,-1.));
#47254=DIRECTION('center_axis',(-1.,0.,0.));
#47255=DIRECTION('ref_axis',(0.,0.,1.));
#47256=DIRECTION('center_axis',(1.,0.,0.));
#47257=DIRECTION('ref_axis',(0.,0.,-1.));
#47258=DIRECTION('center_axis',(1.,0.,0.));
#47259=DIRECTION('ref_axis',(0.,0.,-1.));
#47260=DIRECTION('',(-1.,0.,0.));
#47261=DIRECTION('',(0.,0.,1.));
#47262=DIRECTION('',(1.,0.,0.));
#47263=DIRECTION('',(0.,0.,1.));
#47264=DIRECTION('',(1.,0.,0.));
#47265=DIRECTION('',(0.,0.,1.));
#47266=DIRECTION('',(1.,0.,0.));
#47267=DIRECTION('',(0.,0.,-1.));
#47268=DIRECTION('',(-1.,0.,0.));
#47269=DIRECTION('',(0.,0.,-1.));
#47270=DIRECTION('',(-1.,0.,0.));
#47271=DIRECTION('',(0.,0.,1.));
#47272=DIRECTION('',(1.,0.,0.));
#47273=DIRECTION('',(0.,0.,1.));
#47274=DIRECTION('',(1.,0.,0.));
#47275=DIRECTION('',(0.,0.,1.));
#47276=DIRECTION('',(1.,0.,0.));
#47277=DIRECTION('',(0.,0.,1.));
#47278=DIRECTION('',(1.,0.,0.));
#47279=DIRECTION('',(0.,0.,1.));
#47280=DIRECTION('',(1.,0.,0.));
#47281=DIRECTION('',(0.,0.,1.));
#47282=DIRECTION('',(1.,0.,0.));
#47283=DIRECTION('',(0.,1.,0.));
#47284=DIRECTION('',(1.,0.,0.));
#47285=DIRECTION('',(0.,0.,1.));
#47286=DIRECTION('',(1.,0.,0.));
#47287=DIRECTION('',(0.,0.309016994374948,0.951056516295154));
#47288=DIRECTION('',(0.999999999999999,0.,0.));
#47289=DIRECTION('',(0.,0.,1.));
#47290=DIRECTION('',(1.,0.,0.));
#47291=DIRECTION('',(0.,-0.809016994374947,0.587785252292473));
#47292=DIRECTION('',(1.,0.,0.));
#47293=DIRECTION('',(0.,0.,1.));
#47294=DIRECTION('',(1.,0.,0.));
#47295=DIRECTION('',(0.,-0.809016994374949,-0.587785252292473));
#47296=DIRECTION('',(0.999999999999999,0.,0.));
#47297=DIRECTION('',(0.,0.,1.));
#47298=DIRECTION('',(1.,0.,0.));
#47299=DIRECTION('',(0.,0.309016994374948,-0.951056516295154));
#47300=DIRECTION('',(1.,0.,0.));
#47301=DIRECTION('',(0.,0.,1.));
#47302=DIRECTION('',(1.,0.,0.));
#47303=CARTESIAN_POINT('',(0.,0.,0.));
#47304=CARTESIAN_POINT('',(0.,0.,0.));
#47305=CARTESIAN_POINT('Origin',(6.63819660112501,0.,-1.21095483169075E-15));
#47306=CARTESIAN_POINT('',(7.,40.,-4.89858719658941E-15));
#47307=CARTESIAN_POINT('',(7.,-40.,-4.89858719658941E-15));
#47308=CARTESIAN_POINT('Origin',(7.,0.,0.));
#47309=CARTESIAN_POINT('Origin',(7.,0.,0.));
#47310=CARTESIAN_POINT('',(6.27639320225002,39.5527864045,4.84381932676299E-15));
#47311=CARTESIAN_POINT('',(6.63819660112501,39.77639320225,4.8712032616762E-15));
#47312=CARTESIAN_POINT('',(6.27639320225002,-39.5527864045,-4.84381932676299E-15));
#47313=CARTESIAN_POINT('Origin',(6.27639320225002,0.,-2.4219096633815E-15));
#47314=CARTESIAN_POINT('Origin',(6.27639320225002,0.,-2.4219096633815E-15));
#47315=CARTESIAN_POINT('Origin',(5.75,0.,0.));
#47316=CARTESIAN_POINT('',(5.22360679774998,-37.4472135955,-4.58596102667163E-15));
#47317=CARTESIAN_POINT('',(5.75,-38.5,-4.71489017671731E-15));
#47318=CARTESIAN_POINT('',(5.22360679774998,37.4472135955,-4.58596102667163E-15));
#47319=CARTESIAN_POINT('Origin',(5.22360679774998,0.,-2.29298051333581E-15));
#47320=CARTESIAN_POINT('Origin',(5.22360679774998,0.,-2.29298051333581E-15));
#47321=CARTESIAN_POINT('Origin',(31.25,0.,0.));
#47322=CARTESIAN_POINT('',(56.,-40.,-4.89858719658941E-15));
#47323=CARTESIAN_POINT('Origin',(56.,0.,0.));
#47324=CARTESIAN_POINT('',(31.25,-40.,-4.89858719658941E-15));
#47325=CARTESIAN_POINT('Origin',(5.11180339887499,0.,-1.14649025666791E-15));
#47326=CARTESIAN_POINT('',(5.,36.5,4.46996081688784E-15));
#47327=CARTESIAN_POINT('',(5.11180339887499,36.97360679775,4.52796092177973E-15));
#47328=CARTESIAN_POINT('Origin',(5.,0.,0.));
#47329=CARTESIAN_POINT('Origin',(5.,37.,0.));
#47330=CARTESIAN_POINT('',(5.,-33.2,-4.06582737316921E-15));
#47331=CARTESIAN_POINT('Origin',(5.,0.,0.));
#47332=CARTESIAN_POINT('Origin',(32.19,0.,0.));
#47333=CARTESIAN_POINT('',(31.94,26.5,-3.24531401774049E-15));
#47334=CARTESIAN_POINT('Origin',(31.94,0.,0.));
#47335=CARTESIAN_POINT('',(32.44,26.,3.18408167778312E-15));
#47336=CARTESIAN_POINT('',(32.19,26.25,-3.2146978477618E-15));
#47337=CARTESIAN_POINT('',(32.44,-26.,-3.18408167778312E-15));
#47338=CARTESIAN_POINT('Origin',(32.44,0.,0.));
#47339=CARTESIAN_POINT('Origin',(32.44,0.,0.));
#47340=CARTESIAN_POINT('Origin',(32.97,0.,0.));
#47341=CARTESIAN_POINT('',(34.,-26.,-3.18408167778312E-15));
#47342=CARTESIAN_POINT('Origin',(34.,0.,0.));
#47343=CARTESIAN_POINT('',(32.97,-26.,-3.18408167778312E-15));
#47344=CARTESIAN_POINT('Origin',(31.94,29.58,0.));
#47345=CARTESIAN_POINT('',(31.94,-29.58,-3.62250523187787E-15));
#47346=CARTESIAN_POINT('Origin',(31.94,0.,0.));
#47347=CARTESIAN_POINT('Origin',(104.823223304703,0.,-9.90541890020826E-16));
#47348=CARTESIAN_POINT('',(105.,31.5,-3.85763741731416E-15));
#47349=CARTESIAN_POINT('Origin',(105.,0.,0.));
#47350=CARTESIAN_POINT('',(104.646446609407,32.3535533905933,3.96216756008331E-15));
#47351=CARTESIAN_POINT('',(104.823223304703,31.9267766952966,3.90990248869873E-15));
#47352=CARTESIAN_POINT('',(104.646446609407,-32.3535533905933,-3.96216756008331E-15));
#47353=CARTESIAN_POINT('Origin',(104.646446609407,0.,-1.98108378004165E-15));
#47354=CARTESIAN_POINT('Origin',(104.646446609407,0.,-1.98108378004165E-15));
#47355=CARTESIAN_POINT('Origin',(104.,0.,0.));
#47356=CARTESIAN_POINT('',(103.353553390593,-33.6464466094067,-4.12050131428923E-15));
#47357=CARTESIAN_POINT('',(104.,-33.,-4.04133443718627E-15));
#47358=CARTESIAN_POINT('',(103.353553390593,33.6464466094067,-4.12050131428923E-15));
#47359=CARTESIAN_POINT('Origin',(103.353553390593,0.,-2.06025065714461E-15));
#47360=CARTESIAN_POINT('Origin',(103.353553390593,0.,-2.06025065714461E-15));
#47361=CARTESIAN_POINT('Origin',(105.,25.16,0.));
#47362=CARTESIAN_POINT('',(105.,-25.16,-3.08121134665474E-15));
#47363=CARTESIAN_POINT('Origin',(105.,0.,0.));
#47364=CARTESIAN_POINT('Origin',(102.928240579529,0.,-2.07272928697064E-15));
#47365=CARTESIAN_POINT('',(102.502927768465,34.0540295903842,4.17041583359333E-15));
#47366=CARTESIAN_POINT('',(102.928240579529,33.8502380998955,4.14545857394128E-15));
#47367=CARTESIAN_POINT('',(102.502927768465,-34.0540295903842,-4.17041583359333E-15));
#47368=CARTESIAN_POINT('Origin',(102.502927768465,0.,-2.08520791679666E-15));
#47369=CARTESIAN_POINT('Origin',(102.502927768465,0.,-2.08520791679666E-15));
#47370=CARTESIAN_POINT('Origin',(91.5,0.,0.));
#47371=CARTESIAN_POINT('',(80.,-36.5,-4.46996081688784E-15));
#47372=CARTESIAN_POINT('',(91.5,-35.25,-4.31687996699442E-15));
#47373=CARTESIAN_POINT('Origin',(80.,0.,0.));
#47374=CARTESIAN_POINT('Origin',(70.90242469777,0.,-7.77414446918783E-15));
#47375=CARTESIAN_POINT('',(71.0821994936527,126.506803038084,-1.54926151410954E-14));
#47376=CARTESIAN_POINT('',(71.0821994936527,-126.506803038084,-1.54926151410954E-14));
#47377=CARTESIAN_POINT('Origin',(71.0821994936527,0.,-7.74630757054771E-15));
#47378=CARTESIAN_POINT('Origin',(71.0821994936527,0.,-7.74630757054771E-15));
#47379=CARTESIAN_POINT('',(70.7226499018874,127.416025147169,1.56039627356559E-14));
#47380=CARTESIAN_POINT('',(70.90242469777,126.961414092626,1.55482889383757E-14));
#47381=CARTESIAN_POINT('',(70.7226499018874,-127.416025147169,-1.56039627356559E-14));
#47382=CARTESIAN_POINT('Origin',(70.7226499018874,0.,-7.80198136782795E-15));
#47383=CARTESIAN_POINT('Origin',(70.7226499018874,0.,-7.80198136782795E-15));
#47384=CARTESIAN_POINT('Origin',(69.5,0.,0.));
#47385=CARTESIAN_POINT('',(68.2773500981126,-131.083974852831,-1.60531570223032E-14));
#47386=CARTESIAN_POINT('',(69.5,-129.25,-1.58285598789795E-14));
#47387=CARTESIAN_POINT('',(68.2773500981126,131.083974852831,-1.60531570223032E-14));
#47388=CARTESIAN_POINT('Origin',(68.2773500981126,0.,-8.02657851115159E-15));
#47389=CARTESIAN_POINT('Origin',(68.2773500981126,0.,-8.02657851115159E-15));
#47390=CARTESIAN_POINT('Origin',(71.5,0.,0.));
#47391=CARTESIAN_POINT('',(72.,-121.,-1.4818226269683E-14));
#47392=CARTESIAN_POINT('Origin',(72.,0.,0.));
#47393=CARTESIAN_POINT('',(71.5,-124.,-1.51856203094272E-14));
#47394=CARTESIAN_POINT('Origin',(67.9386750490563,0.,-8.04850045876632E-15));
#47395=CARTESIAN_POINT('',(67.6,131.8,1.61408448127621E-14));
#47396=CARTESIAN_POINT('',(67.9386750490563,131.441987426416,1.60970009175327E-14));
#47397=CARTESIAN_POINT('',(67.6,-131.8,-1.61408448127621E-14));
#47398=CARTESIAN_POINT('Origin',(67.6,0.,-8.07042240638106E-15));
#47399=CARTESIAN_POINT('Origin',(67.6,0.,-8.07042240638106E-15));
#47400=CARTESIAN_POINT('Origin',(66.,0.,0.));
#47401=CARTESIAN_POINT('',(64.4,-134.2,-1.64347600445575E-14));
#47402=CARTESIAN_POINT('',(66.,-133.,-1.62878024286598E-14));
#47403=CARTESIAN_POINT('',(64.4,134.2,-1.64347600445575E-14));
#47404=CARTESIAN_POINT('Origin',(64.4,0.,-8.21738002227874E-15));
#47405=CARTESIAN_POINT('Origin',(64.4,0.,-8.21738002227874E-15));
#47406=CARTESIAN_POINT('Origin',(63.9659177056077,0.,-8.23193990075793E-15));
#47407=CARTESIAN_POINT('',(63.5318354112155,134.675561720794,1.64929995584742E-14));
#47408=CARTESIAN_POINT('',(63.9659177056077,134.437780860397,1.64638798015159E-14));
#47409=CARTESIAN_POINT('',(63.5318354112155,-134.675561720794,-1.64929995584742E-14));
#47410=CARTESIAN_POINT('Origin',(63.5318354112155,0.,-8.24649977923712E-15));
#47411=CARTESIAN_POINT('Origin',(63.5318354112155,0.,-8.24649977923712E-15));
#47412=CARTESIAN_POINT('Origin',(62.,0.,0.));
#47413=CARTESIAN_POINT('',(60.4681645887845,-135.824438279206,-1.66336963584617E-14));
#47414=CARTESIAN_POINT('',(62.,-135.25,-1.6563347958468E-14));
#47415=CARTESIAN_POINT('',(60.4681645887845,135.824438279206,-1.66336963584617E-14));
#47416=CARTESIAN_POINT('Origin',(60.4681645887845,0.,-8.31684817923083E-15));
#47417=CARTESIAN_POINT('Origin',(60.4681645887845,0.,-8.31684817923083E-15));
#47418=CARTESIAN_POINT('Origin',(59.9840822943923,0.,-4.15842408961541E-15));
#47419=CARTESIAN_POINT('',(59.5,136.,1.6655196468404E-14));
#47420=CARTESIAN_POINT('',(59.9840822943923,135.912219139603,1.66444464134328E-14));
#47421=CARTESIAN_POINT('',(59.5,-136.,-1.6655196468404E-14));
#47422=CARTESIAN_POINT('Origin',(59.5,0.,0.));
#47423=CARTESIAN_POINT('Origin',(59.5,0.,0.));
#47424=CARTESIAN_POINT('Origin',(36.,0.,0.));
#47425=CARTESIAN_POINT('',(58.,-136.,-1.6655196468404E-14));
#47426=CARTESIAN_POINT('',(36.,-136.,-1.6655196468404E-14));
#47427=CARTESIAN_POINT('',(58.,-135.997660312937,-0.797740187650247));
#47428=CARTESIAN_POINT('Origin',(58.,0.,0.));
#47429=CARTESIAN_POINT('',(57.5,-135.993780676136,-1.30062193238639));
#47430=CARTESIAN_POINT('Origin',(72.3260541341288,0.,0.));
#47431=CARTESIAN_POINT('',(14.5,-135.993780676136,-1.30062193238639));
#47432=CARTESIAN_POINT('',(36.,-135.993780676136,-1.30062193238639));
#47433=CARTESIAN_POINT('',(14.,-135.997660312937,-0.797740187650244));
#47434=CARTESIAN_POINT('Origin',(-0.32605413412881,0.,0.));
#47435=CARTESIAN_POINT('',(14.,-136.,-1.6655196468404E-14));
#47436=CARTESIAN_POINT('Origin',(14.,0.,0.));
#47437=CARTESIAN_POINT('',(12.,-136.,-1.6655196468404E-14));
#47438=CARTESIAN_POINT('',(36.,-136.,-1.6655196468404E-14));
#47439=CARTESIAN_POINT('Origin',(12.,0.,0.));
#47440=CARTESIAN_POINT('',(14.,-135.997660312937,0.797740187650262));
#47441=CARTESIAN_POINT('Origin',(14.,0.,0.));
#47442=CARTESIAN_POINT('',(14.5,-135.993780676136,1.3006219323864));
#47443=CARTESIAN_POINT('Origin',(-0.32605413412885,0.,0.));
#47444=CARTESIAN_POINT('',(57.5,-135.993780676136,1.3006219323864));
#47445=CARTESIAN_POINT('',(36.,-135.993780676136,1.3006219323864));
#47446=CARTESIAN_POINT('',(58.,-135.997660312937,0.797740187650262));
#47447=CARTESIAN_POINT('Origin',(72.3260541341288,0.,0.));
#47448=CARTESIAN_POINT('Origin',(58.,0.,0.));
#47449=CARTESIAN_POINT('',(57.5,-1.3006219323864,135.993780676136));
#47450=CARTESIAN_POINT('',(14.5,-1.3006219323864,135.993780676136));
#47451=CARTESIAN_POINT('',(36.,-1.3006219323864,135.993780676136));
#47452=CARTESIAN_POINT('',(14.,-0.797740187650253,135.997660312937));
#47453=CARTESIAN_POINT('Origin',(-0.326054134128819,0.,0.));
#47454=CARTESIAN_POINT('',(14.,0.797740187650255,135.997660312937));
#47455=CARTESIAN_POINT('Origin',(14.,0.,0.));
#47456=CARTESIAN_POINT('',(14.5,1.3006219323864,135.993780676136));
#47457=CARTESIAN_POINT('Origin',(-0.326054134128837,0.,0.));
#47458=CARTESIAN_POINT('',(57.5,1.3006219323864,135.993780676136));
#47459=CARTESIAN_POINT('',(36.,1.3006219323864,135.993780676136));
#47460=CARTESIAN_POINT('',(58.,0.797740187650255,135.997660312937));
#47461=CARTESIAN_POINT('Origin',(72.3260541341288,0.,0.));
#47462=CARTESIAN_POINT('',(58.,-0.797740187650253,135.997660312937));
#47463=CARTESIAN_POINT('Origin',(58.,0.,0.));
#47464=CARTESIAN_POINT('Origin',(72.3260541341288,0.,0.));
#47465=CARTESIAN_POINT('',(57.5,-13.1483116371559,135.362926612467));
#47466=CARTESIAN_POINT('',(14.5,-13.1483116371559,135.362926612467));
#47467=CARTESIAN_POINT('',(36.,-13.1483116371559,135.362926612467));
#47468=CARTESIAN_POINT('',(14.,-12.6476816419096,135.410620518056));
#47469=CARTESIAN_POINT('Origin',(-0.32605413412881,0.,0.));
#47470=CARTESIAN_POINT('',(14.,-11.0582725511258,135.549675795204));
#47471=CARTESIAN_POINT('Origin',(14.,0.,0.));
#47472=CARTESIAN_POINT('',(14.5,-10.5569662906256,135.589639953569));
#47473=CARTESIAN_POINT('Origin',(-0.326054134128801,0.,0.));
#47474=CARTESIAN_POINT('',(57.5,-10.5569662906256,135.589639953569));
#47475=CARTESIAN_POINT('',(36.,-10.5569662906256,135.589639953569));
#47476=CARTESIAN_POINT('',(58.,-11.0582725511258,135.549675795204));
#47477=CARTESIAN_POINT('Origin',(72.3260541341287,0.,0.));
#47478=CARTESIAN_POINT('',(58.,-12.6476816419096,135.410620518056));
#47479=CARTESIAN_POINT('Origin',(58.,0.,0.));
#47480=CARTESIAN_POINT('Origin',(72.3260541341288,0.,0.));
#47481=CARTESIAN_POINT('',(57.5,-24.8959347511991,133.701878942908));
#47482=CARTESIAN_POINT('',(14.5,-24.8959347511991,133.701878942908));
#47483=CARTESIAN_POINT('',(36.,-24.8959347511991,133.701878942908));
#47484=CARTESIAN_POINT('',(14.,-24.4013666019951,133.793024137864));
#47485=CARTESIAN_POINT('Origin',(-0.326054134128935,0.,0.));
#47486=CARTESIAN_POINT('',(14.,-22.8301251586203,134.070076397538));
#47487=CARTESIAN_POINT('Origin',(14.,0.,0.));
#47488=CARTESIAN_POINT('',(14.5,-22.3342096256954,134.153580199693));
#47489=CARTESIAN_POINT('Origin',(-0.32605413412921,0.,0.));
#47490=CARTESIAN_POINT('',(57.5,-22.3342096256954,134.153580199693));
#47491=CARTESIAN_POINT('',(36.,-22.3342096256954,134.153580199693));
#47492=CARTESIAN_POINT('',(58.,-22.8301251586203,134.070076397538));
#47493=CARTESIAN_POINT('Origin',(72.326054134129,0.,0.));
#47494=CARTESIAN_POINT('',(58.,-24.4013666019951,133.793024137864));
#47495=CARTESIAN_POINT('Origin',(58.,0.,0.));
#47496=CARTESIAN_POINT('Origin',(72.3260541341287,0.,0.));
#47497=CARTESIAN_POINT('',(57.5,-36.4540847692092,131.023279243191));
#47498=CARTESIAN_POINT('',(14.5,-36.4540847692092,131.023279243191));
#47499=CARTESIAN_POINT('',(36.,-36.4540847692092,131.023279243191));
#47500=CARTESIAN_POINT('',(14.,-35.9693424282914,131.157182057546));
#47501=CARTESIAN_POINT('Origin',(-0.326054134128735,0.,0.));
#47502=CARTESIAN_POINT('',(14.,-34.4282267284513,131.570122764761));
#47503=CARTESIAN_POINT('Origin',(14.,0.,0.));
#47504=CARTESIAN_POINT('',(14.5,-33.9414761397491,131.696530696351));
#47505=CARTESIAN_POINT('Origin',(-0.326054134129108,0.,0.));
#47506=CARTESIAN_POINT('',(57.5,-33.9414761397491,131.696530696351));
#47507=CARTESIAN_POINT('',(36.,-33.9414761397491,131.696530696351));
#47508=CARTESIAN_POINT('',(58.,-34.4282267284513,131.570122764761));
#47509=CARTESIAN_POINT('Origin',(72.3260541341289,0.,0.));
#47510=CARTESIAN_POINT('',(58.,-35.9693424282914,131.157182057546));
#47511=CARTESIAN_POINT('Origin',(58.,0.,0.));
#47512=CARTESIAN_POINT('Origin',(72.3260541341287,0.,0.));
#47513=CARTESIAN_POINT('',(57.5,-47.7347971905474,127.347513274415));
#47514=CARTESIAN_POINT('',(14.5,-47.7347971905474,127.347513274415));
#47515=CARTESIAN_POINT('',(36.,-47.7347971905474,127.347513274415));
#47516=CARTESIAN_POINT('',(14.,-47.2635698398256,127.523154626899));
#47517=CARTESIAN_POINT('Origin',(-0.326054134129197,0.,0.));
#47518=CARTESIAN_POINT('',(14.,-45.764308704547,128.068841053532));
#47519=CARTESIAN_POINT('Origin',(14.,0.,0.));
#47520=CARTESIAN_POINT('',(14.5,-45.2904275259558,128.23719107387));
#47521=CARTESIAN_POINT('Origin',(-0.326054134128597,0.,0.));
#47522=CARTESIAN_POINT('',(57.5,-45.2904275259558,128.23719107387));
#47523=CARTESIAN_POINT('',(36.,-45.2904275259558,128.23719107387));
#47524=CARTESIAN_POINT('',(58.,-45.764308704547,128.068841053532));
#47525=CARTESIAN_POINT('Origin',(72.3260541341288,0.,0.));
#47526=CARTESIAN_POINT('',(58.,-47.2635698398257,127.523154626899));
#47527=CARTESIAN_POINT('Origin',(58.,0.,0.));
#47528=CARTESIAN_POINT('Origin',(72.3260541341294,0.,0.));
#47529=CARTESIAN_POINT('',(57.5,-58.652218982207,122.702555835089));
#47530=CARTESIAN_POINT('',(14.5,-58.652218982207,122.702555835089));
#47531=CARTESIAN_POINT('',(36.,-58.652218982207,122.702555835089));
#47532=CARTESIAN_POINT('',(14.,-58.198092946355,122.918598988955));
#47533=CARTESIAN_POINT('Origin',(-0.326054134128229,0.,0.));
#47534=CARTESIAN_POINT('',(14.,-56.7520966581561,123.592878131805));
#47535=CARTESIAN_POINT('Origin',(14.,0.,0.));
#47536=CARTESIAN_POINT('',(14.5,-56.2946914115821,123.801888995583));
#47537=CARTESIAN_POINT('Origin',(-0.326054134128895,0.,0.));
#47538=CARTESIAN_POINT('',(57.5,-56.2946914115821,123.801888995583));
#47539=CARTESIAN_POINT('',(36.,-56.2946914115821,123.801888995583));
#47540=CARTESIAN_POINT('',(58.,-56.7520966581561,123.592878131805));
#47541=CARTESIAN_POINT('Origin',(72.3260541341286,0.,0.));
#47542=CARTESIAN_POINT('',(58.,-58.198092946355,122.918598988955));
#47543=CARTESIAN_POINT('Origin',(58.,0.,0.));
#47544=CARTESIAN_POINT('Origin',(72.3260541341284,0.,0.));
#47545=CARTESIAN_POINT('',(57.5,-69.1232619722338,117.12375785603));
#47546=CARTESIAN_POINT('',(14.5,-69.1232619722338,117.12375785603));
#47547=CARTESIAN_POINT('',(36.,-69.1232619722338,117.12375785603));
#47548=CARTESIAN_POINT('',(14.,-68.6896934245934,117.378558592425));
#47549=CARTESIAN_POINT('Origin',(-0.326054134128499,0.,0.));
#47550=CARTESIAN_POINT('',(14.,-67.3079668883436,118.176298780075));
#47551=CARTESIAN_POINT('Origin',(14.,0.,0.));
#47552=CARTESIAN_POINT('',(14.5,-66.8705187039022,118.424379788416));
#47553=CARTESIAN_POINT('Origin',(-0.326054134129121,0.,0.));
#47554=CARTESIAN_POINT('',(57.5,-66.8705187039022,118.424379788416));
#47555=CARTESIAN_POINT('',(36.,-66.8705187039022,118.424379788416));
#47556=CARTESIAN_POINT('',(58.,-67.3079668883436,118.176298780075));
#47557=CARTESIAN_POINT('Origin',(72.3260541341291,0.,0.));
#47558=CARTESIAN_POINT('',(58.,-68.6896934245934,117.378558592425));
#47559=CARTESIAN_POINT('Origin',(58.,0.,0.));
#47560=CARTESIAN_POINT('Origin',(72.3260541341284,0.,0.));
#47561=CARTESIAN_POINT('',(57.5,-79.0682352008853,110.653577358427));
#47562=CARTESIAN_POINT('',(14.5,-79.0682352008853,110.653577358427));
#47563=CARTESIAN_POINT('',(36.,-79.0682352008853,110.653577358427));
#47564=CARTESIAN_POINT('',(14.,-78.6585238598997,110.945196489896));
#47565=CARTESIAN_POINT('Origin',(-0.326054134129188,0.,0.));
#47566=CARTESIAN_POINT('',(14.,-77.3515828488493,111.860326437829));
#47567=CARTESIAN_POINT('Origin',(14.,0.,0.));
#47568=CARTESIAN_POINT('',(14.5,-76.9374209713625,112.145589544464));
#47569=CARTESIAN_POINT('Origin',(-0.326054134128935,0.,0.));
#47570=CARTESIAN_POINT('',(57.5,-76.9374209713625,112.145589544464));
#47571=CARTESIAN_POINT('',(36.,-76.9374209713625,112.145589544464));
#47572=CARTESIAN_POINT('',(58.,-77.3515828488493,111.860326437829));
#47573=CARTESIAN_POINT('Origin',(72.3260541341289,0.,0.));
#47574=CARTESIAN_POINT('',(58.,-78.6585238598997,110.945196489896));
#47575=CARTESIAN_POINT('Origin',(58.,0.,0.));
#47576=CARTESIAN_POINT('Origin',(72.3260541341289,0.,0.));
#47577=CARTESIAN_POINT('',(57.5,-88.4114514169522,103.341256322671));
#47578=CARTESIAN_POINT('',(14.5,-88.4114514169522,103.341256322671));
#47579=CARTESIAN_POINT('',(36.,-88.4114514169522,103.341256322671));
#47580=CARTESIAN_POINT('',(14.,-88.0287154333169,103.667474451537));
#47581=CARTESIAN_POINT('Origin',(-0.326054134129112,0.,0.));
#47582=CARTESIAN_POINT('',(14.,-86.8065065577125,104.693029468278));
#47583=CARTESIAN_POINT('Origin',(14.,0.,0.));
#47584=CARTESIAN_POINT('',(14.5,-86.4187830091457,105.01330364872));
#47585=CARTESIAN_POINT('Origin',(-0.326054134129139,0.,0.));
#47586=CARTESIAN_POINT('',(57.5,-86.4187830091457,105.01330364872));
#47587=CARTESIAN_POINT('',(36.,-86.4187830091457,105.01330364872));
#47588=CARTESIAN_POINT('',(58.,-86.8065065577126,104.693029468278));
#47589=CARTESIAN_POINT('Origin',(72.3260541341287,0.,0.));
#47590=CARTESIAN_POINT('',(58.,-88.0287154333169,103.667474451537));
#47591=CARTESIAN_POINT('Origin',(58.,0.,0.));
#47592=CARTESIAN_POINT('Origin',(72.3260541341291,0.,0.));
#47593=CARTESIAN_POINT('',(57.5,-97.0818031034423,95.2424459271415));
#47594=CARTESIAN_POINT('',(14.5,-97.0818031034423,95.2424459271415));
#47595=CARTESIAN_POINT('',(36.,-97.0818031034423,95.2424459271415));
#47596=CARTESIAN_POINT('',(14.,-96.7289553290949,95.6007803364699));
#47597=CARTESIAN_POINT('Origin',(-0.32605413412873,0.,0.));
#47598=CARTESIAN_POINT('',(14.,-95.6007803364699,96.7289553290949));
#47599=CARTESIAN_POINT('Origin',(14.,0.,0.));
#47600=CARTESIAN_POINT('',(14.5,-95.2424459271415,97.0818031034423));
#47601=CARTESIAN_POINT('Origin',(-0.326054134128722,0.,0.));
#47602=CARTESIAN_POINT('',(57.5,-95.2424459271415,97.0818031034423));
#47603=CARTESIAN_POINT('',(36.,-95.2424459271415,97.0818031034423));
#47604=CARTESIAN_POINT('',(58.,-95.6007803364699,96.7289553290949));
#47605=CARTESIAN_POINT('Origin',(72.3260541341287,0.,0.));
#47606=CARTESIAN_POINT('',(58.,-96.7289553290949,95.6007803364699));
#47607=CARTESIAN_POINT('Origin',(58.,0.,0.));
#47608=CARTESIAN_POINT('Origin',(72.3260541341287,0.,0.));
#47609=CARTESIAN_POINT('',(57.5,-105.01330364872,86.4187830091457));
#47610=CARTESIAN_POINT('',(14.5,-105.01330364872,86.4187830091457));
#47611=CARTESIAN_POINT('',(36.,-105.01330364872,86.4187830091457));
#47612=CARTESIAN_POINT('',(14.,-104.693029468278,86.8065065577126));
#47613=CARTESIAN_POINT('Origin',(-0.326054134128375,0.,0.));
#47614=CARTESIAN_POINT('',(14.,-103.667474451537,88.0287154333169));
#47615=CARTESIAN_POINT('Origin',(14.,0.,0.));
#47616=CARTESIAN_POINT('',(14.5,-103.341256322671,88.4114514169522));
#47617=CARTESIAN_POINT('Origin',(-0.326054134128864,0.,0.));
#47618=CARTESIAN_POINT('',(57.5,-103.341256322671,88.4114514169522));
#47619=CARTESIAN_POINT('',(36.,-103.341256322671,88.4114514169522));
#47620=CARTESIAN_POINT('',(58.,-103.667474451537,88.0287154333169));
#47621=CARTESIAN_POINT('Origin',(72.3260541341288,0.,0.));
#47622=CARTESIAN_POINT('',(58.,-104.693029468278,86.8065065577126));
#47623=CARTESIAN_POINT('Origin',(58.,0.,0.));
#47624=CARTESIAN_POINT('Origin',(72.3260541341287,0.,0.));
#47625=CARTESIAN_POINT('',(57.5,-112.145589544464,76.9374209713625));
#47626=CARTESIAN_POINT('',(14.5,-112.145589544464,76.9374209713625));
#47627=CARTESIAN_POINT('',(36.,-112.145589544464,76.9374209713625));
#47628=CARTESIAN_POINT('',(14.,-111.860326437829,77.3515828488493));
#47629=CARTESIAN_POINT('Origin',(-0.32605413412869,0.,0.));
#47630=CARTESIAN_POINT('',(14.,-110.945196489896,78.6585238598997));
#47631=CARTESIAN_POINT('Origin',(14.,0.,0.));
#47632=CARTESIAN_POINT('',(14.5,-110.653577358427,79.0682352008853));
#47633=CARTESIAN_POINT('Origin',(-0.326054134128939,0.,0.));
#47634=CARTESIAN_POINT('',(57.5,-110.653577358427,79.0682352008853));
#47635=CARTESIAN_POINT('',(36.,-110.653577358427,79.0682352008853));
#47636=CARTESIAN_POINT('',(58.,-110.945196489896,78.6585238598997));
#47637=CARTESIAN_POINT('Origin',(72.3260541341289,0.,0.));
#47638=CARTESIAN_POINT('',(58.,-111.860326437829,77.3515828488493));
#47639=CARTESIAN_POINT('Origin',(58.,0.,0.));
#47640=CARTESIAN_POINT('Origin',(72.3260541341286,0.,0.));
#47641=CARTESIAN_POINT('',(57.5,-118.424379788416,66.8705187039022));
#47642=CARTESIAN_POINT('',(14.5,-118.424379788416,66.8705187039022));
#47643=CARTESIAN_POINT('',(36.,-118.424379788416,66.8705187039022));
#47644=CARTESIAN_POINT('',(14.,-118.176298780075,67.3079668883436));
#47645=CARTESIAN_POINT('Origin',(-0.326054134129148,0.,0.));
#47646=CARTESIAN_POINT('',(14.,-117.378558592425,68.6896934245934));
#47647=CARTESIAN_POINT('Origin',(14.,0.,0.));
#47648=CARTESIAN_POINT('',(14.5,-117.12375785603,69.1232619722339));
#47649=CARTESIAN_POINT('Origin',(-0.326054134128753,0.,0.));
#47650=CARTESIAN_POINT('',(57.5,-117.12375785603,69.1232619722339));
#47651=CARTESIAN_POINT('',(36.,-117.12375785603,69.1232619722339));
#47652=CARTESIAN_POINT('',(58.,-117.378558592425,68.6896934245934));
#47653=CARTESIAN_POINT('Origin',(72.3260541341287,0.,0.));
#47654=CARTESIAN_POINT('',(58.,-118.176298780075,67.3079668883436));
#47655=CARTESIAN_POINT('Origin',(58.,0.,0.));
#47656=CARTESIAN_POINT('Origin',(72.3260541341285,0.,0.));
#47657=CARTESIAN_POINT('',(57.5,-123.801888995583,56.2946914115821));
#47658=CARTESIAN_POINT('',(14.5,-123.801888995583,56.2946914115821));
#47659=CARTESIAN_POINT('',(36.,-123.801888995583,56.2946914115821));
#47660=CARTESIAN_POINT('',(14.,-123.592878131805,56.7520966581561));
#47661=CARTESIAN_POINT('Origin',(-0.32605413412869,0.,0.));
#47662=CARTESIAN_POINT('',(14.,-122.918598988955,58.198092946355));
#47663=CARTESIAN_POINT('Origin',(14.,0.,0.));
#47664=CARTESIAN_POINT('',(14.5,-122.702555835089,58.652218982207));
#47665=CARTESIAN_POINT('Origin',(-0.326054134128726,0.,0.));
#47666=CARTESIAN_POINT('',(57.5,-122.702555835089,58.652218982207));
#47667=CARTESIAN_POINT('',(36.,-122.702555835089,58.652218982207));
#47668=CARTESIAN_POINT('',(58.,-122.918598988955,58.198092946355));
#47669=CARTESIAN_POINT('Origin',(72.3260541341287,0.,0.));
#47670=CARTESIAN_POINT('',(58.,-123.592878131805,56.7520966581561));
#47671=CARTESIAN_POINT('Origin',(58.,0.,0.));
#47672=CARTESIAN_POINT('Origin',(72.3260541341286,0.,0.));
#47673=CARTESIAN_POINT('',(57.5,-128.23719107387,45.2904275259558));
#47674=CARTESIAN_POINT('',(14.5,-128.23719107387,45.2904275259558));
#47675=CARTESIAN_POINT('',(36.,-128.23719107387,45.2904275259558));
#47676=CARTESIAN_POINT('',(14.,-128.068841053532,45.764308704547));
#47677=CARTESIAN_POINT('Origin',(-0.326054134128846,0.,0.));
#47678=CARTESIAN_POINT('',(14.,-127.523154626899,47.2635698398257));
#47679=CARTESIAN_POINT('Origin',(14.,0.,0.));
#47680=CARTESIAN_POINT('',(14.5,-127.347513274415,47.7347971905474));
#47681=CARTESIAN_POINT('Origin',(-0.326054134129197,0.,0.));
#47682=CARTESIAN_POINT('',(57.5,-127.347513274415,47.7347971905474));
#47683=CARTESIAN_POINT('',(36.,-127.347513274415,47.7347971905474));
#47684=CARTESIAN_POINT('',(58.,-127.523154626899,47.2635698398257));
#47685=CARTESIAN_POINT('Origin',(72.3260541341291,0.,0.));
#47686=CARTESIAN_POINT('',(58.,-128.068841053532,45.764308704547));
#47687=CARTESIAN_POINT('Origin',(58.,0.,0.));
#47688=CARTESIAN_POINT('Origin',(72.3260541341288,0.,0.));
#47689=CARTESIAN_POINT('',(57.5,-131.696530696351,33.9414761397492));
#47690=CARTESIAN_POINT('',(14.5,-131.696530696351,33.9414761397492));
#47691=CARTESIAN_POINT('',(36.,-131.696530696351,33.9414761397492));
#47692=CARTESIAN_POINT('',(14.,-131.570122764761,34.4282267284513));
#47693=CARTESIAN_POINT('Origin',(-0.326054134128975,0.,0.));
#47694=CARTESIAN_POINT('',(14.,-131.157182057546,35.9693424282914));
#47695=CARTESIAN_POINT('Origin',(14.,0.,0.));
#47696=CARTESIAN_POINT('',(14.5,-131.023279243191,36.4540847692092));
#47697=CARTESIAN_POINT('Origin',(-0.326054134128864,0.,0.));
#47698=CARTESIAN_POINT('',(57.5,-131.023279243191,36.4540847692092));
#47699=CARTESIAN_POINT('',(36.,-131.023279243191,36.4540847692092));
#47700=CARTESIAN_POINT('',(58.,-131.157182057546,35.9693424282914));
#47701=CARTESIAN_POINT('Origin',(72.3260541341288,0.,0.));
#47702=CARTESIAN_POINT('',(58.,-131.570122764761,34.4282267284513));
#47703=CARTESIAN_POINT('Origin',(58.,0.,0.));
#47704=CARTESIAN_POINT('Origin',(72.3260541341289,0.,0.));
#47705=CARTESIAN_POINT('',(57.5,-134.153580199693,22.3342096256954));
#47706=CARTESIAN_POINT('',(14.5,-134.153580199693,22.3342096256954));
#47707=CARTESIAN_POINT('',(36.,-134.153580199693,22.3342096256954));
#47708=CARTESIAN_POINT('',(14.,-134.070076397538,22.8301251586204));
#47709=CARTESIAN_POINT('Origin',(-0.326054134128957,0.,0.));
#47710=CARTESIAN_POINT('',(14.,-133.793024137864,24.4013666019951));
#47711=CARTESIAN_POINT('Origin',(14.,0.,0.));
#47712=CARTESIAN_POINT('',(14.5,-133.701878942908,24.8959347511991));
#47713=CARTESIAN_POINT('Origin',(-0.326054134128939,0.,0.));
#47714=CARTESIAN_POINT('',(57.5,-133.701878942908,24.8959347511991));
#47715=CARTESIAN_POINT('',(36.,-133.701878942908,24.8959347511991));
#47716=CARTESIAN_POINT('',(58.,-133.793024137864,24.4013666019951));
#47717=CARTESIAN_POINT('Origin',(72.3260541341289,0.,0.));
#47718=CARTESIAN_POINT('',(58.,-134.070076397538,22.8301251586204));
#47719=CARTESIAN_POINT('Origin',(58.,0.,0.));
#47720=CARTESIAN_POINT('Origin',(72.3260541341289,0.,0.));
#47721=CARTESIAN_POINT('',(57.5,-135.589639953569,10.5569662906256));
#47722=CARTESIAN_POINT('',(14.5,-135.589639953569,10.5569662906256));
#47723=CARTESIAN_POINT('',(36.,-135.589639953569,10.5569662906256));
#47724=CARTESIAN_POINT('',(14.,-135.549675795204,11.0582725511259));
#47725=CARTESIAN_POINT('Origin',(-0.32605413412893,0.,0.));
#47726=CARTESIAN_POINT('',(14.,-135.410620518056,12.6476816419097));
#47727=CARTESIAN_POINT('Origin',(14.,0.,0.));
#47728=CARTESIAN_POINT('',(14.5,-135.362926612467,13.148311637156));
#47729=CARTESIAN_POINT('Origin',(-0.32605413412881,0.,0.));
#47730=CARTESIAN_POINT('',(57.5,-135.362926612467,13.148311637156));
#47731=CARTESIAN_POINT('',(36.,-135.362926612467,13.148311637156));
#47732=CARTESIAN_POINT('',(58.,-135.410620518056,12.6476816419097));
#47733=CARTESIAN_POINT('Origin',(72.3260541341288,0.,0.));
#47734=CARTESIAN_POINT('',(58.,-135.549675795204,11.0582725511259));
#47735=CARTESIAN_POINT('Origin',(58.,0.,0.));
#47736=CARTESIAN_POINT('Origin',(72.3260541341289,0.,0.));
#47737=CARTESIAN_POINT('',(57.5,-135.362926612467,-13.1483116371559));
#47738=CARTESIAN_POINT('',(14.5,-135.362926612467,-13.1483116371559));
#47739=CARTESIAN_POINT('',(36.,-135.362926612467,-13.1483116371559));
#47740=CARTESIAN_POINT('',(14.,-135.410620518056,-12.6476816419096));
#47741=CARTESIAN_POINT('Origin',(-0.32605413412881,0.,0.));
#47742=CARTESIAN_POINT('',(14.,-135.549675795204,-11.0582725511258));
#47743=CARTESIAN_POINT('Origin',(14.,0.,0.));
#47744=CARTESIAN_POINT('',(14.5,-135.589639953569,-10.5569662906256));
#47745=CARTESIAN_POINT('Origin',(-0.326054134128806,0.,0.));
#47746=CARTESIAN_POINT('',(57.5,-135.589639953569,-10.5569662906256));
#47747=CARTESIAN_POINT('',(36.,-135.589639953569,-10.5569662906256));
#47748=CARTESIAN_POINT('',(58.,-135.549675795204,-11.0582725511258));
#47749=CARTESIAN_POINT('Origin',(72.3260541341287,0.,0.));
#47750=CARTESIAN_POINT('',(58.,-135.410620518056,-12.6476816419096));
#47751=CARTESIAN_POINT('Origin',(58.,0.,0.));
#47752=CARTESIAN_POINT('Origin',(72.3260541341288,0.,0.));
#47753=CARTESIAN_POINT('',(57.5,-133.701878942908,-24.8959347511991));
#47754=CARTESIAN_POINT('',(14.5,-133.701878942908,-24.8959347511991));
#47755=CARTESIAN_POINT('',(36.,-133.701878942908,-24.8959347511991));
#47756=CARTESIAN_POINT('',(14.,-133.793024137864,-24.4013666019951));
#47757=CARTESIAN_POINT('Origin',(-0.326054134128806,0.,0.));
#47758=CARTESIAN_POINT('',(14.,-134.070076397538,-22.8301251586203));
#47759=CARTESIAN_POINT('Origin',(14.,0.,0.));
#47760=CARTESIAN_POINT('',(14.5,-134.153580199693,-22.3342096256954));
#47761=CARTESIAN_POINT('Origin',(-0.32605413412921,0.,0.));
#47762=CARTESIAN_POINT('',(57.5,-134.153580199693,-22.3342096256954));
#47763=CARTESIAN_POINT('',(36.,-134.153580199693,-22.3342096256954));
#47764=CARTESIAN_POINT('',(58.,-134.070076397538,-22.8301251586203));
#47765=CARTESIAN_POINT('Origin',(72.3260541341289,0.,0.));
#47766=CARTESIAN_POINT('',(58.,-133.793024137864,-24.4013666019951));
#47767=CARTESIAN_POINT('Origin',(58.,0.,0.));
#47768=CARTESIAN_POINT('Origin',(72.3260541341287,0.,0.));
#47769=CARTESIAN_POINT('',(57.5,-131.023279243191,-36.4540847692092));
#47770=CARTESIAN_POINT('',(14.5,-131.023279243191,-36.4540847692092));
#47771=CARTESIAN_POINT('',(36.,-131.023279243191,-36.4540847692092));
#47772=CARTESIAN_POINT('',(14.,-131.157182057546,-35.9693424282914));
#47773=CARTESIAN_POINT('Origin',(-0.326054134128735,0.,0.));
#47774=CARTESIAN_POINT('',(14.,-131.570122764761,-34.4282267284513));
#47775=CARTESIAN_POINT('Origin',(14.,0.,0.));
#47776=CARTESIAN_POINT('',(14.5,-131.696530696351,-33.9414761397491));
#47777=CARTESIAN_POINT('Origin',(-0.326054134128984,0.,0.));
#47778=CARTESIAN_POINT('',(57.5,-131.696530696351,-33.9414761397491));
#47779=CARTESIAN_POINT('',(36.,-131.696530696351,-33.9414761397491));
#47780=CARTESIAN_POINT('',(58.,-131.570122764761,-34.4282267284513));
#47781=CARTESIAN_POINT('Origin',(72.3260541341289,0.,0.));
#47782=CARTESIAN_POINT('',(58.,-131.157182057546,-35.9693424282914));
#47783=CARTESIAN_POINT('Origin',(58.,0.,0.));
#47784=CARTESIAN_POINT('Origin',(72.3260541341289,0.,0.));
#47785=CARTESIAN_POINT('',(57.5,-127.347513274415,-47.7347971905474));
#47786=CARTESIAN_POINT('',(14.5,-127.347513274415,-47.7347971905474));
#47787=CARTESIAN_POINT('',(36.,-127.347513274415,-47.7347971905474));
#47788=CARTESIAN_POINT('',(14.,-127.523154626899,-47.2635698398256));
#47789=CARTESIAN_POINT('Origin',(-0.326054134129197,0.,0.));
#47790=CARTESIAN_POINT('',(14.,-128.068841053532,-45.764308704547));
#47791=CARTESIAN_POINT('Origin',(14.,0.,0.));
#47792=CARTESIAN_POINT('',(14.5,-128.23719107387,-45.2904275259558));
#47793=CARTESIAN_POINT('Origin',(-0.326054134128606,0.,0.));
#47794=CARTESIAN_POINT('',(57.5,-128.23719107387,-45.2904275259558));
#47795=CARTESIAN_POINT('',(36.,-128.23719107387,-45.2904275259558));
#47796=CARTESIAN_POINT('',(58.,-128.068841053532,-45.764308704547));
#47797=CARTESIAN_POINT('Origin',(72.3260541341288,0.,0.));
#47798=CARTESIAN_POINT('',(58.,-127.523154626899,-47.2635698398257));
#47799=CARTESIAN_POINT('Origin',(58.,0.,0.));
#47800=CARTESIAN_POINT('Origin',(72.3260541341294,0.,0.));
#47801=CARTESIAN_POINT('',(57.5,-122.702555835089,-58.652218982207));
#47802=CARTESIAN_POINT('',(14.5,-122.702555835089,-58.652218982207));
#47803=CARTESIAN_POINT('',(36.,-122.702555835089,-58.652218982207));
#47804=CARTESIAN_POINT('',(14.,-122.918598988955,-58.198092946355));
#47805=CARTESIAN_POINT('Origin',(-0.326054134128735,0.,0.));
#47806=CARTESIAN_POINT('',(14.,-123.592878131805,-56.752096658156));
#47807=CARTESIAN_POINT('Origin',(14.,0.,0.));
#47808=CARTESIAN_POINT('',(14.5,-123.801888995583,-56.2946914115821));
#47809=CARTESIAN_POINT('Origin',(-0.326054134129112,0.,0.));
#47810=CARTESIAN_POINT('',(57.5,-123.801888995583,-56.2946914115821));
#47811=CARTESIAN_POINT('',(36.,-123.801888995583,-56.2946914115821));
#47812=CARTESIAN_POINT('',(58.,-123.592878131805,-56.752096658156));
#47813=CARTESIAN_POINT('Origin',(72.3260541341288,0.,0.));
#47814=CARTESIAN_POINT('',(58.,-122.918598988955,-58.198092946355));
#47815=CARTESIAN_POINT('Origin',(58.,0.,0.));
#47816=CARTESIAN_POINT('Origin',(72.3260541341287,0.,0.));
#47817=CARTESIAN_POINT('',(57.5,-117.12375785603,-69.1232619722338));
#47818=CARTESIAN_POINT('',(14.5,-117.12375785603,-69.1232619722338));
#47819=CARTESIAN_POINT('',(36.,-117.12375785603,-69.1232619722338));
#47820=CARTESIAN_POINT('',(14.,-117.378558592425,-68.6896934245934));
#47821=CARTESIAN_POINT('Origin',(-0.32605413412877,0.,0.));
#47822=CARTESIAN_POINT('',(14.,-118.176298780075,-67.3079668883436));
#47823=CARTESIAN_POINT('Origin',(14.,0.,0.));
#47824=CARTESIAN_POINT('',(14.5,-118.424379788416,-66.8705187039022));
#47825=CARTESIAN_POINT('Origin',(-0.326054134129108,0.,0.));
#47826=CARTESIAN_POINT('',(57.5,-118.424379788416,-66.8705187039022));
#47827=CARTESIAN_POINT('',(36.,-118.424379788416,-66.8705187039022));
#47828=CARTESIAN_POINT('',(58.,-118.176298780075,-67.3079668883436));
#47829=CARTESIAN_POINT('Origin',(72.3260541341291,0.,0.));
#47830=CARTESIAN_POINT('',(58.,-117.378558592425,-68.6896934245934));
#47831=CARTESIAN_POINT('Origin',(58.,0.,0.));
#47832=CARTESIAN_POINT('Origin',(72.3260541341287,0.,0.));
#47833=CARTESIAN_POINT('',(57.5,-110.653577358427,-79.0682352008852));
#47834=CARTESIAN_POINT('',(14.5,-110.653577358427,-79.0682352008852));
#47835=CARTESIAN_POINT('',(36.,-110.653577358427,-79.0682352008852));
#47836=CARTESIAN_POINT('',(14.,-110.945196489896,-78.6585238598997));
#47837=CARTESIAN_POINT('Origin',(-0.326054134128948,0.,0.));
#47838=CARTESIAN_POINT('',(14.,-111.860326437829,-77.3515828488493));
#47839=CARTESIAN_POINT('Origin',(14.,0.,0.));
#47840=CARTESIAN_POINT('',(14.5,-112.145589544464,-76.9374209713624));
#47841=CARTESIAN_POINT('Origin',(-0.326054134128895,0.,0.));
#47842=CARTESIAN_POINT('',(57.5,-112.145589544464,-76.9374209713624));
#47843=CARTESIAN_POINT('',(36.,-112.145589544464,-76.9374209713624));
#47844=CARTESIAN_POINT('',(58.,-111.860326437829,-77.3515828488493));
#47845=CARTESIAN_POINT('Origin',(72.3260541341289,0.,0.));
#47846=CARTESIAN_POINT('',(58.,-110.945196489896,-78.6585238598997));
#47847=CARTESIAN_POINT('Origin',(58.,0.,0.));
#47848=CARTESIAN_POINT('Origin',(72.3260541341289,0.,0.));
#47849=CARTESIAN_POINT('',(57.5,-103.341256322671,-88.4114514169522));
#47850=CARTESIAN_POINT('',(14.5,-103.341256322671,-88.4114514169522));
#47851=CARTESIAN_POINT('',(36.,-103.341256322671,-88.4114514169522));
#47852=CARTESIAN_POINT('',(14.,-103.667474451537,-88.0287154333169));
#47853=CARTESIAN_POINT('Origin',(-0.326054134129112,0.,0.));
#47854=CARTESIAN_POINT('',(14.,-104.693029468278,-86.8065065577126));
#47855=CARTESIAN_POINT('Origin',(14.,0.,0.));
#47856=CARTESIAN_POINT('',(14.5,-105.01330364872,-86.4187830091457));
#47857=CARTESIAN_POINT('Origin',(-0.326054134128748,0.,0.));
#47858=CARTESIAN_POINT('',(57.5,-105.01330364872,-86.4187830091457));
#47859=CARTESIAN_POINT('',(36.,-105.01330364872,-86.4187830091457));
#47860=CARTESIAN_POINT('',(58.,-104.693029468278,-86.8065065577126));
#47861=CARTESIAN_POINT('Origin',(72.3260541341287,0.,0.));
#47862=CARTESIAN_POINT('',(58.,-103.667474451537,-88.0287154333169));
#47863=CARTESIAN_POINT('Origin',(58.,0.,0.));
#47864=CARTESIAN_POINT('Origin',(72.3260541341291,0.,0.));
#47865=CARTESIAN_POINT('',(57.5,-95.2424459271415,-97.0818031034422));
#47866=CARTESIAN_POINT('',(14.5,-95.2424459271415,-97.0818031034422));
#47867=CARTESIAN_POINT('',(36.,-95.2424459271415,-97.0818031034422));
#47868=CARTESIAN_POINT('',(14.,-95.6007803364699,-96.7289553290949));
#47869=CARTESIAN_POINT('Origin',(-0.326054134128722,0.,0.));
#47870=CARTESIAN_POINT('',(14.,-96.7289553290949,-95.6007803364699));
#47871=CARTESIAN_POINT('Origin',(14.,0.,0.));
#47872=CARTESIAN_POINT('',(14.5,-97.0818031034423,-95.2424459271415));
#47873=CARTESIAN_POINT('Origin',(-0.326054134128717,0.,0.));
#47874=CARTESIAN_POINT('',(57.5,-97.0818031034423,-95.2424459271415));
#47875=CARTESIAN_POINT('',(36.,-97.0818031034423,-95.2424459271415));
#47876=CARTESIAN_POINT('',(58.,-96.7289553290949,-95.6007803364698));
#47877=CARTESIAN_POINT('Origin',(72.3260541341287,0.,0.));
#47878=CARTESIAN_POINT('',(58.,-95.6007803364699,-96.7289553290949));
#47879=CARTESIAN_POINT('Origin',(58.,0.,0.));
#47880=CARTESIAN_POINT('Origin',(72.3260541341287,0.,0.));
#47881=CARTESIAN_POINT('',(57.5,-86.4187830091457,-105.01330364872));
#47882=CARTESIAN_POINT('',(14.5,-86.4187830091457,-105.01330364872));
#47883=CARTESIAN_POINT('',(36.,-86.4187830091457,-105.01330364872));
#47884=CARTESIAN_POINT('',(14.,-86.8065065577126,-104.693029468278));
#47885=CARTESIAN_POINT('Origin',(-0.326054134128375,0.,0.));
#47886=CARTESIAN_POINT('',(14.,-88.0287154333169,-103.667474451537));
#47887=CARTESIAN_POINT('Origin',(14.,0.,0.));
#47888=CARTESIAN_POINT('',(14.5,-88.4114514169522,-103.34125632267));
#47889=CARTESIAN_POINT('Origin',(-0.326054134128846,0.,0.));
#47890=CARTESIAN_POINT('',(57.5,-88.4114514169522,-103.34125632267));
#47891=CARTESIAN_POINT('',(36.,-88.4114514169522,-103.34125632267));
#47892=CARTESIAN_POINT('',(58.,-88.0287154333169,-103.667474451537));
#47893=CARTESIAN_POINT('Origin',(72.3260541341288,0.,0.));
#47894=CARTESIAN_POINT('',(58.,-86.8065065577126,-104.693029468278));
#47895=CARTESIAN_POINT('Origin',(58.,0.,0.));
#47896=CARTESIAN_POINT('Origin',(72.3260541341283,0.,0.));
#47897=CARTESIAN_POINT('',(57.5,-76.9374209713625,-112.145589544464));
#47898=CARTESIAN_POINT('',(14.5,-76.9374209713625,-112.145589544464));
#47899=CARTESIAN_POINT('',(36.,-76.9374209713625,-112.145589544464));
#47900=CARTESIAN_POINT('',(14.,-77.3515828488493,-111.860326437829));
#47901=CARTESIAN_POINT('Origin',(-0.326054134129095,0.,0.));
#47902=CARTESIAN_POINT('',(14.,-78.6585238598997,-110.945196489896));
#47903=CARTESIAN_POINT('Origin',(14.,0.,0.));
#47904=CARTESIAN_POINT('',(14.5,-79.0682352008853,-110.653577358427));
#47905=CARTESIAN_POINT('Origin',(-0.326054134128939,0.,0.));
#47906=CARTESIAN_POINT('',(57.5,-79.0682352008853,-110.653577358427));
#47907=CARTESIAN_POINT('',(36.,-79.0682352008853,-110.653577358427));
#47908=CARTESIAN_POINT('',(58.,-78.6585238598997,-110.945196489896));
#47909=CARTESIAN_POINT('Origin',(72.3260541341289,0.,0.));
#47910=CARTESIAN_POINT('',(58.,-77.3515828488494,-111.860326437829));
#47911=CARTESIAN_POINT('Origin',(58.,0.,0.));
#47912=CARTESIAN_POINT('Origin',(72.3260541341286,0.,0.));
#47913=CARTESIAN_POINT('',(57.5,-66.8705187039022,-118.424379788416));
#47914=CARTESIAN_POINT('',(14.5,-66.8705187039022,-118.424379788416));
#47915=CARTESIAN_POINT('',(36.,-66.8705187039022,-118.424379788416));
#47916=CARTESIAN_POINT('',(14.,-67.3079668883436,-118.176298780075));
#47917=CARTESIAN_POINT('Origin',(-0.326054134128908,0.,0.));
#47918=CARTESIAN_POINT('',(14.,-68.6896934245934,-117.378558592425));
#47919=CARTESIAN_POINT('Origin',(14.,0.,0.));
#47920=CARTESIAN_POINT('',(14.5,-69.1232619722338,-117.12375785603));
#47921=CARTESIAN_POINT('Origin',(-0.326054134128504,0.,0.));
#47922=CARTESIAN_POINT('',(57.5,-69.1232619722338,-117.12375785603));
#47923=CARTESIAN_POINT('',(36.,-69.1232619722338,-117.12375785603));
#47924=CARTESIAN_POINT('',(58.,-68.6896934245934,-117.378558592425));
#47925=CARTESIAN_POINT('Origin',(72.3260541341287,0.,0.));
#47926=CARTESIAN_POINT('',(58.,-67.3079668883436,-118.176298780075));
#47927=CARTESIAN_POINT('Origin',(58.,0.,0.));
#47928=CARTESIAN_POINT('Origin',(72.3260541341288,0.,0.));
#47929=CARTESIAN_POINT('',(57.5,-56.2946914115821,-123.801888995583));
#47930=CARTESIAN_POINT('',(14.5,-56.2946914115821,-123.801888995583));
#47931=CARTESIAN_POINT('',(36.,-56.2946914115821,-123.801888995583));
#47932=CARTESIAN_POINT('',(14.,-56.7520966581561,-123.592878131805));
#47933=CARTESIAN_POINT('Origin',(-0.326054134128895,0.,0.));
#47934=CARTESIAN_POINT('',(14.,-58.198092946355,-122.918598988955));
#47935=CARTESIAN_POINT('Origin',(14.,0.,0.));
#47936=CARTESIAN_POINT('',(14.5,-58.652218982207,-122.702555835089));
#47937=CARTESIAN_POINT('Origin',(-0.326054134128477,0.,0.));
#47938=CARTESIAN_POINT('',(57.5,-58.652218982207,-122.702555835089));
#47939=CARTESIAN_POINT('',(36.,-58.652218982207,-122.702555835089));
#47940=CARTESIAN_POINT('',(58.,-58.198092946355,-122.918598988955));
#47941=CARTESIAN_POINT('Origin',(72.3260541341284,0.,0.));
#47942=CARTESIAN_POINT('',(58.,-56.7520966581561,-123.592878131805));
#47943=CARTESIAN_POINT('Origin',(58.,0.,0.));
#47944=CARTESIAN_POINT('Origin',(72.3260541341288,0.,0.));
#47945=CARTESIAN_POINT('',(57.5,-45.2904275259558,-128.23719107387));
#47946=CARTESIAN_POINT('',(14.5,-45.2904275259558,-128.23719107387));
#47947=CARTESIAN_POINT('',(36.,-45.2904275259558,-128.23719107387));
#47948=CARTESIAN_POINT('',(14.,-45.764308704547,-128.068841053532));
#47949=CARTESIAN_POINT('Origin',(-0.326054134129086,0.,0.));
#47950=CARTESIAN_POINT('',(14.,-47.2635698398257,-127.523154626899));
#47951=CARTESIAN_POINT('Origin',(14.,0.,0.));
#47952=CARTESIAN_POINT('',(14.5,-47.7347971905474,-127.347513274415));
#47953=CARTESIAN_POINT('Origin',(-0.326054134129183,0.,0.));
#47954=CARTESIAN_POINT('',(57.5,-47.7347971905474,-127.347513274415));
#47955=CARTESIAN_POINT('',(36.,-47.7347971905474,-127.347513274415));
#47956=CARTESIAN_POINT('',(58.,-47.2635698398257,-127.523154626899));
#47957=CARTESIAN_POINT('Origin',(72.3260541341291,0.,0.));
#47958=CARTESIAN_POINT('',(58.,-45.764308704547,-128.068841053532));
#47959=CARTESIAN_POINT('Origin',(58.,0.,0.));
#47960=CARTESIAN_POINT('Origin',(72.3260541341288,0.,0.));
#47961=CARTESIAN_POINT('',(57.5,-33.9414761397492,-131.696530696351));
#47962=CARTESIAN_POINT('',(14.5,-33.9414761397492,-131.696530696351));
#47963=CARTESIAN_POINT('',(36.,-33.9414761397492,-131.696530696351));
#47964=CARTESIAN_POINT('',(14.,-34.4282267284513,-131.570122764761));
#47965=CARTESIAN_POINT('Origin',(-0.326054134128837,0.,0.));
#47966=CARTESIAN_POINT('',(14.,-35.9693424282914,-131.157182057546));
#47967=CARTESIAN_POINT('Origin',(14.,0.,0.));
#47968=CARTESIAN_POINT('',(14.5,-36.4540847692092,-131.023279243191));
#47969=CARTESIAN_POINT('Origin',(-0.326054134128855,0.,0.));
#47970=CARTESIAN_POINT('',(57.5,-36.4540847692092,-131.023279243191));
#47971=CARTESIAN_POINT('',(36.,-36.4540847692092,-131.023279243191));
#47972=CARTESIAN_POINT('',(58.,-35.9693424282914,-131.157182057546));
#47973=CARTESIAN_POINT('Origin',(72.3260541341288,0.,0.));
#47974=CARTESIAN_POINT('',(58.,-34.4282267284513,-131.570122764761));
#47975=CARTESIAN_POINT('Origin',(58.,0.,0.));
#47976=CARTESIAN_POINT('Origin',(72.3260541341289,0.,0.));
#47977=CARTESIAN_POINT('',(57.5,-22.3342096256954,-134.153580199693));
#47978=CARTESIAN_POINT('',(14.5,-22.3342096256954,-134.153580199693));
#47979=CARTESIAN_POINT('',(36.,-22.3342096256954,-134.153580199693));
#47980=CARTESIAN_POINT('',(14.,-22.8301251586204,-134.070076397538));
#47981=CARTESIAN_POINT('Origin',(-0.326054134129081,0.,0.));
#47982=CARTESIAN_POINT('',(14.,-24.4013666019952,-133.793024137864));
#47983=CARTESIAN_POINT('Origin',(14.,0.,0.));
#47984=CARTESIAN_POINT('',(14.5,-24.8959347511991,-133.701878942908));
#47985=CARTESIAN_POINT('Origin',(-0.326054134128686,0.,0.));
#47986=CARTESIAN_POINT('',(57.5,-24.8959347511991,-133.701878942908));
#47987=CARTESIAN_POINT('',(36.,-24.8959347511991,-133.701878942908));
#47988=CARTESIAN_POINT('',(58.,-24.4013666019952,-133.793024137864));
#47989=CARTESIAN_POINT('Origin',(72.3260541341286,0.,0.));
#47990=CARTESIAN_POINT('',(58.,-22.8301251586204,-134.070076397538));
#47991=CARTESIAN_POINT('Origin',(58.,0.,0.));
#47992=CARTESIAN_POINT('Origin',(72.326054134129,0.,0.));
#47993=CARTESIAN_POINT('',(57.5,-10.5569662906256,-135.589639953569));
#47994=CARTESIAN_POINT('',(14.5,-10.5569662906256,-135.589639953569));
#47995=CARTESIAN_POINT('',(36.,-10.5569662906256,-135.589639953569));
#47996=CARTESIAN_POINT('',(14.,-11.0582725511258,-135.549675795204));
#47997=CARTESIAN_POINT('Origin',(-0.326054134128864,0.,0.));
#47998=CARTESIAN_POINT('',(14.,-12.6476816419096,-135.410620518056));
#47999=CARTESIAN_POINT('Origin',(14.,0.,0.));
#48000=CARTESIAN_POINT('',(14.5,-13.1483116371559,-135.362926612467));
#48001=CARTESIAN_POINT('Origin',(-0.326054134128744,0.,0.));
#48002=CARTESIAN_POINT('',(57.5,-13.1483116371559,-135.362926612467));
#48003=CARTESIAN_POINT('',(36.,-13.1483116371559,-135.362926612467));
#48004=CARTESIAN_POINT('',(58.,-12.6476816419096,-135.410620518056));
#48005=CARTESIAN_POINT('Origin',(72.3260541341288,0.,0.));
#48006=CARTESIAN_POINT('',(58.,-11.0582725511258,-135.549675795204));
#48007=CARTESIAN_POINT('Origin',(58.,0.,0.));
#48008=CARTESIAN_POINT('Origin',(72.3260541341289,0.,0.));
#48009=CARTESIAN_POINT('',(57.5,1.30062193238638,-135.993780676136));
#48010=CARTESIAN_POINT('',(14.5,1.30062193238638,-135.993780676136));
#48011=CARTESIAN_POINT('',(36.,1.30062193238638,-135.993780676136));
#48012=CARTESIAN_POINT('',(14.,0.797740187650235,-135.997660312937));
#48013=CARTESIAN_POINT('Origin',(-0.326054134128824,0.,0.));
#48014=CARTESIAN_POINT('',(14.,-0.797740187650269,-135.997660312937));
#48015=CARTESIAN_POINT('Origin',(14.,0.,0.));
#48016=CARTESIAN_POINT('',(14.5,-1.30062193238641,-135.993780676136));
#48017=CARTESIAN_POINT('Origin',(-0.326054134128819,0.,0.));
#48018=CARTESIAN_POINT('',(57.5,-1.30062193238641,-135.993780676136));
#48019=CARTESIAN_POINT('',(36.,-1.30062193238641,-135.993780676136));
#48020=CARTESIAN_POINT('',(58.,-0.797740187650269,-135.997660312937));
#48021=CARTESIAN_POINT('Origin',(72.3260541341288,0.,0.));
#48022=CARTESIAN_POINT('',(58.,0.797740187650238,-135.997660312937));
#48023=CARTESIAN_POINT('Origin',(58.,0.,0.));
#48024=CARTESIAN_POINT('Origin',(72.3260541341288,0.,0.));
#48025=CARTESIAN_POINT('',(57.5,13.1483116371559,-135.362926612467));
#48026=CARTESIAN_POINT('',(14.5,13.1483116371559,-135.362926612467));
#48027=CARTESIAN_POINT('',(36.,13.1483116371559,-135.362926612467));
#48028=CARTESIAN_POINT('',(14.,12.6476816419096,-135.410620518056));
#48029=CARTESIAN_POINT('Origin',(-0.32605413412881,0.,0.));
#48030=CARTESIAN_POINT('',(14.,11.0582725511258,-135.549675795204));
#48031=CARTESIAN_POINT('Origin',(14.,0.,0.));
#48032=CARTESIAN_POINT('',(14.5,10.5569662906256,-135.589639953569));
#48033=CARTESIAN_POINT('Origin',(-0.326054134128806,0.,0.));
#48034=CARTESIAN_POINT('',(57.5,10.5569662906256,-135.589639953569));
#48035=CARTESIAN_POINT('',(36.,10.5569662906256,-135.589639953569));
#48036=CARTESIAN_POINT('',(58.,11.0582725511258,-135.549675795204));
#48037=CARTESIAN_POINT('Origin',(72.3260541341287,0.,0.));
#48038=CARTESIAN_POINT('',(58.,12.6476816419096,-135.410620518056));
#48039=CARTESIAN_POINT('Origin',(58.,0.,0.));
#48040=CARTESIAN_POINT('Origin',(72.3260541341288,0.,0.));
#48041=CARTESIAN_POINT('',(57.5,24.895934751199,-133.701878942908));
#48042=CARTESIAN_POINT('',(14.5,24.895934751199,-133.701878942908));
#48043=CARTESIAN_POINT('',(36.,24.895934751199,-133.701878942908));
#48044=CARTESIAN_POINT('',(14.,24.4013666019951,-133.793024137864));
#48045=CARTESIAN_POINT('Origin',(-0.326054134128935,0.,0.));
#48046=CARTESIAN_POINT('',(14.,22.8301251586203,-134.070076397538));
#48047=CARTESIAN_POINT('Origin',(14.,0.,0.));
#48048=CARTESIAN_POINT('',(14.5,22.3342096256953,-134.153580199693));
#48049=CARTESIAN_POINT('Origin',(-0.32605413412921,0.,0.));
#48050=CARTESIAN_POINT('',(57.5,22.3342096256953,-134.153580199693));
#48051=CARTESIAN_POINT('',(36.,22.3342096256953,-134.153580199693));
#48052=CARTESIAN_POINT('',(58.,22.8301251586203,-134.070076397538));
#48053=CARTESIAN_POINT('Origin',(72.326054134129,0.,0.));
#48054=CARTESIAN_POINT('',(58.,24.4013666019951,-133.793024137864));
#48055=CARTESIAN_POINT('Origin',(58.,0.,0.));
#48056=CARTESIAN_POINT('Origin',(72.3260541341287,0.,0.));
#48057=CARTESIAN_POINT('',(57.5,36.4540847692092,-131.023279243191));
#48058=CARTESIAN_POINT('',(14.5,36.4540847692092,-131.023279243191));
#48059=CARTESIAN_POINT('',(36.,36.4540847692092,-131.023279243191));
#48060=CARTESIAN_POINT('',(14.,35.9693424282914,-131.157182057546));
#48061=CARTESIAN_POINT('Origin',(-0.326054134128868,0.,0.));
#48062=CARTESIAN_POINT('',(14.,34.4282267284513,-131.570122764761));
#48063=CARTESIAN_POINT('Origin',(14.,0.,0.));
#48064=CARTESIAN_POINT('',(14.5,33.9414761397492,-131.696530696351));
#48065=CARTESIAN_POINT('Origin',(-0.326054134128984,0.,0.));
#48066=CARTESIAN_POINT('',(57.5,33.9414761397492,-131.696530696351));
#48067=CARTESIAN_POINT('',(36.,33.9414761397492,-131.696530696351));
#48068=CARTESIAN_POINT('',(58.,34.4282267284513,-131.570122764761));
#48069=CARTESIAN_POINT('Origin',(72.3260541341289,0.,0.));
#48070=CARTESIAN_POINT('',(58.,35.9693424282914,-131.157182057546));
#48071=CARTESIAN_POINT('Origin',(58.,0.,0.));
#48072=CARTESIAN_POINT('Origin',(72.3260541341287,0.,0.));
#48073=CARTESIAN_POINT('',(57.5,47.7347971905474,-127.347513274415));
#48074=CARTESIAN_POINT('',(14.5,47.7347971905474,-127.347513274415));
#48075=CARTESIAN_POINT('',(36.,47.7347971905474,-127.347513274415));
#48076=CARTESIAN_POINT('',(14.,47.2635698398257,-127.523154626899));
#48077=CARTESIAN_POINT('Origin',(-0.326054134129454,0.,0.));
#48078=CARTESIAN_POINT('',(14.,45.764308704547,-128.068841053532));
#48079=CARTESIAN_POINT('Origin',(14.,0.,0.));
#48080=CARTESIAN_POINT('',(14.5,45.2904275259558,-128.23719107387));
#48081=CARTESIAN_POINT('Origin',(-0.326054134128611,0.,0.));
#48082=CARTESIAN_POINT('',(57.5,45.2904275259558,-128.23719107387));
#48083=CARTESIAN_POINT('',(36.,45.2904275259558,-128.23719107387));
#48084=CARTESIAN_POINT('',(58.,45.764308704547,-128.068841053532));
#48085=CARTESIAN_POINT('Origin',(72.3260541341288,0.,0.));
#48086=CARTESIAN_POINT('',(58.,47.2635698398257,-127.523154626899));
#48087=CARTESIAN_POINT('Origin',(58.,0.,0.));
#48088=CARTESIAN_POINT('Origin',(72.3260541341294,0.,0.));
#48089=CARTESIAN_POINT('',(57.5,58.652218982207,-122.702555835089));
#48090=CARTESIAN_POINT('',(14.5,58.652218982207,-122.702555835089));
#48091=CARTESIAN_POINT('',(36.,58.652218982207,-122.702555835089));
#48092=CARTESIAN_POINT('',(14.,58.198092946355,-122.918598988955));
#48093=CARTESIAN_POINT('Origin',(-0.326054134128477,0.,0.));
#48094=CARTESIAN_POINT('',(14.,56.752096658156,-123.592878131805));
#48095=CARTESIAN_POINT('Origin',(14.,0.,0.));
#48096=CARTESIAN_POINT('',(14.5,56.2946914115821,-123.801888995583));
#48097=CARTESIAN_POINT('Origin',(-0.326054134128873,0.,0.));
#48098=CARTESIAN_POINT('',(57.5,56.2946914115821,-123.801888995583));
#48099=CARTESIAN_POINT('',(36.,56.2946914115821,-123.801888995583));
#48100=CARTESIAN_POINT('',(58.,56.752096658156,-123.592878131805));
#48101=CARTESIAN_POINT('Origin',(72.3260541341288,0.,0.));
#48102=CARTESIAN_POINT('',(58.,58.198092946355,-122.918598988955));
#48103=CARTESIAN_POINT('Origin',(58.,0.,0.));
#48104=CARTESIAN_POINT('Origin',(72.3260541341284,0.,0.));
#48105=CARTESIAN_POINT('',(57.5,69.1232619722338,-117.12375785603));
#48106=CARTESIAN_POINT('',(14.5,69.1232619722338,-117.12375785603));
#48107=CARTESIAN_POINT('',(36.,69.1232619722338,-117.12375785603));
#48108=CARTESIAN_POINT('',(14.,68.6896934245934,-117.378558592425));
#48109=CARTESIAN_POINT('Origin',(-0.326054134128757,0.,0.));
#48110=CARTESIAN_POINT('',(14.,67.3079668883436,-118.176298780075));
#48111=CARTESIAN_POINT('Origin',(14.,0.,0.));
#48112=CARTESIAN_POINT('',(14.5,66.8705187039021,-118.424379788416));
#48113=CARTESIAN_POINT('Origin',(-0.326054134129086,0.,0.));
#48114=CARTESIAN_POINT('',(57.5,66.8705187039021,-118.424379788416));
#48115=CARTESIAN_POINT('',(36.,66.8705187039021,-118.424379788416));
#48116=CARTESIAN_POINT('',(58.,67.3079668883436,-118.176298780075));
#48117=CARTESIAN_POINT('Origin',(72.326054134129,0.,0.));
#48118=CARTESIAN_POINT('',(58.,68.6896934245934,-117.378558592425));
#48119=CARTESIAN_POINT('Origin',(58.,0.,0.));
#48120=CARTESIAN_POINT('Origin',(72.3260541341287,0.,0.));
#48121=CARTESIAN_POINT('',(57.5,79.0682352008852,-110.653577358427));
#48122=CARTESIAN_POINT('',(14.5,79.0682352008852,-110.653577358427));
#48123=CARTESIAN_POINT('',(36.,79.0682352008852,-110.653577358427));
#48124=CARTESIAN_POINT('',(14.,78.6585238598996,-110.945196489896));
#48125=CARTESIAN_POINT('Origin',(-0.326054134128921,0.,0.));
#48126=CARTESIAN_POINT('',(14.,77.3515828488492,-111.860326437829));
#48127=CARTESIAN_POINT('Origin',(14.,0.,0.));
#48128=CARTESIAN_POINT('',(14.5,76.9374209713624,-112.145589544464));
#48129=CARTESIAN_POINT('Origin',(-0.326054134128895,0.,0.));
#48130=CARTESIAN_POINT('',(57.5,76.9374209713624,-112.145589544464));
#48131=CARTESIAN_POINT('',(36.,76.9374209713624,-112.145589544464));
#48132=CARTESIAN_POINT('',(58.,77.3515828488492,-111.860326437829));
#48133=CARTESIAN_POINT('Origin',(72.3260541341288,0.,0.));
#48134=CARTESIAN_POINT('',(58.,78.6585238598996,-110.945196489896));
#48135=CARTESIAN_POINT('Origin',(58.,0.,0.));
#48136=CARTESIAN_POINT('Origin',(72.3260541341289,0.,0.));
#48137=CARTESIAN_POINT('',(57.5,88.4114514169522,-103.341256322671));
#48138=CARTESIAN_POINT('',(14.5,88.4114514169522,-103.341256322671));
#48139=CARTESIAN_POINT('',(36.,88.4114514169522,-103.341256322671));
#48140=CARTESIAN_POINT('',(14.,88.0287154333169,-103.667474451537));
#48141=CARTESIAN_POINT('Origin',(-0.326054134129112,0.,0.));
#48142=CARTESIAN_POINT('',(14.,86.8065065577125,-104.693029468278));
#48143=CARTESIAN_POINT('Origin',(14.,0.,0.));
#48144=CARTESIAN_POINT('',(14.5,86.4187830091457,-105.01330364872));
#48145=CARTESIAN_POINT('Origin',(-0.326054134129139,0.,0.));
#48146=CARTESIAN_POINT('',(57.5,86.4187830091457,-105.01330364872));
#48147=CARTESIAN_POINT('',(36.,86.4187830091457,-105.01330364872));
#48148=CARTESIAN_POINT('',(58.,86.8065065577126,-104.693029468278));
#48149=CARTESIAN_POINT('Origin',(72.3260541341287,0.,0.));
#48150=CARTESIAN_POINT('',(58.,88.0287154333169,-103.667474451537));
#48151=CARTESIAN_POINT('Origin',(58.,0.,0.));
#48152=CARTESIAN_POINT('Origin',(72.3260541341291,0.,0.));
#48153=CARTESIAN_POINT('',(57.5,97.0818031034422,-95.2424459271415));
#48154=CARTESIAN_POINT('',(14.5,97.0818031034422,-95.2424459271415));
#48155=CARTESIAN_POINT('',(36.,97.0818031034422,-95.2424459271415));
#48156=CARTESIAN_POINT('',(14.,96.7289553290949,-95.6007803364699));
#48157=CARTESIAN_POINT('Origin',(-0.326054134128397,0.,0.));
#48158=CARTESIAN_POINT('',(14.,95.6007803364699,-96.7289553290949));
#48159=CARTESIAN_POINT('Origin',(14.,0.,0.));
#48160=CARTESIAN_POINT('',(14.5,95.2424459271415,-97.0818031034423));
#48161=CARTESIAN_POINT('Origin',(-0.326054134128722,0.,0.));
#48162=CARTESIAN_POINT('',(57.5,95.2424459271415,-97.0818031034423));
#48163=CARTESIAN_POINT('',(36.,95.2424459271415,-97.0818031034423));
#48164=CARTESIAN_POINT('',(58.,95.6007803364699,-96.7289553290949));
#48165=CARTESIAN_POINT('Origin',(72.3260541341287,0.,0.));
#48166=CARTESIAN_POINT('',(58.,96.7289553290949,-95.6007803364699));
#48167=CARTESIAN_POINT('Origin',(58.,0.,0.));
#48168=CARTESIAN_POINT('Origin',(72.3260541341287,0.,0.));
#48169=CARTESIAN_POINT('',(57.5,105.01330364872,-86.4187830091457));
#48170=CARTESIAN_POINT('',(14.5,105.01330364872,-86.4187830091457));
#48171=CARTESIAN_POINT('',(36.,105.01330364872,-86.4187830091457));
#48172=CARTESIAN_POINT('',(14.,104.693029468278,-86.8065065577126));
#48173=CARTESIAN_POINT('Origin',(-0.326054134128375,0.,0.));
#48174=CARTESIAN_POINT('',(14.,103.667474451537,-88.0287154333169));
#48175=CARTESIAN_POINT('Origin',(14.,0.,0.));
#48176=CARTESIAN_POINT('',(14.5,103.34125632267,-88.4114514169522));
#48177=CARTESIAN_POINT('Origin',(-0.326054134128846,0.,0.));
#48178=CARTESIAN_POINT('',(57.5,103.34125632267,-88.4114514169522));
#48179=CARTESIAN_POINT('',(36.,103.34125632267,-88.4114514169522));
#48180=CARTESIAN_POINT('',(58.,103.667474451537,-88.0287154333169));
#48181=CARTESIAN_POINT('Origin',(72.3260541341288,0.,0.));
#48182=CARTESIAN_POINT('',(58.,104.693029468278,-86.8065065577126));
#48183=CARTESIAN_POINT('Origin',(58.,0.,0.));
#48184=CARTESIAN_POINT('Origin',(72.3260541341283,0.,0.));
#48185=CARTESIAN_POINT('',(57.5,112.145589544464,-76.9374209713625));
#48186=CARTESIAN_POINT('',(14.5,112.145589544464,-76.9374209713625));
#48187=CARTESIAN_POINT('',(36.,112.145589544464,-76.9374209713625));
#48188=CARTESIAN_POINT('',(14.,111.860326437829,-77.3515828488493));
#48189=CARTESIAN_POINT('Origin',(-0.32605413412909,0.,0.));
#48190=CARTESIAN_POINT('',(14.,110.945196489896,-78.6585238598997));
#48191=CARTESIAN_POINT('Origin',(14.,0.,0.));
#48192=CARTESIAN_POINT('',(14.5,110.653577358427,-79.0682352008853));
#48193=CARTESIAN_POINT('Origin',(-0.326054134128935,0.,0.));
#48194=CARTESIAN_POINT('',(57.5,110.653577358427,-79.0682352008853));
#48195=CARTESIAN_POINT('',(36.,110.653577358427,-79.0682352008853));
#48196=CARTESIAN_POINT('',(58.,110.945196489896,-78.6585238598997));
#48197=CARTESIAN_POINT('Origin',(72.3260541341289,0.,0.));
#48198=CARTESIAN_POINT('',(58.,111.860326437829,-77.3515828488494));
#48199=CARTESIAN_POINT('Origin',(58.,0.,0.));
#48200=CARTESIAN_POINT('Origin',(72.3260541341286,0.,0.));
#48201=CARTESIAN_POINT('',(57.5,118.424379788416,-66.8705187039023));
#48202=CARTESIAN_POINT('',(14.5,118.424379788416,-66.8705187039023));
#48203=CARTESIAN_POINT('',(36.,118.424379788416,-66.8705187039023));
#48204=CARTESIAN_POINT('',(14.,118.176298780075,-67.3079668883437));
#48205=CARTESIAN_POINT('Origin',(-0.326054134129321,0.,0.));
#48206=CARTESIAN_POINT('',(14.,117.378558592425,-68.6896934245934));
#48207=CARTESIAN_POINT('Origin',(14.,0.,0.));
#48208=CARTESIAN_POINT('',(14.5,117.12375785603,-69.1232619722339));
#48209=CARTESIAN_POINT('Origin',(-0.326054134128744,0.,0.));
#48210=CARTESIAN_POINT('',(57.5,117.12375785603,-69.1232619722339));
#48211=CARTESIAN_POINT('',(36.,117.12375785603,-69.1232619722339));
#48212=CARTESIAN_POINT('',(58.,117.378558592425,-68.6896934245935));
#48213=CARTESIAN_POINT('Origin',(72.3260541341287,0.,0.));
#48214=CARTESIAN_POINT('',(58.,118.176298780075,-67.3079668883437));
#48215=CARTESIAN_POINT('Origin',(58.,0.,0.));
#48216=CARTESIAN_POINT('Origin',(72.3260541341288,0.,0.));
#48217=CARTESIAN_POINT('',(57.5,123.801888995583,-56.2946914115822));
#48218=CARTESIAN_POINT('',(14.5,123.801888995583,-56.2946914115822));
#48219=CARTESIAN_POINT('',(36.,123.801888995583,-56.2946914115822));
#48220=CARTESIAN_POINT('',(14.,123.592878131805,-56.7520966581561));
#48221=CARTESIAN_POINT('Origin',(-0.326054134128881,0.,0.));
#48222=CARTESIAN_POINT('',(14.,122.918598988954,-58.1980929463551));
#48223=CARTESIAN_POINT('Origin',(14.,0.,0.));
#48224=CARTESIAN_POINT('',(14.5,122.702555835089,-58.652218982207));
#48225=CARTESIAN_POINT('Origin',(-0.32605413412873,0.,0.));
#48226=CARTESIAN_POINT('',(57.5,122.702555835089,-58.652218982207));
#48227=CARTESIAN_POINT('',(36.,122.702555835089,-58.652218982207));
#48228=CARTESIAN_POINT('',(58.,122.918598988954,-58.1980929463551));
#48229=CARTESIAN_POINT('Origin',(72.3260541341287,0.,0.));
#48230=CARTESIAN_POINT('',(58.,123.592878131805,-56.7520966581561));
#48231=CARTESIAN_POINT('Origin',(58.,0.,0.));
#48232=CARTESIAN_POINT('Origin',(72.3260541341288,0.,0.));
#48233=CARTESIAN_POINT('',(57.5,128.23719107387,-45.2904275259559));
#48234=CARTESIAN_POINT('',(14.5,128.23719107387,-45.2904275259559));
#48235=CARTESIAN_POINT('',(36.,128.23719107387,-45.2904275259559));
#48236=CARTESIAN_POINT('',(14.,128.068841053532,-45.7643087045471));
#48237=CARTESIAN_POINT('Origin',(-0.326054134128855,0.,0.));
#48238=CARTESIAN_POINT('',(14.,127.523154626899,-47.2635698398257));
#48239=CARTESIAN_POINT('Origin',(14.,0.,0.));
#48240=CARTESIAN_POINT('',(14.5,127.347513274415,-47.7347971905475));
#48241=CARTESIAN_POINT('Origin',(-0.326054134128952,0.,0.));
#48242=CARTESIAN_POINT('',(57.5,127.347513274415,-47.7347971905475));
#48243=CARTESIAN_POINT('',(36.,127.347513274415,-47.7347971905475));
#48244=CARTESIAN_POINT('',(58.,127.523154626899,-47.2635698398257));
#48245=CARTESIAN_POINT('Origin',(72.3260541341289,0.,0.));
#48246=CARTESIAN_POINT('',(58.,128.068841053532,-45.7643087045471));
#48247=CARTESIAN_POINT('Origin',(58.,0.,0.));
#48248=CARTESIAN_POINT('Origin',(72.3260541341288,0.,0.));
#48249=CARTESIAN_POINT('',(57.5,131.696530696351,-33.9414761397491));
#48250=CARTESIAN_POINT('',(14.5,131.696530696351,-33.9414761397491));
#48251=CARTESIAN_POINT('',(36.,131.696530696351,-33.9414761397491));
#48252=CARTESIAN_POINT('',(14.,131.570122764761,-34.4282267284513));
#48253=CARTESIAN_POINT('Origin',(-0.326054134128864,0.,0.));
#48254=CARTESIAN_POINT('',(14.,131.157182057546,-35.9693424282914));
#48255=CARTESIAN_POINT('Origin',(14.,0.,0.));
#48256=CARTESIAN_POINT('',(14.5,131.023279243191,-36.4540847692092));
#48257=CARTESIAN_POINT('Origin',(-0.326054134128739,0.,0.));
#48258=CARTESIAN_POINT('',(57.5,131.023279243191,-36.4540847692092));
#48259=CARTESIAN_POINT('',(36.,131.023279243191,-36.4540847692092));
#48260=CARTESIAN_POINT('',(58.,131.157182057546,-35.9693424282914));
#48261=CARTESIAN_POINT('Origin',(72.3260541341289,0.,0.));
#48262=CARTESIAN_POINT('',(58.,131.570122764761,-34.4282267284513));
#48263=CARTESIAN_POINT('Origin',(58.,0.,0.));
#48264=CARTESIAN_POINT('Origin',(72.3260541341289,0.,0.));
#48265=CARTESIAN_POINT('',(57.5,134.153580199693,-22.3342096256954));
#48266=CARTESIAN_POINT('',(14.5,134.153580199693,-22.3342096256954));
#48267=CARTESIAN_POINT('',(36.,134.153580199693,-22.3342096256954));
#48268=CARTESIAN_POINT('',(14.,134.070076397538,-22.8301251586203));
#48269=CARTESIAN_POINT('Origin',(-0.326054134129072,0.,0.));
#48270=CARTESIAN_POINT('',(14.,133.793024137864,-24.4013666019951));
#48271=CARTESIAN_POINT('Origin',(14.,0.,0.));
#48272=CARTESIAN_POINT('',(14.5,133.701878942908,-24.8959347511991));
#48273=CARTESIAN_POINT('Origin',(-0.326054134128939,0.,0.));
#48274=CARTESIAN_POINT('',(57.5,133.701878942908,-24.8959347511991));
#48275=CARTESIAN_POINT('',(36.,133.701878942908,-24.8959347511991));
#48276=CARTESIAN_POINT('',(58.,133.793024137864,-24.4013666019951));
#48277=CARTESIAN_POINT('Origin',(72.3260541341289,0.,0.));
#48278=CARTESIAN_POINT('',(58.,134.070076397538,-22.8301251586204));
#48279=CARTESIAN_POINT('Origin',(58.,0.,0.));
#48280=CARTESIAN_POINT('Origin',(72.3260541341289,0.,0.));
#48281=CARTESIAN_POINT('',(57.5,135.589639953569,-10.5569662906256));
#48282=CARTESIAN_POINT('',(14.5,135.589639953569,-10.5569662906256));
#48283=CARTESIAN_POINT('',(36.,135.589639953569,-10.5569662906256));
#48284=CARTESIAN_POINT('',(14.,135.549675795204,-11.0582725511259));
#48285=CARTESIAN_POINT('Origin',(-0.32605413412893,0.,0.));
#48286=CARTESIAN_POINT('',(14.,135.410620518056,-12.6476816419096));
#48287=CARTESIAN_POINT('Origin',(14.,0.,0.));
#48288=CARTESIAN_POINT('',(14.5,135.362926612467,-13.1483116371559));
#48289=CARTESIAN_POINT('Origin',(-0.326054134128819,0.,0.));
#48290=CARTESIAN_POINT('',(57.5,135.362926612467,-13.1483116371559));
#48291=CARTESIAN_POINT('',(36.,135.362926612467,-13.1483116371559));
#48292=CARTESIAN_POINT('',(58.,135.410620518056,-12.6476816419096));
#48293=CARTESIAN_POINT('Origin',(72.3260541341288,0.,0.));
#48294=CARTESIAN_POINT('',(58.,135.549675795204,-11.0582725511259));
#48295=CARTESIAN_POINT('Origin',(58.,0.,0.));
#48296=CARTESIAN_POINT('Origin',(72.3260541341289,0.,0.));
#48297=CARTESIAN_POINT('',(57.5,135.993780676136,1.30062193238637));
#48298=CARTESIAN_POINT('',(14.5,135.993780676136,1.30062193238637));
#48299=CARTESIAN_POINT('',(36.,135.993780676136,1.30062193238637));
#48300=CARTESIAN_POINT('',(14.,135.997660312937,0.797740187650231));
#48301=CARTESIAN_POINT('Origin',(-0.326054134128819,0.,0.));
#48302=CARTESIAN_POINT('',(14.,135.997660312937,-0.797740187650278));
#48303=CARTESIAN_POINT('Origin',(14.,0.,0.));
#48304=CARTESIAN_POINT('',(14.5,135.993780676136,-1.30062193238642));
#48305=CARTESIAN_POINT('Origin',(-0.326054134128824,0.,0.));
#48306=CARTESIAN_POINT('',(57.5,135.993780676136,-1.30062193238642));
#48307=CARTESIAN_POINT('',(36.,135.993780676136,-1.30062193238642));
#48308=CARTESIAN_POINT('',(58.,135.997660312937,-0.797740187650278));
#48309=CARTESIAN_POINT('Origin',(72.3260541341288,0.,0.));
#48310=CARTESIAN_POINT('',(58.,135.997660312937,0.797740187650231));
#48311=CARTESIAN_POINT('Origin',(58.,0.,0.));
#48312=CARTESIAN_POINT('Origin',(72.3260541341288,0.,0.));
#48313=CARTESIAN_POINT('',(57.5,135.362926612467,13.1483116371559));
#48314=CARTESIAN_POINT('',(14.5,135.362926612467,13.1483116371559));
#48315=CARTESIAN_POINT('',(36.,135.362926612467,13.1483116371559));
#48316=CARTESIAN_POINT('',(14.,135.410620518056,12.6476816419096));
#48317=CARTESIAN_POINT('Origin',(-0.32605413412881,0.,0.));
#48318=CARTESIAN_POINT('',(14.,135.549675795204,11.0582725511258));
#48319=CARTESIAN_POINT('Origin',(14.,0.,0.));
#48320=CARTESIAN_POINT('',(14.5,135.589639953569,10.5569662906256));
#48321=CARTESIAN_POINT('Origin',(-0.326054134128806,0.,0.));
#48322=CARTESIAN_POINT('',(57.5,135.589639953569,10.5569662906256));
#48323=CARTESIAN_POINT('',(36.,135.589639953569,10.5569662906256));
#48324=CARTESIAN_POINT('',(58.,135.549675795204,11.0582725511258));
#48325=CARTESIAN_POINT('Origin',(72.3260541341288,0.,0.));
#48326=CARTESIAN_POINT('',(58.,135.410620518056,12.6476816419096));
#48327=CARTESIAN_POINT('Origin',(58.,0.,0.));
#48328=CARTESIAN_POINT('Origin',(72.3260541341288,0.,0.));
#48329=CARTESIAN_POINT('',(57.5,133.701878942908,24.895934751199));
#48330=CARTESIAN_POINT('',(14.5,133.701878942908,24.895934751199));
#48331=CARTESIAN_POINT('',(36.,133.701878942908,24.895934751199));
#48332=CARTESIAN_POINT('',(14.,133.793024137864,24.4013666019951));
#48333=CARTESIAN_POINT('Origin',(-0.32605413412893,0.,0.));
#48334=CARTESIAN_POINT('',(14.,134.070076397538,22.8301251586203));
#48335=CARTESIAN_POINT('Origin',(14.,0.,0.));
#48336=CARTESIAN_POINT('',(14.5,134.153580199693,22.3342096256953));
#48337=CARTESIAN_POINT('Origin',(-0.326054134128952,0.,0.));
#48338=CARTESIAN_POINT('',(57.5,134.153580199693,22.3342096256953));
#48339=CARTESIAN_POINT('',(36.,134.153580199693,22.3342096256953));
#48340=CARTESIAN_POINT('',(58.,134.070076397538,22.8301251586203));
#48341=CARTESIAN_POINT('Origin',(72.3260541341289,0.,0.));
#48342=CARTESIAN_POINT('',(58.,133.793024137864,24.4013666019951));
#48343=CARTESIAN_POINT('Origin',(58.,0.,0.));
#48344=CARTESIAN_POINT('Origin',(72.3260541341287,0.,0.));
#48345=CARTESIAN_POINT('',(57.5,131.023279243191,36.4540847692091));
#48346=CARTESIAN_POINT('',(14.5,131.023279243191,36.4540847692091));
#48347=CARTESIAN_POINT('',(36.,131.023279243191,36.4540847692091));
#48348=CARTESIAN_POINT('',(14.,131.157182057546,35.9693424282913));
#48349=CARTESIAN_POINT('Origin',(-0.326054134128735,0.,0.));
#48350=CARTESIAN_POINT('',(14.,131.570122764761,34.4282267284512));
#48351=CARTESIAN_POINT('Origin',(14.,0.,0.));
#48352=CARTESIAN_POINT('',(14.5,131.696530696351,33.9414761397491));
#48353=CARTESIAN_POINT('Origin',(-0.326054134128992,0.,0.));
#48354=CARTESIAN_POINT('',(57.5,131.696530696351,33.9414761397491));
#48355=CARTESIAN_POINT('',(36.,131.696530696351,33.9414761397491));
#48356=CARTESIAN_POINT('',(58.,131.570122764761,34.4282267284512));
#48357=CARTESIAN_POINT('Origin',(72.3260541341289,0.,0.));
#48358=CARTESIAN_POINT('',(58.,131.157182057546,35.9693424282913));
#48359=CARTESIAN_POINT('Origin',(58.,0.,0.));
#48360=CARTESIAN_POINT('Origin',(72.3260541341287,0.,0.));
#48361=CARTESIAN_POINT('',(57.5,127.347513274415,47.7347971905473));
#48362=CARTESIAN_POINT('',(14.5,127.347513274415,47.7347971905473));
#48363=CARTESIAN_POINT('',(36.,127.347513274415,47.7347971905473));
#48364=CARTESIAN_POINT('',(14.,127.523154626899,47.2635698398256));
#48365=CARTESIAN_POINT('Origin',(-0.326054134128948,0.,0.));
#48366=CARTESIAN_POINT('',(14.,128.068841053532,45.7643087045469));
#48367=CARTESIAN_POINT('Origin',(14.,0.,0.));
#48368=CARTESIAN_POINT('',(14.5,128.23719107387,45.2904275259557));
#48369=CARTESIAN_POINT('Origin',(-0.326054134128855,0.,0.));
#48370=CARTESIAN_POINT('',(57.5,128.23719107387,45.2904275259557));
#48371=CARTESIAN_POINT('',(36.,128.23719107387,45.2904275259557));
#48372=CARTESIAN_POINT('',(58.,128.068841053532,45.7643087045469));
#48373=CARTESIAN_POINT('Origin',(72.3260541341288,0.,0.));
#48374=CARTESIAN_POINT('',(58.,127.523154626899,47.2635698398256));
#48375=CARTESIAN_POINT('Origin',(58.,0.,0.));
#48376=CARTESIAN_POINT('Origin',(72.3260541341292,0.,0.));
#48377=CARTESIAN_POINT('',(57.5,122.702555835089,58.6522189822069));
#48378=CARTESIAN_POINT('',(14.5,122.702555835089,58.6522189822069));
#48379=CARTESIAN_POINT('',(36.,122.702555835089,58.6522189822069));
#48380=CARTESIAN_POINT('',(14.,122.918598988955,58.198092946355));
#48381=CARTESIAN_POINT('Origin',(-0.326054134128726,0.,0.));
#48382=CARTESIAN_POINT('',(14.,123.592878131805,56.752096658156));
#48383=CARTESIAN_POINT('Origin',(14.,0.,0.));
#48384=CARTESIAN_POINT('',(14.5,123.801888995583,56.294691411582));
#48385=CARTESIAN_POINT('Origin',(-0.326054134129121,0.,0.));
#48386=CARTESIAN_POINT('',(57.5,123.801888995583,56.294691411582));
#48387=CARTESIAN_POINT('',(36.,123.801888995583,56.294691411582));
#48388=CARTESIAN_POINT('',(58.,123.592878131805,56.752096658156));
#48389=CARTESIAN_POINT('Origin',(72.3260541341291,0.,0.));
#48390=CARTESIAN_POINT('',(58.,122.918598988955,58.198092946355));
#48391=CARTESIAN_POINT('Origin',(58.,0.,0.));
#48392=CARTESIAN_POINT('Origin',(72.3260541341287,0.,0.));
#48393=CARTESIAN_POINT('',(57.5,117.12375785603,69.1232619722339));
#48394=CARTESIAN_POINT('',(14.5,117.12375785603,69.1232619722339));
#48395=CARTESIAN_POINT('',(36.,117.12375785603,69.1232619722339));
#48396=CARTESIAN_POINT('',(14.,117.378558592425,68.6896934245934));
#48397=CARTESIAN_POINT('Origin',(-0.326054134128504,0.,0.));
#48398=CARTESIAN_POINT('',(14.,118.176298780075,67.3079668883437));
#48399=CARTESIAN_POINT('Origin',(14.,0.,0.));
#48400=CARTESIAN_POINT('',(14.5,118.424379788416,66.8705187039022));
#48401=CARTESIAN_POINT('Origin',(-0.326054134128895,0.,0.));
#48402=CARTESIAN_POINT('',(57.5,118.424379788416,66.8705187039022));
#48403=CARTESIAN_POINT('',(36.,118.424379788416,66.8705187039022));
#48404=CARTESIAN_POINT('',(58.,118.176298780075,67.3079668883437));
#48405=CARTESIAN_POINT('Origin',(72.3260541341288,0.,0.));
#48406=CARTESIAN_POINT('',(58.,117.378558592425,68.6896934245934));
#48407=CARTESIAN_POINT('Origin',(58.,0.,0.));
#48408=CARTESIAN_POINT('Origin',(72.3260541341284,0.,0.));
#48409=CARTESIAN_POINT('',(57.5,110.653577358427,79.0682352008853));
#48410=CARTESIAN_POINT('',(14.5,110.653577358427,79.0682352008853));
#48411=CARTESIAN_POINT('',(36.,110.653577358427,79.0682352008853));
#48412=CARTESIAN_POINT('',(14.,110.945196489896,78.6585238598997));
#48413=CARTESIAN_POINT('Origin',(-0.326054134129183,0.,0.));
#48414=CARTESIAN_POINT('',(14.,111.860326437829,77.3515828488493));
#48415=CARTESIAN_POINT('Origin',(14.,0.,0.));
#48416=CARTESIAN_POINT('',(14.5,112.145589544464,76.9374209713625));
#48417=CARTESIAN_POINT('Origin',(-0.326054134128935,0.,0.));
#48418=CARTESIAN_POINT('',(57.5,112.145589544464,76.9374209713625));
#48419=CARTESIAN_POINT('',(36.,112.145589544464,76.9374209713625));
#48420=CARTESIAN_POINT('',(58.,111.860326437829,77.3515828488493));
#48421=CARTESIAN_POINT('Origin',(72.3260541341289,0.,0.));
#48422=CARTESIAN_POINT('',(58.,110.945196489896,78.6585238598997));
#48423=CARTESIAN_POINT('Origin',(58.,0.,0.));
#48424=CARTESIAN_POINT('Origin',(72.3260541341289,0.,0.));
#48425=CARTESIAN_POINT('',(57.5,103.341256322671,88.4114514169522));
#48426=CARTESIAN_POINT('',(14.5,103.341256322671,88.4114514169522));
#48427=CARTESIAN_POINT('',(36.,103.341256322671,88.4114514169522));
#48428=CARTESIAN_POINT('',(14.,103.667474451537,88.0287154333169));
#48429=CARTESIAN_POINT('Origin',(-0.326054134129126,0.,0.));
#48430=CARTESIAN_POINT('',(14.,104.693029468278,86.8065065577125));
#48431=CARTESIAN_POINT('Origin',(14.,0.,0.));
#48432=CARTESIAN_POINT('',(14.5,105.01330364872,86.4187830091457));
#48433=CARTESIAN_POINT('Origin',(-0.32605413412873,0.,0.));
#48434=CARTESIAN_POINT('',(57.5,105.01330364872,86.4187830091457));
#48435=CARTESIAN_POINT('',(36.,105.01330364872,86.4187830091457));
#48436=CARTESIAN_POINT('',(58.,104.693029468278,86.8065065577125));
#48437=CARTESIAN_POINT('Origin',(72.3260541341287,0.,0.));
#48438=CARTESIAN_POINT('',(58.,103.667474451537,88.0287154333169));
#48439=CARTESIAN_POINT('Origin',(58.,0.,0.));
#48440=CARTESIAN_POINT('Origin',(72.3260541341291,0.,0.));
#48441=CARTESIAN_POINT('',(57.5,95.2424459271415,97.0818031034422));
#48442=CARTESIAN_POINT('',(14.5,95.2424459271415,97.0818031034422));
#48443=CARTESIAN_POINT('',(36.,95.2424459271415,97.0818031034422));
#48444=CARTESIAN_POINT('',(14.,95.6007803364699,96.7289553290949));
#48445=CARTESIAN_POINT('Origin',(-0.326054134128722,0.,0.));
#48446=CARTESIAN_POINT('',(14.,96.7289553290949,95.6007803364699));
#48447=CARTESIAN_POINT('Origin',(14.,0.,0.));
#48448=CARTESIAN_POINT('',(14.5,97.0818031034423,95.2424459271415));
#48449=CARTESIAN_POINT('Origin',(-0.326054134128722,0.,0.));
#48450=CARTESIAN_POINT('',(57.5,97.0818031034423,95.2424459271415));
#48451=CARTESIAN_POINT('',(36.,97.0818031034423,95.2424459271415));
#48452=CARTESIAN_POINT('',(58.,96.7289553290949,95.6007803364699));
#48453=CARTESIAN_POINT('Origin',(72.3260541341287,0.,0.));
#48454=CARTESIAN_POINT('',(58.,95.6007803364699,96.7289553290949));
#48455=CARTESIAN_POINT('Origin',(58.,0.,0.));
#48456=CARTESIAN_POINT('Origin',(72.3260541341287,0.,0.));
#48457=CARTESIAN_POINT('',(57.5,86.4187830091458,105.01330364872));
#48458=CARTESIAN_POINT('',(14.5,86.4187830091458,105.01330364872));
#48459=CARTESIAN_POINT('',(36.,86.4187830091458,105.01330364872));
#48460=CARTESIAN_POINT('',(14.,86.8065065577126,104.693029468278));
#48461=CARTESIAN_POINT('Origin',(-0.326054134128388,0.,0.));
#48462=CARTESIAN_POINT('',(14.,88.0287154333169,103.667474451537));
#48463=CARTESIAN_POINT('Origin',(14.,0.,0.));
#48464=CARTESIAN_POINT('',(14.5,88.4114514169523,103.34125632267));
#48465=CARTESIAN_POINT('Origin',(-0.326054134128415,0.,0.));
#48466=CARTESIAN_POINT('',(57.5,88.4114514169523,103.34125632267));
#48467=CARTESIAN_POINT('',(36.,88.4114514169523,103.34125632267));
#48468=CARTESIAN_POINT('',(58.,88.0287154333169,103.667474451537));
#48469=CARTESIAN_POINT('Origin',(72.3260541341291,0.,0.));
#48470=CARTESIAN_POINT('',(58.,86.8065065577126,104.693029468278));
#48471=CARTESIAN_POINT('Origin',(58.,0.,0.));
#48472=CARTESIAN_POINT('Origin',(72.3260541341283,0.,0.));
#48473=CARTESIAN_POINT('',(57.5,76.9374209713625,112.145589544464));
#48474=CARTESIAN_POINT('',(14.5,76.9374209713625,112.145589544464));
#48475=CARTESIAN_POINT('',(36.,76.9374209713625,112.145589544464));
#48476=CARTESIAN_POINT('',(14.,77.3515828488493,111.860326437829));
#48477=CARTESIAN_POINT('Origin',(-0.326054134129108,0.,0.));
#48478=CARTESIAN_POINT('',(14.,78.6585238598997,110.945196489896));
#48479=CARTESIAN_POINT('Origin',(14.,0.,0.));
#48480=CARTESIAN_POINT('',(14.5,79.0682352008854,110.653577358427));
#48481=CARTESIAN_POINT('Origin',(-0.326054134128699,0.,0.));
#48482=CARTESIAN_POINT('',(57.5,79.0682352008854,110.653577358427));
#48483=CARTESIAN_POINT('',(36.,79.0682352008854,110.653577358427));
#48484=CARTESIAN_POINT('',(58.,78.6585238598997,110.945196489896));
#48485=CARTESIAN_POINT('Origin',(72.3260541341286,0.,0.));
#48486=CARTESIAN_POINT('',(58.,77.3515828488494,111.860326437829));
#48487=CARTESIAN_POINT('Origin',(58.,0.,0.));
#48488=CARTESIAN_POINT('Origin',(72.3260541341286,0.,0.));
#48489=CARTESIAN_POINT('',(57.5,66.8705187039023,118.424379788416));
#48490=CARTESIAN_POINT('',(14.5,66.8705187039023,118.424379788416));
#48491=CARTESIAN_POINT('',(36.,66.8705187039023,118.424379788416));
#48492=CARTESIAN_POINT('',(14.,67.3079668883437,118.176298780075));
#48493=CARTESIAN_POINT('Origin',(-0.326054134129325,0.,0.));
#48494=CARTESIAN_POINT('',(14.,68.6896934245934,117.378558592425));
#48495=CARTESIAN_POINT('Origin',(14.,0.,0.));
#48496=CARTESIAN_POINT('',(14.5,69.1232619722339,117.12375785603));
#48497=CARTESIAN_POINT('Origin',(-0.326054134128744,0.,0.));
#48498=CARTESIAN_POINT('',(57.5,69.1232619722339,117.12375785603));
#48499=CARTESIAN_POINT('',(36.,69.1232619722339,117.12375785603));
#48500=CARTESIAN_POINT('',(58.,68.6896934245935,117.378558592425));
#48501=CARTESIAN_POINT('Origin',(72.3260541341287,0.,0.));
#48502=CARTESIAN_POINT('',(58.,67.3079668883437,118.176298780075));
#48503=CARTESIAN_POINT('Origin',(58.,0.,0.));
#48504=CARTESIAN_POINT('Origin',(72.3260541341288,0.,0.));
#48505=CARTESIAN_POINT('',(57.5,56.2946914115822,123.801888995583));
#48506=CARTESIAN_POINT('',(14.5,56.2946914115822,123.801888995583));
#48507=CARTESIAN_POINT('',(36.,56.2946914115822,123.801888995583));
#48508=CARTESIAN_POINT('',(14.,56.7520966581561,123.592878131805));
#48509=CARTESIAN_POINT('Origin',(-0.326054134128895,0.,0.));
#48510=CARTESIAN_POINT('',(14.,58.1980929463551,122.918598988954));
#48511=CARTESIAN_POINT('Origin',(14.,0.,0.));
#48512=CARTESIAN_POINT('',(14.5,58.652218982207,122.702555835089));
#48513=CARTESIAN_POINT('Origin',(-0.326054134128717,0.,0.));
#48514=CARTESIAN_POINT('',(57.5,58.652218982207,122.702555835089));
#48515=CARTESIAN_POINT('',(36.,58.652218982207,122.702555835089));
#48516=CARTESIAN_POINT('',(58.,58.1980929463551,122.918598988954));
#48517=CARTESIAN_POINT('Origin',(72.3260541341287,0.,0.));
#48518=CARTESIAN_POINT('',(58.,56.7520966581561,123.592878131805));
#48519=CARTESIAN_POINT('Origin',(58.,0.,0.));
#48520=CARTESIAN_POINT('Origin',(72.3260541341288,0.,0.));
#48521=CARTESIAN_POINT('',(57.5,45.2904275259559,128.23719107387));
#48522=CARTESIAN_POINT('',(14.5,45.2904275259559,128.23719107387));
#48523=CARTESIAN_POINT('',(36.,45.2904275259559,128.23719107387));
#48524=CARTESIAN_POINT('',(14.,45.7643087045471,128.068841053532));
#48525=CARTESIAN_POINT('Origin',(-0.326054134129072,0.,0.));
#48526=CARTESIAN_POINT('',(14.,47.2635698398257,127.523154626899));
#48527=CARTESIAN_POINT('Origin',(14.,0.,0.));
#48528=CARTESIAN_POINT('',(14.5,47.7347971905475,127.347513274415));
#48529=CARTESIAN_POINT('Origin',(-0.326054134129192,0.,0.));
#48530=CARTESIAN_POINT('',(57.5,47.7347971905475,127.347513274415));
#48531=CARTESIAN_POINT('',(36.,47.7347971905475,127.347513274415));
#48532=CARTESIAN_POINT('',(58.,47.2635698398257,127.523154626899));
#48533=CARTESIAN_POINT('Origin',(72.3260541341288,0.,0.));
#48534=CARTESIAN_POINT('',(58.,45.7643087045471,128.068841053532));
#48535=CARTESIAN_POINT('Origin',(58.,0.,0.));
#48536=CARTESIAN_POINT('Origin',(72.326054134129,0.,0.));
#48537=CARTESIAN_POINT('',(57.5,33.9414761397491,131.696530696351));
#48538=CARTESIAN_POINT('',(14.5,33.9414761397491,131.696530696351));
#48539=CARTESIAN_POINT('',(36.,33.9414761397491,131.696530696351));
#48540=CARTESIAN_POINT('',(14.,34.4282267284513,131.570122764761));
#48541=CARTESIAN_POINT('Origin',(-0.326054134128975,0.,0.));
#48542=CARTESIAN_POINT('',(14.,35.9693424282914,131.157182057546));
#48543=CARTESIAN_POINT('Origin',(14.,0.,0.));
#48544=CARTESIAN_POINT('',(14.5,36.4540847692092,131.023279243191));
#48545=CARTESIAN_POINT('Origin',(-0.326054134128868,0.,0.));
#48546=CARTESIAN_POINT('',(57.5,36.4540847692092,131.023279243191));
#48547=CARTESIAN_POINT('',(36.,36.4540847692092,131.023279243191));
#48548=CARTESIAN_POINT('',(58.,35.9693424282914,131.157182057546));
#48549=CARTESIAN_POINT('Origin',(72.3260541341288,0.,0.));
#48550=CARTESIAN_POINT('',(58.,34.4282267284513,131.570122764761));
#48551=CARTESIAN_POINT('Origin',(58.,0.,0.));
#48552=CARTESIAN_POINT('Origin',(72.3260541341289,0.,0.));
#48553=CARTESIAN_POINT('',(57.5,22.3342096256954,134.153580199693));
#48554=CARTESIAN_POINT('',(14.5,22.3342096256954,134.153580199693));
#48555=CARTESIAN_POINT('',(36.,22.3342096256954,134.153580199693));
#48556=CARTESIAN_POINT('',(14.,22.8301251586204,134.070076397538));
#48557=CARTESIAN_POINT('Origin',(-0.326054134129081,0.,0.));
#48558=CARTESIAN_POINT('',(14.,24.4013666019951,133.793024137864));
#48559=CARTESIAN_POINT('Origin',(14.,0.,0.));
#48560=CARTESIAN_POINT('',(14.5,24.8959347511991,133.701878942908));
#48561=CARTESIAN_POINT('Origin',(-0.326054134128939,0.,0.));
#48562=CARTESIAN_POINT('',(57.5,24.8959347511991,133.701878942908));
#48563=CARTESIAN_POINT('',(36.,24.8959347511991,133.701878942908));
#48564=CARTESIAN_POINT('',(58.,24.4013666019951,133.793024137864));
#48565=CARTESIAN_POINT('Origin',(72.3260541341289,0.,0.));
#48566=CARTESIAN_POINT('',(58.,22.8301251586204,134.070076397538));
#48567=CARTESIAN_POINT('Origin',(58.,0.,0.));
#48568=CARTESIAN_POINT('Origin',(72.3260541341289,0.,0.));
#48569=CARTESIAN_POINT('',(57.5,10.5569662906256,135.589639953569));
#48570=CARTESIAN_POINT('',(14.5,10.5569662906256,135.589639953569));
#48571=CARTESIAN_POINT('',(36.,10.5569662906256,135.589639953569));
#48572=CARTESIAN_POINT('',(14.,11.0582725511259,135.549675795204));
#48573=CARTESIAN_POINT('Origin',(-0.326054134128935,0.,0.));
#48574=CARTESIAN_POINT('',(14.,12.6476816419097,135.410620518056));
#48575=CARTESIAN_POINT('Origin',(14.,0.,0.));
#48576=CARTESIAN_POINT('',(14.5,13.1483116371559,135.362926612467));
#48577=CARTESIAN_POINT('Origin',(-0.32605413412881,0.,0.));
#48578=CARTESIAN_POINT('',(57.5,13.1483116371559,135.362926612467));
#48579=CARTESIAN_POINT('',(36.,13.1483116371559,135.362926612467));
#48580=CARTESIAN_POINT('',(58.,12.6476816419097,135.410620518056));
#48581=CARTESIAN_POINT('Origin',(72.3260541341288,0.,0.));
#48582=CARTESIAN_POINT('',(58.,11.0582725511259,135.549675795204));
#48583=CARTESIAN_POINT('Origin',(58.,0.,0.));
#48584=CARTESIAN_POINT('Origin',(72.3260541341289,0.,0.));
#48585=CARTESIAN_POINT('Origin',(79.75,0.,0.));
#48586=CARTESIAN_POINT('',(80.,-39.531555373985,-33.0076677412016));
#48587=CARTESIAN_POINT('',(80.,-51.3831204224764,3.46769889830224));
#48588=CARTESIAN_POINT('Origin',(80.,0.,0.));
#48589=CARTESIAN_POINT('',(79.5,-51.9213615157264,2.85870921103307));
#48590=CARTESIAN_POINT('Ctrl Pts',(80.,-51.3831204224764,3.46769889830225));
#48591=CARTESIAN_POINT('Ctrl Pts',(79.8355728101073,-51.5617816321932,3.26232634574879));
#48592=CARTESIAN_POINT('Ctrl Pts',(79.6687511538102,-51.7413105700118,3.05929982841873));
#48593=CARTESIAN_POINT('Ctrl Pts',(79.5,-51.9213615157264,2.85870921103307));
#48594=CARTESIAN_POINT('',(79.5,-40.3249567224702,-32.8313549115919));
#48595=CARTESIAN_POINT('Origin',(79.5,0.,0.));
#48596=CARTESIAN_POINT('Ctrl Pts',(80.,-39.5315553739849,-33.0076677412016));
#48597=CARTESIAN_POINT('Ctrl Pts',(79.8355728101073,-39.7968102864981,-32.946532280236));
#48598=CARTESIAN_POINT('Ctrl Pts',(79.6687511538101,-40.0613882408863,-32.8878048394167));
#48599=CARTESIAN_POINT('Ctrl Pts',(79.5,-40.3249567224702,-32.8313549115919));
#48600=CARTESIAN_POINT('Origin',(79.75,-54.352879906268,17.6603212285283));
#48601=CARTESIAN_POINT('',(80.,-43.6080799176108,27.396813060998));
#48602=CARTESIAN_POINT('Origin',(80.,-54.352879906268,17.6603212285283));
#48603=CARTESIAN_POINT('',(79.5,-43.6855709521459,28.205866244188));
#48604=CARTESIAN_POINT('Ctrl Pts',(80.,-43.6080799176108,27.396813060998));
#48605=CARTESIAN_POINT('Ctrl Pts',(79.8355728101073,-43.6319049148906,27.6679773704202));
#48606=CARTESIAN_POINT('Ctrl Pts',(79.6687511538101,-43.6578108838571,27.9377537352586));
#48607=CARTESIAN_POINT('Ctrl Pts',(79.5,-43.6855709521459,28.205866244188));
#48608=CARTESIAN_POINT('Origin',(79.5,-54.352879906268,17.6603212285283));
#48609=CARTESIAN_POINT('Origin',(79.75,0.,0.));
#48610=CARTESIAN_POINT('',(80.,-12.5802798007798,49.9398293963255));
#48611=CARTESIAN_POINT('Origin',(80.,0.,0.));
#48612=CARTESIAN_POINT('',(79.5,-13.3257890560989,50.2635389326334));
#48613=CARTESIAN_POINT('Ctrl Pts',(80.,-12.5802798007798,49.9398293963255));
#48614=CARTESIAN_POINT('Ctrl Pts',(79.8355728101072,-12.8308100551922,50.0462826951187));
#48615=CARTESIAN_POINT('Ctrl Pts',(79.6687511538099,-13.0793772402478,50.1542862171309));
#48616=CARTESIAN_POINT('Ctrl Pts',(79.5,-13.3257890560989,50.2635389326334));
#48617=CARTESIAN_POINT('Origin',(79.5,0.,0.));
#48618=CARTESIAN_POINT('Origin',(79.75,3.49942822856356E-15,57.15));
#48619=CARTESIAN_POINT('',(80.,12.5802798007798,49.9398293963255));
#48620=CARTESIAN_POINT('Origin',(80.,3.49942822856356E-15,57.15));
#48621=CARTESIAN_POINT('',(79.5,13.3257890560989,50.2635389326334));
#48622=CARTESIAN_POINT('Ctrl Pts',(80.,12.5802798007798,49.9398293963255));
#48623=CARTESIAN_POINT('Ctrl Pts',(79.8355728101074,12.8308100551919,50.0462826951186));
#48624=CARTESIAN_POINT('Ctrl Pts',(79.6687511538103,13.0793772402473,50.1542862171307));
#48625=CARTESIAN_POINT('Ctrl Pts',(79.5,13.3257890560989,50.2635389326334));
#48626=CARTESIAN_POINT('Origin',(79.5,3.49942822856356E-15,57.15));
#48627=CARTESIAN_POINT('Origin',(79.75,0.,0.));
#48628=CARTESIAN_POINT('',(80.,43.6080799176108,27.396813060998));
#48629=CARTESIAN_POINT('Origin',(80.,0.,0.));
#48630=CARTESIAN_POINT('',(79.5,43.6855709521459,28.205866244188));
#48631=CARTESIAN_POINT('Ctrl Pts',(80.,43.6080799176108,27.396813060998));
#48632=CARTESIAN_POINT('Ctrl Pts',(79.8355728101071,43.6319049148907,27.6679773704205));
#48633=CARTESIAN_POINT('Ctrl Pts',(79.6687511538098,43.6578108838571,27.9377537352591));
#48634=CARTESIAN_POINT('Ctrl Pts',(79.5,43.6855709521459,28.205866244188));
#48635=CARTESIAN_POINT('Origin',(79.5,0.,0.));
#48636=CARTESIAN_POINT('Origin',(79.75,54.352879906268,17.6603212285282));
#48637=CARTESIAN_POINT('',(80.,51.3831204224764,3.46769889830222));
#48638=CARTESIAN_POINT('Origin',(80.,54.352879906268,17.6603212285282));
#48639=CARTESIAN_POINT('',(79.5,51.9213615157264,2.85870921103304));
#48640=CARTESIAN_POINT('Ctrl Pts',(80.,51.3831204224764,3.46769889830223));
#48641=CARTESIAN_POINT('Ctrl Pts',(79.8355728101072,51.5617816321933,3.26232634574865));
#48642=CARTESIAN_POINT('Ctrl Pts',(79.66875115381,51.741310570012,3.05929982841845));
#48643=CARTESIAN_POINT('Ctrl Pts',(79.5,51.9213615157264,2.85870921103305));
#48644=CARTESIAN_POINT('Origin',(79.5,54.352879906268,17.6603212285282));
#48645=CARTESIAN_POINT('Origin',(79.75,0.,0.));
#48646=CARTESIAN_POINT('',(79.5,40.3249567224702,-32.8313549115919));
#48647=CARTESIAN_POINT('Origin',(79.5,0.,0.));
#48648=CARTESIAN_POINT('',(80.,39.5315553739849,-33.0076677412016));
#48649=CARTESIAN_POINT('Origin',(80.,0.,0.));
#48650=CARTESIAN_POINT('Ctrl Pts',(80.,39.5315553739849,-33.0076677412016));
#48651=CARTESIAN_POINT('Ctrl Pts',(79.8355728101073,39.796810286498,-32.946532280236));
#48652=CARTESIAN_POINT('Ctrl Pts',(79.6687511538102,40.0613882408862,-32.8878048394167));
#48653=CARTESIAN_POINT('Ctrl Pts',(79.5,40.3249567224702,-32.8313549115919));
#48654=CARTESIAN_POINT('Origin',(79.75,33.5919271685148,-46.2353212285282));
#48655=CARTESIAN_POINT('',(79.5,18.7633771027908,-48.4967594762626));
#48656=CARTESIAN_POINT('Origin',(79.5,33.5919271685148,-46.2353212285282));
#48657=CARTESIAN_POINT('',(80.,19.1762350683395,-47.7966736144241));
#48658=CARTESIAN_POINT('Origin',(80.,33.5919271685148,-46.2353212285282));
#48659=CARTESIAN_POINT('Ctrl Pts',(80.,19.1762350683395,-47.7966736144241));
#48660=CARTESIAN_POINT('Ctrl Pts',(79.8355728101073,19.0361235140034,-48.0300541310517));
#48661=CARTESIAN_POINT('Ctrl Pts',(79.6687511538101,18.8985113144839,-48.2635349413914));
#48662=CARTESIAN_POINT('Ctrl Pts',(79.5,18.7633771027908,-48.4967594762626));
#48663=CARTESIAN_POINT('Origin',(79.75,0.,0.));
#48664=CARTESIAN_POINT('',(79.5,-18.7633771027908,-48.4967594762626));
#48665=CARTESIAN_POINT('Origin',(79.5,0.,0.));
#48666=CARTESIAN_POINT('',(80.,-19.1762350683395,-47.7966736144241));
#48667=CARTESIAN_POINT('Origin',(80.,0.,0.));
#48668=CARTESIAN_POINT('Ctrl Pts',(80.,-19.1762350683395,-47.7966736144241));
#48669=CARTESIAN_POINT('Ctrl Pts',(79.8355728101073,-19.0361235140034,-48.0300541310517));
#48670=CARTESIAN_POINT('Ctrl Pts',(79.66875115381,-18.8985113144839,-48.2635349413915));
#48671=CARTESIAN_POINT('Ctrl Pts',(79.5,-18.7633771027908,-48.4967594762626));
#48672=CARTESIAN_POINT('Origin',(79.75,-33.5919271685148,-46.2353212285282));
#48673=CARTESIAN_POINT('Origin',(79.5,-33.5919271685148,-46.2353212285282));
#48674=CARTESIAN_POINT('Origin',(80.,-33.5919271685148,-46.2353212285282));
#48675=CARTESIAN_POINT('Origin',(72.,54.352879906268,17.6603212285282));
#48676=CARTESIAN_POINT('',(72.,51.9213615157264,2.85870921103304));
#48677=CARTESIAN_POINT('',(72.,51.9213615157264,2.85870921103304));
#48678=CARTESIAN_POINT('',(72.,43.6855709521459,28.205866244188));
#48679=CARTESIAN_POINT('Origin',(72.,54.352879906268,17.6603212285282));
#48680=CARTESIAN_POINT('',(72.,43.6855709521459,28.205866244188));
#48681=CARTESIAN_POINT('Origin',(72.,0.,0.));
#48682=CARTESIAN_POINT('',(72.,40.3249567224702,-32.8313549115919));
#48683=CARTESIAN_POINT('',(72.,40.3249567224702,-32.8313549115919));
#48684=CARTESIAN_POINT('Origin',(72.,0.,0.));
#48685=CARTESIAN_POINT('Origin',(72.,33.5919271685148,-46.2353212285282));
#48686=CARTESIAN_POINT('',(72.,18.7633771027908,-48.4967594762626));
#48687=CARTESIAN_POINT('',(72.,18.7633771027908,-48.4967594762626));
#48688=CARTESIAN_POINT('Origin',(72.,33.5919271685148,-46.2353212285282));
#48689=CARTESIAN_POINT('Origin',(72.,0.,0.));
#48690=CARTESIAN_POINT('',(72.,-18.7633771027908,-48.4967594762626));
#48691=CARTESIAN_POINT('',(72.,-18.7633771027908,-48.4967594762626));
#48692=CARTESIAN_POINT('Origin',(72.,0.,0.));
#48693=CARTESIAN_POINT('Origin',(72.,-33.5919271685148,-46.2353212285282));
#48694=CARTESIAN_POINT('',(72.,-40.3249567224702,-32.8313549115919));
#48695=CARTESIAN_POINT('',(72.,-40.3249567224702,-32.8313549115919));
#48696=CARTESIAN_POINT('Origin',(72.,-33.5919271685148,-46.2353212285282));
#48697=CARTESIAN_POINT('Origin',(72.,0.,0.));
#48698=CARTESIAN_POINT('',(72.,-51.9213615157264,2.85870921103307));
#48699=CARTESIAN_POINT('',(72.,-51.9213615157264,2.85870921103307));
#48700=CARTESIAN_POINT('Origin',(72.,0.,0.));
#48701=CARTESIAN_POINT('Origin',(80.,0.,5.45733938573587));
#48702=CARTESIAN_POINT('',(80.,33.5919271685148,-39.0553212285282));
#48703=CARTESIAN_POINT('Origin',(80.,33.5919271685148,-46.2353212285282));
#48704=CARTESIAN_POINT('',(80.,-33.5919271685148,-39.0553212285282));
#48705=CARTESIAN_POINT('Origin',(80.,-33.5919271685148,-46.2353212285282));
#48706=CARTESIAN_POINT('',(80.,-54.352879906268,24.8403212285282));
#48707=CARTESIAN_POINT('Origin',(80.,-54.352879906268,17.6603212285283));
#48708=CARTESIAN_POINT('',(80.,2.62013182677576E-15,64.33));
#48709=CARTESIAN_POINT('Origin',(80.,3.49942822856356E-15,57.15));
#48710=CARTESIAN_POINT('',(80.,54.352879906268,24.8403212285282));
#48711=CARTESIAN_POINT('Origin',(80.,54.352879906268,17.6603212285282));
#48712=CARTESIAN_POINT('Origin',(57.75,1.0453001083881,136.034530010839));
#48713=CARTESIAN_POINT('',(57.7487592975525,0.77487592975525,138.751240702447));
#48714=CARTESIAN_POINT('',(58.,0.547506218943957,138.5));
#48715=CARTESIAN_POINT('',(58.2319907935076,0.337557436295053,138.268009206492));
#48716=CARTESIAN_POINT('',(58.,0.7965408108356,136.009654081084));
#48717=CARTESIAN_POINT('',(57.5,1.0497518595105,138.502481404895));
#48718=CARTESIAN_POINT('',(57.5,1.29405940594059,136.059405940594));
#48719=CARTESIAN_POINT('',(50.4896657310026,8.79608403300078,131.492147135898));
#48720=CARTESIAN_POINT('Origin',(58.,0.,137.));
#48721=CARTESIAN_POINT('',(58.,-0.547506218943957,138.5));
#48722=CARTESIAN_POINT('',(58.,0.5,138.5));
#48723=CARTESIAN_POINT('',(58.,-0.596540810835601,138.009654081084));
#48724=CARTESIAN_POINT('Origin',(57.75,0.5,138.75));
#48725=CARTESIAN_POINT('',(57.5,0.499999999999999,139.));
#48726=CARTESIAN_POINT('',(57.5,0.499999999999999,139.));
#48727=CARTESIAN_POINT('',(57.5,-0.500000000000002,139.));
#48728=CARTESIAN_POINT('',(57.5,0.5,139.));
#48729=CARTESIAN_POINT('',(57.5,-0.500000000000002,139.));
#48730=CARTESIAN_POINT('Origin',(14.,0.774875929755249,138.751240702448));
#48731=CARTESIAN_POINT('',(14.5,1.0497518595105,138.502481404895));
#48732=CARTESIAN_POINT('',(14.,1.0497518595105,138.502481404895));
#48733=CARTESIAN_POINT('',(14.5,0.499999999999999,139.));
#48734=CARTESIAN_POINT('',(14.5,1.0497518595105,138.502481404895));
#48735=CARTESIAN_POINT('',(14.,0.499999999999999,139.));
#48736=CARTESIAN_POINT('Origin',(57.5,-1.0497518595105,138.502481404895));
#48737=CARTESIAN_POINT('',(57.5,-1.0497518595105,138.502481404895));
#48738=CARTESIAN_POINT('',(57.5,-1.0497518595105,138.502481404895));
#48739=CARTESIAN_POINT('',(58.,-0.547506218943957,138.5));
#48740=CARTESIAN_POINT('Origin',(14.,0.547506218943958,138.5));
#48741=CARTESIAN_POINT('',(14.,0.547506218943958,138.5));
#48742=CARTESIAN_POINT('',(14.,0.547506218943958,138.5));
#48743=CARTESIAN_POINT('',(14.5,0.499999999999999,139.));
#48744=CARTESIAN_POINT('Origin',(14.25,1.0453001083881,136.034530010839));
#48745=CARTESIAN_POINT('',(14.,0.7965408108356,136.009654081084));
#48746=CARTESIAN_POINT('',(14.5,1.29405940594059,136.059405940594));
#48747=CARTESIAN_POINT('Origin',(14.5,-1.0497518595105,138.502481404895));
#48748=CARTESIAN_POINT('',(14.,-0.547506218943957,138.5));
#48749=CARTESIAN_POINT('',(14.5,-0.500000000000002,139.));
#48750=CARTESIAN_POINT('',(14.,-0.547506218943957,138.5));
#48751=CARTESIAN_POINT('',(14.5,-1.0497518595105,138.502481404895));
#48752=CARTESIAN_POINT('',(14.5,-1.0497518595105,138.502481404895));
#48753=CARTESIAN_POINT('',(14.5,-0.500000000000002,139.));
#48754=CARTESIAN_POINT('Origin',(14.25,-0.845300108388097,138.034530010839));
#48755=CARTESIAN_POINT('',(14.5,-1.09405940594059,138.059405940594));
#48756=CARTESIAN_POINT('',(14.,-0.5965408108356,138.009654081084));
#48757=CARTESIAN_POINT('Origin',(14.,-0.774875929755251,138.751240702447));
#48758=CARTESIAN_POINT('',(14.,-0.500000000000002,139.));
#48759=CARTESIAN_POINT('',(14.,-1.0497518595105,138.502481404895));
#48760=CARTESIAN_POINT('Origin',(14.25,0.5,138.75));
#48761=CARTESIAN_POINT('',(14.5,0.5,139.));
#48762=CARTESIAN_POINT('',(14.,0.5,138.5));
#48763=CARTESIAN_POINT('Origin',(57.75,-0.845300108388097,138.034530010839));
#48764=CARTESIAN_POINT('',(57.5,-1.09405940594059,138.059405940594));
#48765=CARTESIAN_POINT('Origin',(14.,1.4,135.));
#48766=CARTESIAN_POINT('Origin',(14.,1.,139.));
#48767=CARTESIAN_POINT('Origin',(57.5,-11.6165508928786,138.514640906126));
#48768=CARTESIAN_POINT('',(57.5,-11.025529402481,138.066929551123));
#48769=CARTESIAN_POINT('',(58.,-11.5256475780664,138.020683996878));
#48770=CARTESIAN_POINT('',(57.5,-11.025529402481,138.066929551123));
#48771=CARTESIAN_POINT('',(57.5,-11.6165508928786,138.514640906126));
#48772=CARTESIAN_POINT('',(57.5,-11.6165508928786,138.514640906126));
#48773=CARTESIAN_POINT('',(58.,-11.5256475780664,138.020683996878));
#48774=CARTESIAN_POINT('Origin',(57.5,-13.1170438759936,137.883945745091));
#48775=CARTESIAN_POINT('',(57.5,-12.6127455909704,138.427485163379));
#48776=CARTESIAN_POINT('',(58.,-12.6164931630349,137.925247374536));
#48777=CARTESIAN_POINT('',(57.5,-12.6127455909704,138.427485163379));
#48778=CARTESIAN_POINT('',(57.5,-13.1170438759936,137.883945745091));
#48779=CARTESIAN_POINT('',(57.5,-13.1170438759936,137.883945745091));
#48780=CARTESIAN_POINT('',(58.,-12.6164931630349,137.925247374536));
#48781=CARTESIAN_POINT('Origin',(14.,-11.5256475780664,138.020683996878));
#48782=CARTESIAN_POINT('',(14.5,-11.025529402481,138.066929551123));
#48783=CARTESIAN_POINT('',(14.5,-11.6165508928786,138.514640906126));
#48784=CARTESIAN_POINT('',(14.5,-11.025529402481,138.066929551123));
#48785=CARTESIAN_POINT('',(14.,-11.5256475780664,138.020683996878));
#48786=CARTESIAN_POINT('',(14.,-11.5256475780664,138.020683996878));
#48787=CARTESIAN_POINT('',(14.5,-11.6165508928786,138.514640906126));
#48788=CARTESIAN_POINT('Origin',(14.25,-10.8148680765323,135.607981461541));
#48789=CARTESIAN_POINT('',(14.,-11.0605126897208,135.561519390865));
#48790=CARTESIAN_POINT('',(14.5,-10.5692234633438,135.654443532217));
#48791=CARTESIAN_POINT('Origin',(14.5,-13.1170438759936,137.883945745091));
#48792=CARTESIAN_POINT('',(14.,-12.6164931630349,137.925247374536));
#48793=CARTESIAN_POINT('',(14.5,-12.6127455909704,138.427485163379));
#48794=CARTESIAN_POINT('',(14.,-12.6164931630349,137.925247374536));
#48795=CARTESIAN_POINT('',(14.5,-13.1170438759936,137.883945745091));
#48796=CARTESIAN_POINT('',(14.5,-13.1170438759936,137.883945745091));
#48797=CARTESIAN_POINT('',(14.5,-12.6127455909704,138.427485163379));
#48798=CARTESIAN_POINT('Origin',(14.25,-12.8725854741912,137.435594191592));
#48799=CARTESIAN_POINT('',(14.5,-13.1225662476484,137.438694659581));
#48800=CARTESIAN_POINT('',(14.,-12.622604700734,137.432493723604));
#48801=CARTESIAN_POINT('Origin',(14.,-12.864894733482,138.155715454235));
#48802=CARTESIAN_POINT('',(14.,-12.6127455909704,138.427485163379));
#48803=CARTESIAN_POINT('',(14.,-13.1170438759936,137.883945745091));
#48804=CARTESIAN_POINT('Origin',(14.25,-11.5947619571917,138.265592231604));
#48805=CARTESIAN_POINT('',(14.5,-11.6165508928786,138.514640906126));
#48806=CARTESIAN_POINT('',(14.,-11.5729730215048,138.016543557081));
#48807=CARTESIAN_POINT('Origin',(14.,-11.3210401476798,138.290785228625));
#48808=CARTESIAN_POINT('',(14.,-11.025529402481,138.066929551123));
#48809=CARTESIAN_POINT('',(14.,-11.6165508928786,138.514640906126));
#48810=CARTESIAN_POINT('Origin',(57.75,-12.8725854741912,137.435594191592));
#48811=CARTESIAN_POINT('',(58.,-12.622604700734,137.432493723604));
#48812=CARTESIAN_POINT('',(57.5,-13.1225662476484,137.438694659581));
#48813=CARTESIAN_POINT('Origin',(57.75,-11.5947619571917,138.265592231604));
#48814=CARTESIAN_POINT('',(58.,-11.5729730215048,138.016543557081));
#48815=CARTESIAN_POINT('',(57.5,-11.6165508928786,138.514640906126));
#48816=CARTESIAN_POINT('Origin',(57.75,-10.8148680765323,135.607981461541));
#48817=CARTESIAN_POINT('',(57.5,-10.5692234633438,135.654443532217));
#48818=CARTESIAN_POINT('',(58.,-11.0605126897208,135.561519390865));
#48819=CARTESIAN_POINT('Origin',(14.,-11.9403367564292,136.478673638569));
#48820=CARTESIAN_POINT('Origin',(14.,-10.3713526936054,134.608302282232));
#48821=CARTESIAN_POINT('Origin',(14.,-11.1184535438327,138.5582187775));
#48822=CARTESIAN_POINT('Origin',(57.5,-25.0845072682928,136.216030001563));
#48823=CARTESIAN_POINT('',(57.5,-24.6295005722094,136.801453579863));
#48824=CARTESIAN_POINT('',(58.,-24.5894609761083,136.30080033501));
#48825=CARTESIAN_POINT('',(57.5,-24.6295005722094,136.801453579863));
#48826=CARTESIAN_POINT('',(57.5,-25.0845072682928,136.216030001563));
#48827=CARTESIAN_POINT('',(57.5,-25.0845072682928,136.216030001563));
#48828=CARTESIAN_POINT('',(58.,-24.5894609761083,136.30080033501));
#48829=CARTESIAN_POINT('Origin',(14.,-24.8570039202511,136.508741790713));
#48830=CARTESIAN_POINT('',(14.2512407024475,-24.8570039202511,136.508741790713));
#48831=CARTESIAN_POINT('',(14.5,-25.0845072682928,136.216030001563));
#48832=CARTESIAN_POINT('',(14.3353834448874,-24.9339568454557,136.409732133885));
#48833=CARTESIAN_POINT('',(14.,-25.0845072682928,136.216030001563));
#48834=CARTESIAN_POINT('',(14.5,-24.6295005722094,136.801453579863));
#48835=CARTESIAN_POINT('',(14.,-24.6295005722094,136.801453579863));
#48836=CARTESIAN_POINT('',(14.4305329766294,-24.693031787126,136.719712648378));
#48837=CARTESIAN_POINT('Origin',(57.75,-24.801902691856,135.790690514667));
#48838=CARTESIAN_POINT('',(58.,-24.5526029471227,135.809389104878));
#48839=CARTESIAN_POINT('',(57.5,-25.0512024365894,135.771991924456));
#48840=CARTESIAN_POINT('Origin',(57.5,-23.6446928191972,136.97510175753));
#48841=CARTESIAN_POINT('',(57.5,-23.016899728323,136.580604996376));
#48842=CARTESIAN_POINT('',(58.,-23.5110842376314,136.490947249372));
#48843=CARTESIAN_POINT('',(57.5,-23.016899728323,136.580604996376));
#48844=CARTESIAN_POINT('',(57.5,-23.6446928191972,136.97510175753));
#48845=CARTESIAN_POINT('',(57.5,-23.6446928191972,136.97510175753));
#48846=CARTESIAN_POINT('',(58.,-23.5110842376314,136.490947249372));
#48847=CARTESIAN_POINT('Origin',(14.,-23.3307962737601,136.777853376953));
#48848=CARTESIAN_POINT('',(14.2512407024475,-23.3307962737601,136.777853376953));
#48849=CARTESIAN_POINT('',(14.5,-23.6446928191972,136.97510175753));
#48850=CARTESIAN_POINT('',(14.2590041943422,-23.3405926243297,136.784009272306));
#48851=CARTESIAN_POINT('',(14.,-23.6446928191972,136.97510175753));
#48852=CARTESIAN_POINT('',(14.5,-23.016899728323,136.580604996376));
#48853=CARTESIAN_POINT('',(14.,-23.016899728323,136.580604996376));
#48854=CARTESIAN_POINT('',(14.6801520303733,-22.7895751597781,136.437757285362));
#48855=CARTESIAN_POINT('Origin',(57.75,-23.6012807747805,136.728899819277));
#48856=CARTESIAN_POINT('',(58.,-23.5578687303638,136.482697881024));
#48857=CARTESIAN_POINT('',(57.5,-23.6446928191972,136.97510175753));
#48858=CARTESIAN_POINT('Origin',(57.75,-22.5927285851944,134.149374290983));
#48859=CARTESIAN_POINT('',(57.5,-22.3520681602006,134.217068898167));
#48860=CARTESIAN_POINT('',(58.,-22.8333890101882,134.081679683799));
#48861=CARTESIAN_POINT('Origin',(14.25,-24.801902691856,135.790690514667));
#48862=CARTESIAN_POINT('',(14.,-24.5894609761083,136.30080033501));
#48863=CARTESIAN_POINT('',(14.5,-25.1219044487155,136.71462949103));
#48864=CARTESIAN_POINT('',(14.,-24.5526029471227,135.809389104878));
#48865=CARTESIAN_POINT('',(14.5,-25.0512024365894,135.771991924456));
#48866=CARTESIAN_POINT('Origin',(14.,-23.1522889426911,137.061925846364));
#48867=CARTESIAN_POINT('',(14.5,-23.6446928191972,136.97510175753));
#48868=CARTESIAN_POINT('Origin',(14.25,-23.6012807747805,136.728899819277));
#48869=CARTESIAN_POINT('',(14.,-23.5110842376314,136.490947249372));
#48870=CARTESIAN_POINT('',(14.,-23.5110842376314,136.490947249372));
#48871=CARTESIAN_POINT('',(14.,-23.5578687303638,136.482697881024));
#48872=CARTESIAN_POINT('Origin',(14.25,-22.5927285851944,134.149374290983));
#48873=CARTESIAN_POINT('',(14.5,-22.3520681602006,134.217068898167));
#48874=CARTESIAN_POINT('',(14.,-22.8333890101882,134.081679683799));
#48875=CARTESIAN_POINT('Origin',(14.,-22.0637731308185,133.192154105382));
#48876=CARTESIAN_POINT('Origin',(14.,-25.1219044487155,136.71462949103));
#48877=CARTESIAN_POINT('Origin',(57.5,-35.4928843561059,134.393099376732));
#48878=CARTESIAN_POINT('',(57.5,-34.8330975492484,134.054819567983));
#48879=CARTESIAN_POINT('',(58.,-35.3175873497673,133.922431977811));
#48880=CARTESIAN_POINT('',(57.5,-34.8330975492484,134.054819567983));
#48881=CARTESIAN_POINT('',(57.5,-35.4928843561059,134.393099376732));
#48882=CARTESIAN_POINT('',(57.5,-35.4928843561059,134.393099376732));
#48883=CARTESIAN_POINT('',(58.,-35.3175873497673,133.922431977811));
#48884=CARTESIAN_POINT('Origin',(57.5,-36.8610624138407,133.511428020236));
#48885=CARTESIAN_POINT('',(57.5,-36.4588101823949,134.134280331629));
#48886=CARTESIAN_POINT('',(58.,-36.375288143631,133.639021904261));
#48887=CARTESIAN_POINT('',(57.5,-36.4588101823949,134.134280331629));
#48888=CARTESIAN_POINT('',(57.5,-36.8610624138407,133.511428020236));
#48889=CARTESIAN_POINT('',(57.5,-36.8610624138407,133.511428020236));
#48890=CARTESIAN_POINT('',(58.,-36.375288143631,133.639021904261));
#48891=CARTESIAN_POINT('Origin',(14.,-35.3175873497673,133.922431977811));
#48892=CARTESIAN_POINT('',(14.5,-34.8330975492484,134.054819567983));
#48893=CARTESIAN_POINT('',(14.5,-35.4928843561059,134.393099376732));
#48894=CARTESIAN_POINT('',(14.5,-34.8330975492484,134.054819567983));
#48895=CARTESIAN_POINT('',(14.,-35.3175873497673,133.922431977811));
#48896=CARTESIAN_POINT('',(14.,-35.3175873497673,133.922431977811));
#48897=CARTESIAN_POINT('',(14.5,-35.4928843561059,134.393099376732));
#48898=CARTESIAN_POINT('Origin',(14.25,-34.1986447874607,131.669809380463));
#48899=CARTESIAN_POINT('',(14.,-34.4324894531109,131.581397433607));
#48900=CARTESIAN_POINT('',(14.5,-33.9648001218105,131.75822132732));
#48901=CARTESIAN_POINT('Origin',(14.5,-36.8610624138407,133.511428020236));
#48902=CARTESIAN_POINT('',(14.,-36.375288143631,133.639021904261));
#48903=CARTESIAN_POINT('',(14.5,-36.4588101823949,134.134280331629));
#48904=CARTESIAN_POINT('',(14.,-36.375288143631,133.639021904261));
#48905=CARTESIAN_POINT('',(14.5,-36.8610624138407,133.511428020236));
#48906=CARTESIAN_POINT('',(14.5,-36.8610624138407,133.511428020236));
#48907=CARTESIAN_POINT('',(14.5,-36.4588101823949,134.134280331629));
#48908=CARTESIAN_POINT('Origin',(14.25,-36.5424624542376,133.112337690265));
#48909=CARTESIAN_POINT('',(14.5,-36.7891838486583,133.071982349415));
#48910=CARTESIAN_POINT('',(14.,-36.2957410598168,133.152693031114));
#48911=CARTESIAN_POINT('Origin',(14.,-36.6599362981178,133.822854175933));
#48912=CARTESIAN_POINT('',(14.,-36.4588101823949,134.134280331629));
#48913=CARTESIAN_POINT('',(14.,-36.8610624138407,133.511428020236));
#48914=CARTESIAN_POINT('Origin',(14.25,-35.4281795948302,134.151617920159));
#48915=CARTESIAN_POINT('',(14.5,-35.4928843561059,134.393099376732));
#48916=CARTESIAN_POINT('',(14.,-35.3634748335546,133.910136463587));
#48917=CARTESIAN_POINT('Origin',(14.,-35.1629909526771,134.223959472357));
#48918=CARTESIAN_POINT('',(14.,-34.8330975492484,134.054819567983));
#48919=CARTESIAN_POINT('',(14.,-35.4928843561059,134.393099376732));
#48920=CARTESIAN_POINT('Origin',(57.75,-36.5424624542376,133.112337690265));
#48921=CARTESIAN_POINT('',(58.,-36.2957410598168,133.152693031114));
#48922=CARTESIAN_POINT('',(57.5,-36.7891838486583,133.071982349415));
#48923=CARTESIAN_POINT('Origin',(57.75,-35.4281795948302,134.151617920159));
#48924=CARTESIAN_POINT('',(58.,-35.3634748335546,133.910136463587));
#48925=CARTESIAN_POINT('',(57.5,-35.4928843561059,134.393099376732));
#48926=CARTESIAN_POINT('Origin',(57.75,-34.1986447874607,131.669809380463));
#48927=CARTESIAN_POINT('',(57.5,-33.9648001218105,131.75822132732));
#48928=CARTESIAN_POINT('',(58.,-34.4324894531109,131.581397433607));
#48929=CARTESIAN_POINT('Origin',(14.,-35.4582091790453,132.331838201602));
#48930=CARTESIAN_POINT('Origin',(14.,-33.5882749320356,130.762333212168));
#48931=CARTESIAN_POINT('Origin',(14.,-35.0099214429613,134.522508899283));
#48932=CARTESIAN_POINT('Origin',(57.5,-47.070953611875,130.788284360904));
#48933=CARTESIAN_POINT('',(57.5,-46.3841944650247,130.508796018164));
#48934=CARTESIAN_POINT('',(58.,-46.8553022968291,130.334686134323));
#48935=CARTESIAN_POINT('',(57.5,-46.3841944650247,130.508796018164));
#48936=CARTESIAN_POINT('',(57.5,-47.070953611875,130.788284360904));
#48937=CARTESIAN_POINT('',(57.5,-47.070953611875,130.788284360904));
#48938=CARTESIAN_POINT('',(58.,-46.8553022968291,130.334686134323));
#48939=CARTESIAN_POINT('Origin',(57.5,-48.3570826171013,129.790723455271));
#48940=CARTESIAN_POINT('',(57.5,-48.0106462326609,130.446264217578));
#48941=CARTESIAN_POINT('',(58.,-47.8842774043812,129.960169823373));
#48942=CARTESIAN_POINT('',(57.5,-48.0106462326609,130.446264217578));
#48943=CARTESIAN_POINT('',(57.5,-48.3570826171013,129.790723455271));
#48944=CARTESIAN_POINT('',(57.5,-48.3570826171013,129.790723455271));
#48945=CARTESIAN_POINT('',(58.,-47.8842774043812,129.960169823373));
#48946=CARTESIAN_POINT('Origin',(14.,-46.8553022968291,130.334686134323));
#48947=CARTESIAN_POINT('',(14.5,-46.3841944650247,130.508796018164));
#48948=CARTESIAN_POINT('',(14.5,-47.070953611875,130.788284360904));
#48949=CARTESIAN_POINT('',(14.5,-46.3841944650247,130.508796018164));
#48950=CARTESIAN_POINT('',(14.,-46.8553022968291,130.334686134323));
#48951=CARTESIAN_POINT('',(14.,-46.8553022968291,130.334686134323));
#48952=CARTESIAN_POINT('',(14.5,-47.070953611875,130.788284360904));
#48953=CARTESIAN_POINT('Origin',(14.25,-45.5442886531881,128.188157716154));
#48954=CARTESIAN_POINT('',(14.,-45.7695378603898,128.079701297925));
#48955=CARTESIAN_POINT('',(14.5,-45.3190394459863,128.296614134382));
#48956=CARTESIAN_POINT('Origin',(14.5,-48.3570826171013,129.790723455271));
#48957=CARTESIAN_POINT('',(14.,-47.8842774043812,129.960169823373));
#48958=CARTESIAN_POINT('',(14.5,-48.0106462326609,130.446264217578));
#48959=CARTESIAN_POINT('',(14.,-47.8842774043812,129.960169823373));
#48960=CARTESIAN_POINT('',(14.5,-48.3570826171013,129.790723455271));
#48961=CARTESIAN_POINT('',(14.5,-48.3570826171013,129.790723455271));
#48962=CARTESIAN_POINT('',(14.5,-48.0106462326609,130.446264217578));
#48963=CARTESIAN_POINT('Origin',(14.25,-48.0049120124002,129.420919600612));
#48964=CARTESIAN_POINT('',(14.5,-48.2471773577224,129.359214637636));
#48965=CARTESIAN_POINT('',(14.,-47.762646667078,129.482624563588));
#48966=CARTESIAN_POINT('Origin',(14.,-48.1838644248811,130.118493836425));
#48967=CARTESIAN_POINT('',(14.,-48.0106462326609,130.446264217578));
#48968=CARTESIAN_POINT('',(14.,-48.3570826171013,129.790723455271));
#48969=CARTESIAN_POINT('Origin',(14.25,-46.9854485760436,130.553361205708));
#48970=CARTESIAN_POINT('',(14.5,-47.070953611875,130.788284360904));
#48971=CARTESIAN_POINT('',(14.,-46.8999435402122,130.318438050511));
#48972=CARTESIAN_POINT('Origin',(14.,-46.7275740384498,130.648540189534));
#48973=CARTESIAN_POINT('',(14.,-46.3841944650247,130.508796018164));
#48974=CARTESIAN_POINT('',(14.,-47.070953611875,130.788284360904));
#48975=CARTESIAN_POINT('Origin',(57.75,-48.0049120124002,129.420919600612));
#48976=CARTESIAN_POINT('',(58.,-47.762646667078,129.482624563588));
#48977=CARTESIAN_POINT('',(57.5,-48.2471773577224,129.359214637636));
#48978=CARTESIAN_POINT('Origin',(57.75,-46.9854485760436,130.553361205708));
#48979=CARTESIAN_POINT('',(58.,-46.8999435402122,130.318438050511));
#48980=CARTESIAN_POINT('',(57.5,-47.070953611875,130.788284360904));
#48981=CARTESIAN_POINT('Origin',(57.75,-45.5442886531881,128.188157716154));
#48982=CARTESIAN_POINT('',(57.5,-45.3190394459863,128.296614134382));
#48983=CARTESIAN_POINT('',(58.,-45.7695378603898,128.079701297925));
#48984=CARTESIAN_POINT('Origin',(14.,-46.8567596356166,128.737889047669));
#48985=CARTESIAN_POINT('Origin',(14.,-44.857149679865,127.337332006754));
#48986=CARTESIAN_POINT('Origin',(14.,-46.601107301482,130.959294432567));
#48987=CARTESIAN_POINT('Origin',(57.75,-56.5433129818713,123.730916769498));
#48988=CARTESIAN_POINT('',(57.7487592975525,-57.9365320709093,126.078806628123));
#48989=CARTESIAN_POINT('',(58.,-58.036420101407,125.755014631118));
#48990=CARTESIAN_POINT('',(58.2319907935076,-58.1286547721085,125.456031378864));
#48991=CARTESIAN_POINT('',(58.,-56.7582524481486,123.603241298728));
#48992=CARTESIAN_POINT('',(57.5,-57.5822796533797,125.969521727281));
#48993=CARTESIAN_POINT('',(57.5,-56.3283735155941,123.858592240269));
#48994=CARTESIAN_POINT('',(50.4896657310029,-47.5990232005882,122.889742627585));
#48995=CARTESIAN_POINT('Origin',(58.,-57.8987018584758,124.164166824021));
#48996=CARTESIAN_POINT('',(58.,-59.0288384007668,125.292242378034));
#48997=CARTESIAN_POINT('',(58.,-58.0794753575685,125.734937635446));
#48998=CARTESIAN_POINT('',(58.,-58.8660496933282,124.827115139388));
#48999=CARTESIAN_POINT('Origin',(57.75,-58.1851299230037,125.961514582206));
#49000=CARTESIAN_POINT('',(57.5,-58.2907844884389,126.188091528965));
#49001=CARTESIAN_POINT('',(57.5,-58.2907844884389,126.188091528965));
#49002=CARTESIAN_POINT('',(57.5,-59.1970922754756,125.765473267224));
#49003=CARTESIAN_POINT('',(57.5,-58.2907844884389,126.188091528965));
#49004=CARTESIAN_POINT('',(57.5,-59.1970922754756,125.765473267224));
#49005=CARTESIAN_POINT('Origin',(14.,-57.9365320709093,126.078806628123));
#49006=CARTESIAN_POINT('',(14.5,-57.5822796533797,125.969521727281));
#49007=CARTESIAN_POINT('',(14.,-57.5822796533797,125.969521727281));
#49008=CARTESIAN_POINT('',(14.5,-58.2907844884389,126.188091528965));
#49009=CARTESIAN_POINT('',(14.5,-57.5822796533797,125.969521727281));
#49010=CARTESIAN_POINT('',(14.,-58.2907844884389,126.188091528965));
#49011=CARTESIAN_POINT('Origin',(57.5,-59.4850762228408,125.08223311503));
#49012=CARTESIAN_POINT('',(57.5,-59.4850762228408,125.08223311503));
#49013=CARTESIAN_POINT('',(57.5,-59.4850762228408,125.08223311503));
#49014=CARTESIAN_POINT('',(58.,-59.0288384007668,125.292242378034));
#49015=CARTESIAN_POINT('Origin',(14.,-58.036420101407,125.755014631118));
#49016=CARTESIAN_POINT('',(14.,-58.036420101407,125.755014631118));
#49017=CARTESIAN_POINT('',(14.,-58.036420101407,125.755014631118));
#49018=CARTESIAN_POINT('',(14.5,-58.2907844884389,126.188091528965));
#49019=CARTESIAN_POINT('Origin',(14.25,-56.5433129818713,123.730916769498));
#49020=CARTESIAN_POINT('',(14.,-56.7582524481486,123.603241298728));
#49021=CARTESIAN_POINT('',(14.5,-56.3283735155941,123.858592240269));
#49022=CARTESIAN_POINT('Origin',(14.5,-59.4850762228408,125.08223311503));
#49023=CARTESIAN_POINT('',(14.,-59.0288384007668,125.292242378034));
#49024=CARTESIAN_POINT('',(14.5,-59.1970922754756,125.765473267224));
#49025=CARTESIAN_POINT('',(14.,-59.0288384007668,125.292242378034));
#49026=CARTESIAN_POINT('',(14.5,-59.4850762228408,125.08223311503));
#49027=CARTESIAN_POINT('',(14.5,-59.4850762228408,125.08223311503));
#49028=CARTESIAN_POINT('',(14.5,-59.1970922754756,125.765473267224));
#49029=CARTESIAN_POINT('Origin',(14.25,-59.1020152039901,124.744530166311));
#49030=CARTESIAN_POINT('',(14.5,-59.3379807146521,124.661945193235));
#49031=CARTESIAN_POINT('',(14.,-58.8660496933282,124.827115139388));
#49032=CARTESIAN_POINT('Origin',(14.,-59.3410842491582,125.423853191127));
#49033=CARTESIAN_POINT('',(14.,-59.1970922754756,125.765473267224));
#49034=CARTESIAN_POINT('',(14.,-59.4850762228408,125.08223311503));
#49035=CARTESIAN_POINT('Origin',(14.25,-58.1851299230037,125.961514582206));
#49036=CARTESIAN_POINT('',(14.5,-58.2907844884389,126.188091528965));
#49037=CARTESIAN_POINT('',(14.,-58.0794753575686,125.734937635446));
#49038=CARTESIAN_POINT('Origin',(57.75,-59.1020152039902,124.744530166311));
#49039=CARTESIAN_POINT('',(57.5,-59.3379807146521,124.661945193235));
#49040=CARTESIAN_POINT('Origin',(14.,-55.7846344331431,122.943216816385));
#49041=CARTESIAN_POINT('Origin',(14.,-57.8376305949206,126.399400659835));
#49042=CARTESIAN_POINT('Origin',(57.5,-69.0669872981078,120.627531126037));
#49043=CARTESIAN_POINT('',(57.5,-68.3421289244415,120.471543313576));
#49044=CARTESIAN_POINT('',(58.,-68.7758457056646,120.218271533617));
#49045=CARTESIAN_POINT('',(57.5,-68.3421289244415,120.471543313576));
#49046=CARTESIAN_POINT('',(57.5,-69.0669872981078,120.627531126037));
#49047=CARTESIAN_POINT('',(57.5,-69.0669872981078,120.627531126037));
#49048=CARTESIAN_POINT('',(58.,-68.7758457056646,120.218271533617));
#49049=CARTESIAN_POINT('Origin',(57.5,-70.1603524804535,119.421791454066));
#49050=CARTESIAN_POINT('',(57.5,-69.9330127018922,120.127531126037));
#49051=CARTESIAN_POINT('',(58.,-69.7241542943354,119.670765314673));
#49052=CARTESIAN_POINT('',(57.5,-69.9330127018922,120.127531126037));
#49053=CARTESIAN_POINT('',(57.5,-70.1603524804535,119.421791454066));
#49054=CARTESIAN_POINT('',(57.5,-70.1603524804535,119.421791454066));
#49055=CARTESIAN_POINT('',(58.,-69.7241542943354,119.670765314673));
#49056=CARTESIAN_POINT('Origin',(14.,-68.7758457056646,120.218271533617));
#49057=CARTESIAN_POINT('',(14.5,-68.3421289244415,120.471543313576));
#49058=CARTESIAN_POINT('',(14.5,-69.0669872981078,120.627531126037));
#49059=CARTESIAN_POINT('',(14.5,-68.3421289244415,120.471543313576));
#49060=CARTESIAN_POINT('',(14.,-68.7758457056646,120.218271533617));
#49061=CARTESIAN_POINT('',(14.,-68.7758457056646,120.218271533617));
#49062=CARTESIAN_POINT('',(14.5,-69.0669872981078,120.627531126037));
#49063=CARTESIAN_POINT('Origin',(14.25,-67.1120085569767,118.332008835457));
#49064=CARTESIAN_POINT('',(14.,-67.3150024632071,118.18608599957));
#49065=CARTESIAN_POINT('',(14.5,-66.9090146507463,118.477931671344));
#49066=CARTESIAN_POINT('Origin',(14.5,-70.1603524804535,119.421791454066));
#49067=CARTESIAN_POINT('',(14.,-69.7241542943354,119.670765314673));
#49068=CARTESIAN_POINT('',(14.5,-69.9330127018922,120.127531126037));
#49069=CARTESIAN_POINT('',(14.,-69.7241542943354,119.670765314673));
#49070=CARTESIAN_POINT('',(14.5,-70.1603524804535,119.421791454066));
#49071=CARTESIAN_POINT('',(14.5,-70.1603524804535,119.421791454066));
#49072=CARTESIAN_POINT('',(14.5,-69.9330127018922,120.127531126037));
#49073=CARTESIAN_POINT('Origin',(14.25,-69.7493163731052,119.118759534638));
#49074=CARTESIAN_POINT('',(14.5,-69.9771862090909,119.015923072972));
#49075=CARTESIAN_POINT('',(14.,-69.5214465371196,119.221595996303));
#49076=CARTESIAN_POINT('Origin',(14.,-70.0466825911729,119.774661290051));
#49077=CARTESIAN_POINT('',(14.,-69.9330127018922,120.127531126037));
#49078=CARTESIAN_POINT('',(14.,-70.1603524804535,119.421791454066));
#49079=CARTESIAN_POINT('Origin',(14.25,-68.9419872981078,120.411024775091));
#49080=CARTESIAN_POINT('',(14.5,-69.0669872981078,120.627531126037));
#49081=CARTESIAN_POINT('',(14.,-68.8169872981078,120.194518424145));
#49082=CARTESIAN_POINT('Origin',(14.,-68.7045581112746,120.549537219807));
#49083=CARTESIAN_POINT('',(14.,-68.3421289244415,120.471543313576));
#49084=CARTESIAN_POINT('',(14.,-69.0669872981078,120.627531126037));
#49085=CARTESIAN_POINT('Origin',(57.75,-69.7493163731052,119.118759534638));
#49086=CARTESIAN_POINT('',(58.,-69.5214465371196,119.221595996303));
#49087=CARTESIAN_POINT('',(57.5,-69.9771862090909,119.015923072972));
#49088=CARTESIAN_POINT('Origin',(57.75,-68.9419872981078,120.411024775091));
#49089=CARTESIAN_POINT('',(58.,-68.8169872981078,120.194518424145));
#49090=CARTESIAN_POINT('',(57.5,-69.0669872981078,120.627531126037));
#49091=CARTESIAN_POINT('Origin',(57.75,-67.1120085569767,118.332008835457));
#49092=CARTESIAN_POINT('',(57.5,-66.9090146507463,118.477931671344));
#49093=CARTESIAN_POINT('',(58.,-67.3150024632071,118.18608599957));
#49094=CARTESIAN_POINT('Origin',(14.,-68.5,118.645480318468));
#49095=CARTESIAN_POINT('Origin',(14.,-66.2875644347018,117.613429510899));
#49096=CARTESIAN_POINT('Origin',(14.,-68.6339745962156,120.877531126037));
#49097=CARTESIAN_POINT('Origin',(57.5,-80.3016660917109,112.852477851287));
#49098=CARTESIAN_POINT('',(57.5,-80.1367006749399,113.575345937994));
#49099=CARTESIAN_POINT('',(58.,-79.8888272731288,113.138521468083));
#49100=CARTESIAN_POINT('',(57.5,-80.1367006749399,113.575345937994));
#49101=CARTESIAN_POINT('',(57.5,-80.3016660917109,112.852477851287));
#49102=CARTESIAN_POINT('',(57.5,-80.3016660917109,112.852477851287));
#49103=CARTESIAN_POINT('',(58.,-79.8888272731288,113.138521468083));
#49104=CARTESIAN_POINT('Origin',(14.,-80.2191833833254,113.213911894641));
#49105=CARTESIAN_POINT('',(14.2512407024475,-80.2191833833254,113.213911894641));
#49106=CARTESIAN_POINT('',(14.5,-80.3016660917109,112.852477851287));
#49107=CARTESIAN_POINT('',(14.3353834448875,-80.2470831296091,113.091656960179));
#49108=CARTESIAN_POINT('',(14.,-80.3016660917109,112.852477851287));
#49109=CARTESIAN_POINT('',(14.5,-80.1367006749399,113.575345937994));
#49110=CARTESIAN_POINT('',(14.,-80.1367006749399,113.575345937994));
#49111=CARTESIAN_POINT('',(14.4305329766294,-80.159734299361,113.474414043655));
#49112=CARTESIAN_POINT('Origin',(57.75,-79.8657831288323,112.586423217032));
#49113=CARTESIAN_POINT('',(58.,-79.6477431945663,112.708728519719));
#49114=CARTESIAN_POINT('',(57.5,-80.0838230630982,112.464117914346));
#49115=CARTESIAN_POINT('Origin',(57.5,-79.3175486306509,114.148922374345));
#49116=CARTESIAN_POINT('',(57.5,-78.5818533282825,114.056703712549));
#49117=CARTESIAN_POINT('',(58.,-78.991845596111,113.766594799967));
#49118=CARTESIAN_POINT('',(57.5,-78.5818533282825,114.056703712549));
#49119=CARTESIAN_POINT('',(57.5,-79.3175486306509,114.148922374345));
#49120=CARTESIAN_POINT('',(57.5,-79.3175486306509,114.148922374345));
#49121=CARTESIAN_POINT('',(58.,-78.991845596111,113.766594799967));
#49122=CARTESIAN_POINT('Origin',(14.,-78.9497009794667,114.102813043447));
#49123=CARTESIAN_POINT('',(14.2512407024475,-78.9497009794667,114.102813043447));
#49124=CARTESIAN_POINT('',(14.5,-79.3175486306509,114.148922374345));
#49125=CARTESIAN_POINT('',(14.2590041943422,-78.9611810820661,114.104252062693));
#49126=CARTESIAN_POINT('',(14.,-79.3175486306509,114.148922374345));
#49127=CARTESIAN_POINT('',(14.5,-78.5818533282825,114.056703712549));
#49128=CARTESIAN_POINT('',(14.,-78.5818533282825,114.056703712549));
#49129=CARTESIAN_POINT('',(14.6801520303733,-78.3154572503032,114.023311233706));
#49130=CARTESIAN_POINT('Origin',(57.75,-79.1741545215632,113.944134363273));
#49131=CARTESIAN_POINT('',(58.,-79.0307604124754,113.739346352201));
#49132=CARTESIAN_POINT('',(57.5,-79.3175486306509,114.148922374345));
#49133=CARTESIAN_POINT('Origin',(57.75,-77.1699412236247,112.032522863357));
#49134=CARTESIAN_POINT('',(57.5,-76.9804377836387,112.195582503469));
#49135=CARTESIAN_POINT('',(58.,-77.3594446636108,111.869463223246));
#49136=CARTESIAN_POINT('Origin',(14.25,-79.8657831288323,112.586423217032));
#49137=CARTESIAN_POINT('',(14.,-79.8888272731288,113.138521468083));
#49138=CARTESIAN_POINT('',(14.5,-80.5462766970844,113.288557719819));
#49139=CARTESIAN_POINT('',(14.,-79.6477431945663,112.708728519719));
#49140=CARTESIAN_POINT('',(14.5,-80.0838230630982,112.464117914346));
#49141=CARTESIAN_POINT('Origin',(14.,-78.9079726085064,114.435710592521));
#49142=CARTESIAN_POINT('',(14.5,-79.3175486306509,114.148922374345));
#49143=CARTESIAN_POINT('Origin',(14.25,-79.1741545215632,113.944134363273));
#49144=CARTESIAN_POINT('',(14.,-78.991845596111,113.766594799967));
#49145=CARTESIAN_POINT('',(14.,-78.991845596111,113.766594799967));
#49146=CARTESIAN_POINT('',(14.,-79.0307604124754,113.739346352201));
#49147=CARTESIAN_POINT('Origin',(14.25,-77.1699412236247,112.032522863357));
#49148=CARTESIAN_POINT('',(14.5,-76.9804377836387,112.195582503469));
#49149=CARTESIAN_POINT('',(14.,-77.3594446636108,111.869463223246));
#49150=CARTESIAN_POINT('Origin',(14.,-76.2860060453866,111.388532989905));
#49151=CARTESIAN_POINT('Origin',(14.,-80.5462766970844,113.288557719819));
#49152=CARTESIAN_POINT('Origin',(57.5,-88.9644555248695,106.801571398381));
#49153=CARTESIAN_POINT('',(57.5,-88.223522379275,106.773823726948));
#49154=CARTESIAN_POINT('',(58.,-88.6066698449906,106.449085585742));
#49155=CARTESIAN_POINT('',(57.5,-88.223522379275,106.773823726948));
#49156=CARTESIAN_POINT('',(57.5,-88.9644555248695,106.801571398381));
#49157=CARTESIAN_POINT('',(57.5,-88.9644555248695,106.801571398381));
#49158=CARTESIAN_POINT('',(58.,-88.6066698449906,106.449085585742));
#49159=CARTESIAN_POINT('Origin',(57.5,-89.8318355365387,105.424288749871));
#49160=CARTESIAN_POINT('',(57.5,-89.7304999679885,106.158783788695));
#49161=CARTESIAN_POINT('',(58.,-89.4454980381808,105.745225158215));
#49162=CARTESIAN_POINT('',(57.5,-89.7304999679885,106.158783788695));
#49163=CARTESIAN_POINT('',(57.5,-89.8318355365387,105.424288749871));
#49164=CARTESIAN_POINT('',(57.5,-89.8318355365387,105.424288749871));
#49165=CARTESIAN_POINT('',(58.,-89.4454980381808,105.745225158215));
#49166=CARTESIAN_POINT('Origin',(14.,-88.6066698449906,106.449085585742));
#49167=CARTESIAN_POINT('',(14.5,-88.223522379275,106.773823726948));
#49168=CARTESIAN_POINT('',(14.5,-88.9644555248695,106.801571398381));
#49169=CARTESIAN_POINT('',(14.5,-88.223522379275,106.773823726948));
#49170=CARTESIAN_POINT('',(14.,-88.6066698449906,106.449085585742));
#49171=CARTESIAN_POINT('',(14.,-88.6066698449906,106.449085585742));
#49172=CARTESIAN_POINT('',(14.5,-88.9644555248695,106.801571398381));
#49173=CARTESIAN_POINT('Origin',(14.25,-86.6405640410765,104.880401745181));
#49174=CARTESIAN_POINT('',(14.,-86.8151347792147,104.701446283163));
#49175=CARTESIAN_POINT('',(14.5,-86.4659933029384,105.059357207198));
#49176=CARTESIAN_POINT('Origin',(14.5,-89.8318355365387,105.424288749871));
#49177=CARTESIAN_POINT('',(14.,-89.4454980381808,105.745225158215));
#49178=CARTESIAN_POINT('',(14.5,-89.7304999679885,106.158783788695));
#49179=CARTESIAN_POINT('',(14.,-89.4454980381808,105.745225158215));
#49180=CARTESIAN_POINT('',(14.5,-89.8318355365387,105.424288749871));
#49181=CARTESIAN_POINT('',(14.5,-89.8318355365387,105.424288749871));
#49182=CARTESIAN_POINT('',(14.5,-89.7304999679885,106.158783788695));
#49183=CARTESIAN_POINT('Origin',(14.25,-89.3744230506705,105.197236237204));
#49184=CARTESIAN_POINT('',(14.5,-89.5809736676609,105.0563929107));
#49185=CARTESIAN_POINT('',(14.,-89.1678724336801,105.338079563709));
#49186=CARTESIAN_POINT('Origin',(14.,-89.7811677522636,105.791536269283));
#49187=CARTESIAN_POINT('',(14.,-89.7304999679885,106.158783788695));
#49188=CARTESIAN_POINT('',(14.,-89.8318355365387,105.424288749871));
#49189=CARTESIAN_POINT('Origin',(14.25,-88.8037586224479,106.610060287601));
#49190=CARTESIAN_POINT('',(14.5,-88.9644555248695,106.801571398381));
#49191=CARTESIAN_POINT('',(14.,-88.6430617200262,106.418549176822));
#49192=CARTESIAN_POINT('Origin',(14.,-88.5939889520722,106.787697562665));
#49193=CARTESIAN_POINT('',(14.,-88.223522379275,106.773823726948));
#49194=CARTESIAN_POINT('',(14.,-88.9644555248695,106.801571398381));
#49195=CARTESIAN_POINT('Origin',(57.75,-89.3744230506705,105.197236237204));
#49196=CARTESIAN_POINT('',(58.,-89.1678724336801,105.338079563709));
#49197=CARTESIAN_POINT('',(57.5,-89.5809736676609,105.0563929107));
#49198=CARTESIAN_POINT('Origin',(57.75,-88.8037586224478,106.610060287601));
#49199=CARTESIAN_POINT('',(58.,-88.6430617200262,106.418549176822));
#49200=CARTESIAN_POINT('',(57.5,-88.9644555248695,106.801571398381));
#49201=CARTESIAN_POINT('Origin',(57.75,-86.6405640410765,104.880401745181));
#49202=CARTESIAN_POINT('',(57.5,-86.4659933029383,105.059357207198));
#49203=CARTESIAN_POINT('',(58.,-86.8151347792147,104.701446283163));
#49204=CARTESIAN_POINT('Origin',(14.,-88.0619025270559,104.9480887073));
#49205=CARTESIAN_POINT('Origin',(14.,-85.7038650873162,104.315902474623));
#49206=CARTESIAN_POINT('Origin',(14.,-88.58143330331,107.122965203225));
#49207=CARTESIAN_POINT('Origin',(57.5,-97.9342891943368,98.6413959755234));
#49208=CARTESIAN_POINT('',(57.5,-97.1937571541419,98.678330470988));
#49209=CARTESIAN_POINT('',(58.,-97.5471438341797,98.3214345544939));
#49210=CARTESIAN_POINT('',(57.5,-97.1937571541419,98.678330470988));
#49211=CARTESIAN_POINT('',(57.5,-97.9342891943368,98.6413959755234));
#49212=CARTESIAN_POINT('',(57.5,-97.9342891943368,98.6413959755234));
#49213=CARTESIAN_POINT('',(58.,-97.5471438341797,98.3214345544939));
#49214=CARTESIAN_POINT('Origin',(57.5,-98.678330470988,97.1937571541419));
#49215=CARTESIAN_POINT('',(57.5,-98.6413959755234,97.9342891943368));
#49216=CARTESIAN_POINT('',(58.,-98.3214345544939,97.5471438341798));
#49217=CARTESIAN_POINT('',(57.5,-98.6413959755234,97.9342891943368));
#49218=CARTESIAN_POINT('',(57.5,-98.678330470988,97.1937571541419));
#49219=CARTESIAN_POINT('',(57.5,-98.678330470988,97.1937571541419));
#49220=CARTESIAN_POINT('',(58.,-98.3214345544939,97.5471438341798));
#49221=CARTESIAN_POINT('Origin',(14.,-97.5471438341798,98.3214345544939));
#49222=CARTESIAN_POINT('',(14.5,-97.1937571541419,98.678330470988));
#49223=CARTESIAN_POINT('',(14.5,-97.9342891943368,98.6413959755234));
#49224=CARTESIAN_POINT('',(14.5,-97.1937571541419,98.678330470988));
#49225=CARTESIAN_POINT('',(14.,-97.5471438341798,98.3214345544939));
#49226=CARTESIAN_POINT('',(14.,-97.5471438341798,98.3214345544939));
#49227=CARTESIAN_POINT('',(14.5,-97.9342891943368,98.6413959755234));
#49228=CARTESIAN_POINT('Origin',(14.25,-95.4517998511728,96.9300774412053));
#49229=CARTESIAN_POINT('',(14.,-95.6101092987371,96.7365881164044));
#49230=CARTESIAN_POINT('',(14.5,-95.2934904036084,97.1235667660061));
#49231=CARTESIAN_POINT('Origin',(14.5,-98.678330470988,97.1937571541419));
#49232=CARTESIAN_POINT('',(14.,-98.3214345544939,97.5471438341798));
#49233=CARTESIAN_POINT('',(14.5,-98.6413959755234,97.9342891943368));
#49234=CARTESIAN_POINT('',(14.,-98.3214345544939,97.5471438341798));
#49235=CARTESIAN_POINT('',(14.5,-98.678330470988,97.1937571541419));
#49236=CARTESIAN_POINT('',(14.5,-98.678330470988,97.1937571541419));
#49237=CARTESIAN_POINT('',(14.5,-98.6413959755234,97.9342891943368));
#49238=CARTESIAN_POINT('Origin',(14.25,-98.2028696473411,97.0074347697832));
#49239=CARTESIAN_POINT('',(14.5,-98.3963589721419,96.8491253222189));
#49240=CARTESIAN_POINT('',(14.,-98.0093803225402,97.1657442173475));
#49241=CARTESIAN_POINT('Origin',(14.,-98.6598632232557,97.5640231742394));
#49242=CARTESIAN_POINT('',(14.,-98.6413959755234,97.9342891943368));
#49243=CARTESIAN_POINT('',(14.,-98.678330470988,97.1937571541419));
#49244=CARTESIAN_POINT('Origin',(14.25,-97.7575124990402,98.4646192802267));
#49245=CARTESIAN_POINT('',(14.5,-97.9342891943368,98.6413959755234));
#49246=CARTESIAN_POINT('',(14.,-97.5807358037436,98.2878425849301));
#49247=CARTESIAN_POINT('Origin',(14.,-97.5640231742394,98.6598632232557));
#49248=CARTESIAN_POINT('',(14.,-97.1937571541419,98.678330470988));
#49249=CARTESIAN_POINT('',(14.,-97.9342891943368,98.6413959755234));
#49250=CARTESIAN_POINT('Origin',(57.75,-98.2028696473411,97.0074347697832));
#49251=CARTESIAN_POINT('',(58.,-98.0093803225402,97.1657442173475));
#49252=CARTESIAN_POINT('',(57.5,-98.3963589721419,96.8491253222189));
#49253=CARTESIAN_POINT('Origin',(57.75,-97.7575124990402,98.4646192802267));
#49254=CARTESIAN_POINT('',(58.,-97.5807358037436,98.2878425849301));
#49255=CARTESIAN_POINT('',(57.5,-97.9342891943368,98.6413959755234));
#49256=CARTESIAN_POINT('Origin',(57.75,-95.4517998511728,96.9300774412053));
#49257=CARTESIAN_POINT('',(57.5,-95.2934904036084,97.1235667660061));
#49258=CARTESIAN_POINT('',(58.,-95.6101092987371,96.7365881164045));
#49259=CARTESIAN_POINT('Origin',(14.,-96.873629022557,96.873629022557));
#49260=CARTESIAN_POINT('Origin',(14.,-94.4694659665227,96.4493649538451));
#49261=CARTESIAN_POINT('Origin',(14.,-97.5807358037436,98.9949493661167));
#49262=CARTESIAN_POINT('Origin',(57.75,-103.536589829029,88.2420567199213));
#49263=CARTESIAN_POINT('',(57.7487592975525,-105.791536269283,89.7811677522636));
#49264=CARTESIAN_POINT('',(58.,-105.745225158215,89.4454980381808));
#49265=CARTESIAN_POINT('',(58.2319907935076,-105.702462376149,89.1355471322649));
#49266=CARTESIAN_POINT('',(58.,-103.677433155534,88.0355061029309));
#49267=CARTESIAN_POINT('',(57.5,-105.424288749871,89.8318355365387));
#49268=CARTESIAN_POINT('',(57.5,-103.395746502524,88.4486073369116));
#49269=CARTESIAN_POINT('',(50.4896657310024,-95.0748147970629,91.2597142447225));
#49270=CARTESIAN_POINT('Origin',(58.,-104.9480887073,88.0619025270559));
#49271=CARTESIAN_POINT('',(58.,-106.449085585742,88.6066698449906));
#49272=CARTESIAN_POINT('',(58.,-105.775761567135,89.4091061631452));
#49273=CARTESIAN_POINT('',(58.,-106.104977647464,88.2539188872116));
#49274=CARTESIAN_POINT('Origin',(57.75,-105.967272677915,89.5698030655668));
#49275=CARTESIAN_POINT('',(57.5,-106.158783788695,89.7304999679884));
#49276=CARTESIAN_POINT('',(57.5,-106.158783788695,89.7304999679884));
#49277=CARTESIAN_POINT('',(57.5,-106.801571398381,88.9644555248695));
#49278=CARTESIAN_POINT('',(57.5,-106.158783788695,89.7304999679885));
#49279=CARTESIAN_POINT('',(57.5,-106.801571398381,88.9644555248695));
#49280=CARTESIAN_POINT('Origin',(14.,-105.791536269283,89.7811677522635));
#49281=CARTESIAN_POINT('',(14.5,-105.424288749871,89.8318355365387));
#49282=CARTESIAN_POINT('',(14.,-105.424288749871,89.8318355365387));
#49283=CARTESIAN_POINT('',(14.5,-106.158783788695,89.7304999679884));
#49284=CARTESIAN_POINT('',(14.5,-105.424288749871,89.8318355365387));
#49285=CARTESIAN_POINT('',(14.,-106.158783788695,89.7304999679884));
#49286=CARTESIAN_POINT('Origin',(57.5,-106.773823726948,88.223522379275));
#49287=CARTESIAN_POINT('',(57.5,-106.773823726948,88.223522379275));
#49288=CARTESIAN_POINT('',(57.5,-106.773823726948,88.223522379275));
#49289=CARTESIAN_POINT('',(58.,-106.449085585742,88.6066698449906));
#49290=CARTESIAN_POINT('Origin',(14.,-105.745225158215,89.4454980381808));
#49291=CARTESIAN_POINT('',(14.,-105.745225158215,89.4454980381808));
#49292=CARTESIAN_POINT('',(14.,-105.745225158215,89.4454980381808));
#49293=CARTESIAN_POINT('',(14.5,-106.158783788695,89.7304999679884));
#49294=CARTESIAN_POINT('Origin',(14.25,-103.536589829029,88.2420567199213));
#49295=CARTESIAN_POINT('',(14.,-103.677433155534,88.0355061029309));
#49296=CARTESIAN_POINT('',(14.5,-103.395746502524,88.4486073369116));
#49297=CARTESIAN_POINT('Origin',(14.5,-106.773823726948,88.223522379275));
#49298=CARTESIAN_POINT('',(14.,-106.449085585742,88.6066698449906));
#49299=CARTESIAN_POINT('',(14.5,-106.801571398381,88.9644555248695));
#49300=CARTESIAN_POINT('',(14.,-106.449085585742,88.6066698449906));
#49301=CARTESIAN_POINT('',(14.5,-106.773823726948,88.223522379275));
#49302=CARTESIAN_POINT('',(14.5,-106.773823726948,88.223522379275));
#49303=CARTESIAN_POINT('',(14.5,-106.801571398381,88.9644555248695));
#49304=CARTESIAN_POINT('Origin',(14.25,-106.283933109481,88.0793481490734));
#49305=CARTESIAN_POINT('',(14.5,-106.462888571499,87.9047774109352));
#49306=CARTESIAN_POINT('',(14.,-106.104977647464,88.2539188872116));
#49307=CARTESIAN_POINT('Origin',(14.,-106.787697562665,88.5939889520722));
#49308=CARTESIAN_POINT('',(14.,-106.801571398381,88.9644555248695));
#49309=CARTESIAN_POINT('',(14.,-106.773823726948,88.223522379275));
#49310=CARTESIAN_POINT('Origin',(14.25,-105.967272677915,89.5698030655668));
#49311=CARTESIAN_POINT('',(14.5,-106.158783788695,89.7304999679885));
#49312=CARTESIAN_POINT('',(14.,-105.775761567135,89.4091061631452));
#49313=CARTESIAN_POINT('Origin',(57.75,-106.283933109481,88.0793481490734));
#49314=CARTESIAN_POINT('',(57.5,-106.462888571499,87.9047774109352));
#49315=CARTESIAN_POINT('Origin',(14.,-102.516097167501,87.8487895280494));
#49316=CARTESIAN_POINT('Origin',(14.,-105.837389983851,90.113522189548));
#49317=CARTESIAN_POINT('Origin',(57.5,-113.575345937994,80.1367006749399));
#49318=CARTESIAN_POINT('',(57.5,-112.852477851287,80.3016660917109));
#49319=CARTESIAN_POINT('',(58.,-113.138521468083,79.8888272731288));
#49320=CARTESIAN_POINT('',(57.5,-112.852477851287,80.3016660917109));
#49321=CARTESIAN_POINT('',(57.5,-113.575345937994,80.1367006749399));
#49322=CARTESIAN_POINT('',(57.5,-113.575345937994,80.1367006749399));
#49323=CARTESIAN_POINT('',(58.,-113.138521468083,79.8888272731288));
#49324=CARTESIAN_POINT('Origin',(57.5,-114.056703712549,78.5818533282825));
#49325=CARTESIAN_POINT('',(57.5,-114.148922374345,79.3175486306509));
#49326=CARTESIAN_POINT('',(58.,-113.766594799967,78.991845596111));
#49327=CARTESIAN_POINT('',(57.5,-114.148922374345,79.3175486306509));
#49328=CARTESIAN_POINT('',(57.5,-114.056703712549,78.5818533282825));
#49329=CARTESIAN_POINT('',(57.5,-114.056703712549,78.5818533282825));
#49330=CARTESIAN_POINT('',(58.,-113.766594799967,78.991845596111));
#49331=CARTESIAN_POINT('Origin',(14.,-113.138521468083,79.8888272731288));
#49332=CARTESIAN_POINT('',(14.5,-112.852477851287,80.3016660917109));
#49333=CARTESIAN_POINT('',(14.5,-113.575345937994,80.1367006749399));
#49334=CARTESIAN_POINT('',(14.5,-112.852477851287,80.3016660917109));
#49335=CARTESIAN_POINT('',(14.,-113.138521468083,79.8888272731288));
#49336=CARTESIAN_POINT('',(14.,-113.138521468083,79.8888272731288));
#49337=CARTESIAN_POINT('',(14.5,-113.575345937994,80.1367006749399));
#49338=CARTESIAN_POINT('Origin',(14.25,-110.833403841184,78.882460664988));
#49339=CARTESIAN_POINT('',(14.,-110.955709143871,78.664420730722));
#49340=CARTESIAN_POINT('',(14.5,-110.711098538497,79.1005005992539));
#49341=CARTESIAN_POINT('Origin',(14.5,-114.056703712549,78.5818533282825));
#49342=CARTESIAN_POINT('',(14.,-113.766594799967,78.991845596111));
#49343=CARTESIAN_POINT('',(14.5,-114.148922374345,79.3175486306509));
#49344=CARTESIAN_POINT('',(14.,-113.766594799967,78.991845596111));
#49345=CARTESIAN_POINT('',(14.5,-114.056703712549,78.5818533282825));
#49346=CARTESIAN_POINT('',(14.5,-114.056703712549,78.5818533282825));
#49347=CARTESIAN_POINT('',(14.5,-114.148922374345,79.3175486306509));
#49348=CARTESIAN_POINT('Origin',(14.25,-113.556111664665,78.4809245051846));
#49349=CARTESIAN_POINT('',(14.5,-113.719171304777,78.2914210651985));
#49350=CARTESIAN_POINT('',(14.,-113.393052024553,78.6704279451707));
#49351=CARTESIAN_POINT('Origin',(14.,-114.102813043447,78.9497009794667));
#49352=CARTESIAN_POINT('',(14.,-114.148922374345,79.3175486306509));
#49353=CARTESIAN_POINT('',(14.,-114.056703712549,78.5818533282825));
#49354=CARTESIAN_POINT('Origin',(14.25,-113.370557926922,79.9933065658522));
#49355=CARTESIAN_POINT('',(14.5,-113.575345937994,80.1367006749399));
#49356=CARTESIAN_POINT('',(14.,-113.16576991585,79.8499124567644));
#49357=CARTESIAN_POINT('Origin',(14.,-113.213911894641,80.2191833833254));
#49358=CARTESIAN_POINT('',(14.,-112.852477851287,80.3016660917109));
#49359=CARTESIAN_POINT('',(14.,-113.575345937994,80.1367006749399));
#49360=CARTESIAN_POINT('Origin',(57.75,-113.556111664665,78.4809245051846));
#49361=CARTESIAN_POINT('',(58.,-113.393052024553,78.6704279451707));
#49362=CARTESIAN_POINT('',(57.5,-113.719171304777,78.2914210651985));
#49363=CARTESIAN_POINT('Origin',(57.75,-113.370557926922,79.9933065658522));
#49364=CARTESIAN_POINT('',(58.,-113.16576991585,79.8499124567644));
#49365=CARTESIAN_POINT('',(57.5,-113.575345937994,80.1367006749399));
#49366=CARTESIAN_POINT('Origin',(57.75,-110.833403841184,78.882460664988));
#49367=CARTESIAN_POINT('',(57.5,-110.711098538497,79.1005005992539));
#49368=CARTESIAN_POINT('',(58.,-110.955709143871,78.664420730722));
#49369=CARTESIAN_POINT('Origin',(14.,-112.223830067592,78.5799717800933));
#49370=CARTESIAN_POINT('Origin',(14.,-109.782518968122,78.5796317693958));
#49371=CARTESIAN_POINT('Origin',(14.,-113.288557719819,80.5462766970844));
#49372=CARTESIAN_POINT('Origin',(57.5,-120.471543313576,68.3421289244415));
#49373=CARTESIAN_POINT('',(57.5,-120.627531126037,69.0669872981078));
#49374=CARTESIAN_POINT('',(58.,-120.218271533617,68.7758457056646));
#49375=CARTESIAN_POINT('',(57.5,-120.627531126037,69.0669872981078));
#49376=CARTESIAN_POINT('',(57.5,-120.471543313576,68.3421289244415));
#49377=CARTESIAN_POINT('',(57.5,-120.471543313576,68.3421289244415));
#49378=CARTESIAN_POINT('',(58.,-120.218271533617,68.7758457056646));
#49379=CARTESIAN_POINT('Origin',(14.,-120.549537219807,68.7045581112746));
#49380=CARTESIAN_POINT('',(14.2512407024475,-120.549537219807,68.7045581112746));
#49381=CARTESIAN_POINT('',(14.5,-120.471543313576,68.3421289244415));
#49382=CARTESIAN_POINT('',(14.3353834448874,-120.523155809229,68.5819665698912));
#49383=CARTESIAN_POINT('',(14.,-120.471543313576,68.3421289244415));
#49384=CARTESIAN_POINT('',(14.5,-120.627531126037,69.0669872981078));
#49385=CARTESIAN_POINT('',(14.,-120.627531126037,69.0669872981078));
#49386=CARTESIAN_POINT('',(14.4305329766294,-120.605751017473,68.965777505993));
#49387=CARTESIAN_POINT('Origin',(57.75,-119.964059643026,68.2852136377336));
#49388=CARTESIAN_POINT('',(58.,-119.818136807139,68.488207543964));
#49389=CARTESIAN_POINT('',(57.5,-120.109982478913,68.0822197315032));
#49390=CARTESIAN_POINT('Origin',(57.5,-120.127531126037,69.9330127018922));
#49391=CARTESIAN_POINT('',(57.5,-119.421791454066,70.1603524804536));
#49392=CARTESIAN_POINT('',(58.,-119.670765314673,69.7241542943354));
#49393=CARTESIAN_POINT('',(57.5,-119.421791454066,70.1603524804536));
#49394=CARTESIAN_POINT('',(57.5,-120.127531126037,69.9330127018922));
#49395=CARTESIAN_POINT('',(57.5,-120.127531126037,69.9330127018922));
#49396=CARTESIAN_POINT('',(58.,-119.670765314673,69.7241542943354));
#49397=CARTESIAN_POINT('Origin',(14.,-119.774661290051,70.0466825911729));
#49398=CARTESIAN_POINT('',(14.2512407024475,-119.774661290051,70.0466825911729));
#49399=CARTESIAN_POINT('',(14.5,-120.127531126037,69.9330127018922));
#49400=CARTESIAN_POINT('',(14.2590041943422,-119.785673952245,70.0431350845157));
#49401=CARTESIAN_POINT('',(14.,-120.127531126037,69.9330127018922));
#49402=CARTESIAN_POINT('',(14.5,-119.421791454066,70.1603524804536));
#49403=CARTESIAN_POINT('',(14.,-119.421791454066,70.1603524804536));
#49404=CARTESIAN_POINT('',(14.6801520303733,-119.166242342793,70.24267246426));
#49405=CARTESIAN_POINT('Origin',(57.75,-119.911024775091,69.8080127018922));
#49406=CARTESIAN_POINT('',(58.,-119.694518424145,69.6830127018922));
#49407=CARTESIAN_POINT('',(57.5,-120.127531126037,69.9330127018922));
#49408=CARTESIAN_POINT('Origin',(57.75,-117.286708727069,68.9225214538621));
#49409=CARTESIAN_POINT('',(57.5,-117.183872265404,69.1503912898478));
#49410=CARTESIAN_POINT('',(58.,-117.389545188734,68.6946516178765));
#49411=CARTESIAN_POINT('Origin',(14.25,-119.964059643026,68.2852136377336));
#49412=CARTESIAN_POINT('',(14.,-120.218271533617,68.7758457056646));
#49413=CARTESIAN_POINT('',(14.5,-120.877531126037,68.6339745962156));
#49414=CARTESIAN_POINT('',(14.,-119.818136807139,68.488207543964));
#49415=CARTESIAN_POINT('',(14.5,-120.109982478913,68.0822197315032));
#49416=CARTESIAN_POINT('Origin',(14.,-119.877531126037,70.3660254037845));
#49417=CARTESIAN_POINT('',(14.5,-120.127531126037,69.9330127018922));
#49418=CARTESIAN_POINT('Origin',(14.25,-119.911024775091,69.8080127018922));
#49419=CARTESIAN_POINT('',(14.,-119.670765314673,69.7241542943354));
#49420=CARTESIAN_POINT('',(14.,-119.670765314673,69.7241542943354));
#49421=CARTESIAN_POINT('',(14.,-119.694518424145,69.6830127018922));
#49422=CARTESIAN_POINT('Origin',(14.25,-117.286708727069,68.9225214538621));
#49423=CARTESIAN_POINT('',(14.5,-117.183872265404,69.1503912898478));
#49424=CARTESIAN_POINT('',(14.,-117.389545188734,68.6946516178765));
#49425=CARTESIAN_POINT('Origin',(14.,-116.213429510899,68.7124355652982));
#49426=CARTESIAN_POINT('Origin',(14.,-120.877531126037,68.6339745962156));
#49427=CARTESIAN_POINT('Origin',(57.5,-125.765473267224,59.1970922754756));
#49428=CARTESIAN_POINT('',(57.5,-125.08223311503,59.4850762228408));
#49429=CARTESIAN_POINT('',(58.,-125.292242378034,59.0288384007668));
#49430=CARTESIAN_POINT('',(57.5,-125.08223311503,59.4850762228408));
#49431=CARTESIAN_POINT('',(57.5,-125.765473267224,59.1970922754756));
#49432=CARTESIAN_POINT('',(57.5,-125.765473267224,59.1970922754756));
#49433=CARTESIAN_POINT('',(58.,-125.292242378034,59.0288384007668));
#49434=CARTESIAN_POINT('Origin',(57.5,-125.969521727281,57.5822796533797));
#49435=CARTESIAN_POINT('',(57.5,-126.188091528965,58.2907844884389));
#49436=CARTESIAN_POINT('',(58.,-125.755014631118,58.036420101407));
#49437=CARTESIAN_POINT('',(57.5,-126.188091528965,58.2907844884389));
#49438=CARTESIAN_POINT('',(57.5,-125.969521727281,57.5822796533797));
#49439=CARTESIAN_POINT('',(57.5,-125.969521727281,57.5822796533797));
#49440=CARTESIAN_POINT('',(58.,-125.755014631118,58.036420101407));
#49441=CARTESIAN_POINT('Origin',(14.,-125.292242378034,59.0288384007668));
#49442=CARTESIAN_POINT('',(14.5,-125.08223311503,59.4850762228408));
#49443=CARTESIAN_POINT('',(14.5,-125.765473267224,59.1970922754756));
#49444=CARTESIAN_POINT('',(14.5,-125.08223311503,59.4850762228408));
#49445=CARTESIAN_POINT('',(14.,-125.292242378034,59.0288384007668));
#49446=CARTESIAN_POINT('',(14.,-125.292242378034,59.0288384007668));
#49447=CARTESIAN_POINT('',(14.5,-125.765473267224,59.1970922754756));
#49448=CARTESIAN_POINT('Origin',(14.25,-122.84739093989,58.4380402379161));
#49449=CARTESIAN_POINT('',(14.,-122.929975912966,58.2020747272541));
#49450=CARTESIAN_POINT('',(14.5,-122.764805966813,58.674005748578));
#49451=CARTESIAN_POINT('Origin',(14.5,-125.969521727281,57.5822796533797));
#49452=CARTESIAN_POINT('',(14.,-125.755014631118,58.036420101407));
#49453=CARTESIAN_POINT('',(14.5,-126.188091528965,58.2907844884389));
#49454=CARTESIAN_POINT('',(14.,-125.755014631118,58.036420101407));
#49455=CARTESIAN_POINT('',(14.5,-125.969521727281,57.5822796533797));
#49456=CARTESIAN_POINT('',(14.5,-125.969521727281,57.5822796533797));
#49457=CARTESIAN_POINT('',(14.5,-126.188091528965,58.2907844884389));
#49458=CARTESIAN_POINT('Origin',(14.25,-125.459008691224,57.56981106276));
#49459=CARTESIAN_POINT('',(14.5,-125.586684161994,57.3548715964828));
#49460=CARTESIAN_POINT('',(14.,-125.331333220453,57.7847505290373));
#49461=CARTESIAN_POINT('Origin',(14.,-126.078806628123,57.9365320709093));
#49462=CARTESIAN_POINT('',(14.,-126.188091528965,58.2907844884389));
#49463=CARTESIAN_POINT('',(14.,-125.969521727281,57.5822796533797));
#49464=CARTESIAN_POINT('Origin',(14.25,-125.538896320465,59.0914377100404));
#49465=CARTESIAN_POINT('',(14.5,-125.765473267224,59.1970922754756));
#49466=CARTESIAN_POINT('',(14.,-125.312319373706,58.9857831446052));
#49467=CARTESIAN_POINT('Origin',(14.,-125.423853191127,59.3410842491582));
#49468=CARTESIAN_POINT('',(14.,-125.08223311503,59.4850762228408));
#49469=CARTESIAN_POINT('',(14.,-125.765473267224,59.1970922754756));
#49470=CARTESIAN_POINT('Origin',(57.75,-125.459008691224,57.56981106276));
#49471=CARTESIAN_POINT('',(58.,-125.331333220453,57.7847505290373));
#49472=CARTESIAN_POINT('',(57.5,-125.586684161994,57.3548715964828));
#49473=CARTESIAN_POINT('Origin',(57.75,-125.538896320465,59.0914377100404));
#49474=CARTESIAN_POINT('',(58.,-125.312319373706,58.9857831446052));
#49475=CARTESIAN_POINT('',(57.5,-125.765473267224,59.1970922754756));
#49476=CARTESIAN_POINT('Origin',(57.75,-122.84739093989,58.4380402379161));
#49477=CARTESIAN_POINT('',(57.5,-122.764805966813,58.674005748578));
#49478=CARTESIAN_POINT('',(58.,-122.929975912966,58.2020747272541));
#49479=CARTESIAN_POINT('Origin',(14.,-124.164166824021,57.8987018584758));
#49480=CARTESIAN_POINT('Origin',(14.,-121.759885683511,58.3222962368457));
#49481=CARTESIAN_POINT('Origin',(14.,-125.554164136354,59.6502461689939));
#49482=CARTESIAN_POINT('Origin',(57.5,-130.446264217578,48.0106462326609));
#49483=CARTESIAN_POINT('',(57.5,-129.790723455271,48.3570826171013));
#49484=CARTESIAN_POINT('',(58.,-129.960169823373,47.8842774043812));
#49485=CARTESIAN_POINT('',(57.5,-129.790723455271,48.3570826171013));
#49486=CARTESIAN_POINT('',(57.5,-130.446264217578,48.0106462326609));
#49487=CARTESIAN_POINT('',(57.5,-130.446264217578,48.0106462326609));
#49488=CARTESIAN_POINT('',(58.,-129.960169823373,47.8842774043812));
#49489=CARTESIAN_POINT('Origin',(57.5,-130.508796018164,46.3841944650247));
#49490=CARTESIAN_POINT('',(57.5,-130.788284360904,47.070953611875));
#49491=CARTESIAN_POINT('',(58.,-130.334686134323,46.8553022968291));
#49492=CARTESIAN_POINT('',(57.5,-130.788284360904,47.070953611875));
#49493=CARTESIAN_POINT('',(57.5,-130.508796018164,46.3841944650247));
#49494=CARTESIAN_POINT('',(57.5,-130.508796018164,46.3841944650247));
#49495=CARTESIAN_POINT('',(58.,-130.334686134323,46.8553022968291));
#49496=CARTESIAN_POINT('Origin',(14.,-129.960169823373,47.8842774043812));
#49497=CARTESIAN_POINT('',(14.5,-129.790723455271,48.3570826171013));
#49498=CARTESIAN_POINT('',(14.5,-130.446264217578,48.0106462326609));
#49499=CARTESIAN_POINT('',(14.5,-129.790723455271,48.3570826171013));
#49500=CARTESIAN_POINT('',(14.,-129.960169823373,47.8842774043812));
#49501=CARTESIAN_POINT('',(14.,-129.960169823373,47.8842774043812));
#49502=CARTESIAN_POINT('',(14.5,-130.446264217578,48.0106462326609));
#49503=CARTESIAN_POINT('Origin',(14.25,-127.473130330375,47.5088102499061));
#49504=CARTESIAN_POINT('',(14.,-127.534835293351,47.2665449045839));
#49505=CARTESIAN_POINT('',(14.5,-127.411425367399,47.7510755952283));
#49506=CARTESIAN_POINT('Origin',(14.5,-130.508796018164,46.3841944650247));
#49507=CARTESIAN_POINT('',(14.,-130.334686134323,46.8553022968291));
#49508=CARTESIAN_POINT('',(14.5,-130.788284360904,47.070953611875));
#49509=CARTESIAN_POINT('',(14.,-130.334686134323,46.8553022968291));
#49510=CARTESIAN_POINT('',(14.5,-130.508796018164,46.3841944650247));
#49511=CARTESIAN_POINT('',(14.5,-130.508796018164,46.3841944650247));
#49512=CARTESIAN_POINT('',(14.5,-130.788284360904,47.070953611875));
#49513=CARTESIAN_POINT('Origin',(14.25,-129.99913892906,46.4162674639966));
#49514=CARTESIAN_POINT('',(14.5,-130.107595347289,46.1910182567949));
#49515=CARTESIAN_POINT('',(14.,-129.890682510832,46.6415166711983));
#49516=CARTESIAN_POINT('Origin',(14.,-130.648540189534,46.7275740384498));
#49517=CARTESIAN_POINT('',(14.,-130.788284360904,47.070953611875));
#49518=CARTESIAN_POINT('',(14.,-130.508796018164,46.3841944650247));
#49519=CARTESIAN_POINT('Origin',(14.25,-130.211341062382,47.9251411968295));
#49520=CARTESIAN_POINT('',(14.5,-130.446264217578,48.0106462326609));
#49521=CARTESIAN_POINT('',(14.,-129.976417907185,47.8396361609981));
#49522=CARTESIAN_POINT('Origin',(14.,-130.118493836425,48.1838644248811));
#49523=CARTESIAN_POINT('',(14.,-129.790723455271,48.3570826171013));
#49524=CARTESIAN_POINT('',(14.,-130.446264217578,48.0106462326609));
#49525=CARTESIAN_POINT('Origin',(57.75,-129.99913892906,46.4162674639966));
#49526=CARTESIAN_POINT('',(58.,-129.890682510832,46.6415166711983));
#49527=CARTESIAN_POINT('',(57.5,-130.107595347289,46.1910182567949));
#49528=CARTESIAN_POINT('Origin',(57.75,-130.211341062382,47.9251411968295));
#49529=CARTESIAN_POINT('',(58.,-129.976417907185,47.8396361609981));
#49530=CARTESIAN_POINT('',(57.5,-130.446264217578,48.0106462326609));
#49531=CARTESIAN_POINT('Origin',(57.75,-127.473130330375,47.5088102499061));
#49532=CARTESIAN_POINT('',(57.5,-127.411425367399,47.7510755952283));
#49533=CARTESIAN_POINT('',(58.,-127.534835293351,47.2665449045839));
#49534=CARTESIAN_POINT('Origin',(14.,-128.737889047669,46.8567596356166));
#49535=CARTESIAN_POINT('Origin',(14.,-126.379675605442,47.4882890180656));
#49536=CARTESIAN_POINT('Origin',(14.,-130.275254145916,48.4804925430539));
#49537=CARTESIAN_POINT('Origin',(57.75,-131.128722228666,36.2180095292903));
#49538=CARTESIAN_POINT('',(57.7487592975525,-133.822854175933,36.6599362981178));
#49539=CARTESIAN_POINT('',(58.,-133.639021904261,36.375288143631));
#49540=CARTESIAN_POINT('',(58.2319907935076,-133.469274748797,36.1124495566242));
#49541=CARTESIAN_POINT('',(58.,-131.169077569515,35.9712881348696));
#49542=CARTESIAN_POINT('',(57.5,-133.511428020236,36.8610624138407));
#49543=CARTESIAN_POINT('',(57.5,-131.088366887817,36.4647309237111));
#49544=CARTESIAN_POINT('',(50.4896657310026,-124.735066802703,42.5290366978776));
#49545=CARTESIAN_POINT('Origin',(58.,-132.331838201602,35.4582091790453));
#49546=CARTESIAN_POINT('',(58.,-133.922431977811,35.3175873497673));
#49547=CARTESIAN_POINT('',(58.,-133.651317418485,36.3294006598437));
#49548=CARTESIAN_POINT('',(58.,-133.461485277164,35.1433127085737));
#49549=CARTESIAN_POINT('Origin',(57.75,-133.892798875057,36.3941054211193));
#49550=CARTESIAN_POINT('',(57.5,-134.134280331629,36.4588101823949));
#49551=CARTESIAN_POINT('',(57.5,-134.134280331629,36.4588101823949));
#49552=CARTESIAN_POINT('',(57.5,-134.393099376732,35.4928843561059));
#49553=CARTESIAN_POINT('',(57.5,-134.134280331629,36.4588101823949));
#49554=CARTESIAN_POINT('',(57.5,-134.393099376732,35.4928843561059));
#49555=CARTESIAN_POINT('Origin',(14.,-133.822854175933,36.6599362981178));
#49556=CARTESIAN_POINT('',(14.5,-133.511428020236,36.8610624138407));
#49557=CARTESIAN_POINT('',(14.,-133.511428020236,36.8610624138407));
#49558=CARTESIAN_POINT('',(14.5,-134.134280331629,36.4588101823949));
#49559=CARTESIAN_POINT('',(14.5,-133.511428020236,36.8610624138407));
#49560=CARTESIAN_POINT('',(14.,-134.134280331629,36.4588101823949));
#49561=CARTESIAN_POINT('Origin',(57.5,-134.054819567983,34.8330975492484));
#49562=CARTESIAN_POINT('',(57.5,-134.054819567983,34.8330975492484));
#49563=CARTESIAN_POINT('',(57.5,-134.054819567983,34.8330975492484));
#49564=CARTESIAN_POINT('',(58.,-133.922431977811,35.3175873497673));
#49565=CARTESIAN_POINT('Origin',(14.,-133.639021904261,36.375288143631));
#49566=CARTESIAN_POINT('',(14.,-133.639021904261,36.375288143631));
#49567=CARTESIAN_POINT('',(14.,-133.639021904261,36.375288143631));
#49568=CARTESIAN_POINT('',(14.5,-134.134280331629,36.4588101823949));
#49569=CARTESIAN_POINT('Origin',(14.25,-131.128722228666,36.2180095292903));
#49570=CARTESIAN_POINT('',(14.,-131.169077569515,35.9712881348696));
#49571=CARTESIAN_POINT('',(14.5,-131.088366887817,36.4647309237111));
#49572=CARTESIAN_POINT('Origin',(14.5,-134.054819567983,34.8330975492484));
#49573=CARTESIAN_POINT('',(14.,-133.922431977811,35.3175873497673));
#49574=CARTESIAN_POINT('',(14.5,-134.393099376732,35.4928843561059));
#49575=CARTESIAN_POINT('',(14.,-133.922431977811,35.3175873497673));
#49576=CARTESIAN_POINT('',(14.5,-134.054819567983,34.8330975492484));
#49577=CARTESIAN_POINT('',(14.5,-134.054819567983,34.8330975492484));
#49578=CARTESIAN_POINT('',(14.5,-134.393099376732,35.4928843561059));
#49579=CARTESIAN_POINT('Origin',(14.25,-133.549897224021,34.9094680429235));
#49580=CARTESIAN_POINT('',(14.5,-133.638309170877,34.6756233772733));
#49581=CARTESIAN_POINT('',(14.,-133.461485277164,35.1433127085737));
#49582=CARTESIAN_POINT('Origin',(14.,-134.223959472357,35.1629909526771));
#49583=CARTESIAN_POINT('',(14.,-134.393099376732,35.4928843561059));
#49584=CARTESIAN_POINT('',(14.,-134.054819567983,34.8330975492484));
#49585=CARTESIAN_POINT('Origin',(14.25,-133.892798875057,36.3941054211193));
#49586=CARTESIAN_POINT('',(14.5,-134.134280331629,36.4588101823949));
#49587=CARTESIAN_POINT('',(14.,-133.651317418485,36.3294006598437));
#49588=CARTESIAN_POINT('Origin',(57.75,-133.549897224021,34.9094680429235));
#49589=CARTESIAN_POINT('',(57.5,-133.638309170877,34.6756233772733));
#49590=CARTESIAN_POINT('Origin',(14.,-130.037639885881,36.292867245645));
#49591=CARTESIAN_POINT('Origin',(14.,-134.004870809078,36.9417730955394));
#49592=CARTESIAN_POINT('Origin',(57.5,-136.801453579863,24.6295005722094));
#49593=CARTESIAN_POINT('',(57.5,-136.216030001563,25.0845072682929));
#49594=CARTESIAN_POINT('',(58.,-136.30080033501,24.5894609761083));
#49595=CARTESIAN_POINT('',(57.5,-136.216030001563,25.0845072682929));
#49596=CARTESIAN_POINT('',(57.5,-136.801453579863,24.6295005722094));
#49597=CARTESIAN_POINT('',(57.5,-136.801453579863,24.6295005722094));
#49598=CARTESIAN_POINT('',(58.,-136.30080033501,24.5894609761083));
#49599=CARTESIAN_POINT('Origin',(57.5,-136.580604996376,23.016899728323));
#49600=CARTESIAN_POINT('',(57.5,-136.97510175753,23.6446928191972));
#49601=CARTESIAN_POINT('',(58.,-136.490947249372,23.5110842376315));
#49602=CARTESIAN_POINT('',(57.5,-136.97510175753,23.6446928191972));
#49603=CARTESIAN_POINT('',(57.5,-136.580604996376,23.016899728323));
#49604=CARTESIAN_POINT('',(57.5,-136.580604996376,23.016899728323));
#49605=CARTESIAN_POINT('',(58.,-136.490947249372,23.5110842376315));
#49606=CARTESIAN_POINT('Origin',(14.,-136.30080033501,24.5894609761083));
#49607=CARTESIAN_POINT('',(14.5,-136.216030001563,25.0845072682929));
#49608=CARTESIAN_POINT('',(14.5,-136.801453579863,24.6295005722094));
#49609=CARTESIAN_POINT('',(14.5,-136.216030001563,25.0845072682929));
#49610=CARTESIAN_POINT('',(14.,-136.30080033501,24.5894609761083));
#49611=CARTESIAN_POINT('',(14.,-136.30080033501,24.5894609761083));
#49612=CARTESIAN_POINT('',(14.5,-136.801453579863,24.6295005722094));
#49613=CARTESIAN_POINT('Origin',(14.25,-133.786345373109,24.6515678871246));
#49614=CARTESIAN_POINT('',(14.,-133.805043963321,24.4022681423913));
#49615=CARTESIAN_POINT('',(14.5,-133.767646782898,24.900867631858));
#49616=CARTESIAN_POINT('Origin',(14.5,-136.580604996376,23.016899728323));
#49617=CARTESIAN_POINT('',(14.,-136.490947249372,23.5110842376315));
#49618=CARTESIAN_POINT('',(14.5,-136.97510175753,23.6446928191972));
#49619=CARTESIAN_POINT('',(14.,-136.490947249372,23.5110842376315));
#49620=CARTESIAN_POINT('',(14.5,-136.580604996376,23.016899728323));
#49621=CARTESIAN_POINT('',(14.5,-136.580604996376,23.016899728323));
#49622=CARTESIAN_POINT('',(14.5,-136.97510175753,23.6446928191972));
#49623=CARTESIAN_POINT('Origin',(14.25,-136.084260161474,23.1369864911307));
#49624=CARTESIAN_POINT('',(14.5,-136.151954768658,22.8963260661369));
#49625=CARTESIAN_POINT('',(14.,-136.01656555429,23.3776469161245));
#49626=CARTESIAN_POINT('Origin',(14.,-136.777853376953,23.3307962737601));
#49627=CARTESIAN_POINT('',(14.,-136.97510175753,23.6446928191972));
#49628=CARTESIAN_POINT('',(14.,-136.580604996376,23.016899728323));
#49629=CARTESIAN_POINT('Origin',(14.25,-136.55525164161,24.5860885277927));
#49630=CARTESIAN_POINT('',(14.5,-136.801453579863,24.6295005722094));
#49631=CARTESIAN_POINT('',(14.,-136.309049703357,24.542676483376));
#49632=CARTESIAN_POINT('Origin',(14.,-136.508741790713,24.8570039202512));
#49633=CARTESIAN_POINT('',(14.,-136.216030001563,25.0845072682929));
#49634=CARTESIAN_POINT('',(14.,-136.801453579863,24.6295005722094));
#49635=CARTESIAN_POINT('Origin',(57.75,-136.084260161474,23.1369864911307));
#49636=CARTESIAN_POINT('',(58.,-136.01656555429,23.3776469161245));
#49637=CARTESIAN_POINT('',(57.5,-136.151954768658,22.8963260661369));
#49638=CARTESIAN_POINT('Origin',(57.75,-136.55525164161,24.5860885277927));
#49639=CARTESIAN_POINT('',(58.,-136.309049703357,24.542676483376));
#49640=CARTESIAN_POINT('',(57.5,-136.801453579863,24.6295005722094));
#49641=CARTESIAN_POINT('Origin',(57.75,-133.786345373109,24.6515678871246));
#49642=CARTESIAN_POINT('',(57.5,-133.767646782898,24.900867631858));
#49643=CARTESIAN_POINT('',(58.,-133.805043963321,24.4022681423913));
#49644=CARTESIAN_POINT('Origin',(14.,-134.918662162673,23.7898003403695));
#49645=CARTESIAN_POINT('Origin',(14.,-132.705939207914,24.8212348392527));
#49646=CARTESIAN_POINT('Origin',(14.,-136.71462949103,25.1219044487155));
#49647=CARTESIAN_POINT('Origin',(57.5,-138.066929551123,11.0255294024811));
#49648=CARTESIAN_POINT('',(57.5,-138.514640906126,11.6165508928786));
#49649=CARTESIAN_POINT('',(58.,-138.020683996878,11.5256475780665));
#49650=CARTESIAN_POINT('',(57.5,-138.514640906126,11.6165508928786));
#49651=CARTESIAN_POINT('',(57.5,-138.066929551123,11.0255294024811));
#49652=CARTESIAN_POINT('',(57.5,-138.066929551123,11.0255294024811));
#49653=CARTESIAN_POINT('',(58.,-138.020683996878,11.5256475780665));
#49654=CARTESIAN_POINT('Origin',(14.,-138.290785228625,11.3210401476799));
#49655=CARTESIAN_POINT('',(14.2512407024475,-138.290785228625,11.3210401476798));
#49656=CARTESIAN_POINT('',(14.5,-138.066929551123,11.0255294024811));
#49657=CARTESIAN_POINT('',(14.3353834448875,-138.215066126661,11.22108374498));
#49658=CARTESIAN_POINT('',(14.,-138.066929551123,11.0255294024811));
#49659=CARTESIAN_POINT('',(14.5,-138.514640906126,11.6165508928786));
#49660=CARTESIAN_POINT('',(14.,-138.514640906126,11.6165508928786));
#49661=CARTESIAN_POINT('',(14.4305329766294,-138.452128317718,11.5340283417823));
#49662=CARTESIAN_POINT('Origin',(57.75,-137.582939709175,11.188418501646));
#49663=CARTESIAN_POINT('',(58.,-137.536477638499,11.4340631148345));
#49664=CARTESIAN_POINT('',(57.5,-137.629401779851,10.9427738884575));
#49665=CARTESIAN_POINT('Origin',(57.5,-138.427485163379,12.6127455909704));
#49666=CARTESIAN_POINT('',(57.5,-137.883945745091,13.1170438759937));
#49667=CARTESIAN_POINT('',(58.,-137.925247374536,12.6164931630349));
#49668=CARTESIAN_POINT('',(57.5,-137.883945745091,13.1170438759937));
#49669=CARTESIAN_POINT('',(57.5,-138.427485163379,12.6127455909704));
#49670=CARTESIAN_POINT('',(57.5,-138.427485163379,12.6127455909704));
#49671=CARTESIAN_POINT('',(58.,-137.925247374536,12.6164931630349));
#49672=CARTESIAN_POINT('Origin',(14.,-138.155715454235,12.864894733482));
#49673=CARTESIAN_POINT('',(14.2512407024475,-138.155715454235,12.864894733482));
#49674=CARTESIAN_POINT('',(14.5,-138.427485163379,12.6127455909704));
#49675=CARTESIAN_POINT('',(14.2590041943422,-138.16419707464,12.8570254484205));
#49676=CARTESIAN_POINT('',(14.,-138.427485163379,12.6127455909704));
#49677=CARTESIAN_POINT('',(14.5,-137.883945745091,13.1170438759937));
#49678=CARTESIAN_POINT('',(14.,-137.883945745091,13.1170438759937));
#49679=CARTESIAN_POINT('',(14.6801520303733,-137.687129524037,13.2996508395415));
#49680=CARTESIAN_POINT('Origin',(57.75,-138.178436488856,12.5909566552835));
#49681=CARTESIAN_POINT('',(58.,-137.929387814333,12.5691677195966));
#49682=CARTESIAN_POINT('',(57.5,-138.427485163379,12.6127455909704));
#49683=CARTESIAN_POINT('Origin',(57.75,-135.425773646859,12.8975129283142));
#49684=CARTESIAN_POINT('',(57.5,-135.428874114848,13.1474937017714));
#49685=CARTESIAN_POINT('',(58.,-135.422673178871,12.647532154857));
#49686=CARTESIAN_POINT('Origin',(14.25,-137.582939709175,11.188418501646));
#49687=CARTESIAN_POINT('',(14.,-138.020683996878,11.5256475780665));
#49688=CARTESIAN_POINT('',(14.5,-138.5582187775,11.1184535438328));
#49689=CARTESIAN_POINT('',(14.,-137.536477638499,11.4340631148345));
#49690=CARTESIAN_POINT('',(14.5,-137.629401779851,10.9427738884575));
#49691=CARTESIAN_POINT('Origin',(14.,-138.383907292005,13.1108429400163));
#49692=CARTESIAN_POINT('',(14.5,-138.427485163379,12.6127455909704));
#49693=CARTESIAN_POINT('Origin',(14.25,-138.178436488856,12.5909566552835));
#49694=CARTESIAN_POINT('',(14.,-137.925247374536,12.6164931630349));
#49695=CARTESIAN_POINT('',(14.,-137.925247374536,12.6164931630349));
#49696=CARTESIAN_POINT('',(14.,-137.929387814333,12.5691677195966));
#49697=CARTESIAN_POINT('Origin',(14.25,-135.425773646859,12.8975129283142));
#49698=CARTESIAN_POINT('',(14.5,-135.428874114848,13.1474937017714));
#49699=CARTESIAN_POINT('',(14.,-135.422673178871,12.647532154857));
#49700=CARTESIAN_POINT('Origin',(14.,-134.364266202539,13.1606978482623));
#49701=CARTESIAN_POINT('Origin',(14.,-138.5582187775,11.1184535438328));
#49702=CARTESIAN_POINT('Origin',(57.5,-139.,0.500000000000008));
#49703=CARTESIAN_POINT('',(57.5,-138.502481404895,1.04975185951051));
#49704=CARTESIAN_POINT('',(58.,-138.5,0.547506218943965));
#49705=CARTESIAN_POINT('',(57.5,-138.502481404895,1.04975185951051));
#49706=CARTESIAN_POINT('',(57.5,-139.,0.500000000000008));
#49707=CARTESIAN_POINT('',(57.5,-139.,0.500000000000008));
#49708=CARTESIAN_POINT('',(58.,-138.5,0.547506218943965));
#49709=CARTESIAN_POINT('Origin',(57.5,-138.502481404895,-1.04975185951049));
#49710=CARTESIAN_POINT('',(57.5,-139.,-0.499999999999992));
#49711=CARTESIAN_POINT('',(58.,-138.5,-0.547506218943948));
#49712=CARTESIAN_POINT('',(57.5,-139.,-0.499999999999992));
#49713=CARTESIAN_POINT('',(57.5,-138.502481404895,-1.04975185951049));
#49714=CARTESIAN_POINT('',(57.5,-138.502481404895,-1.04975185951049));
#49715=CARTESIAN_POINT('',(58.,-138.5,-0.547506218943948));
#49716=CARTESIAN_POINT('Origin',(14.,-138.5,0.547506218943967));
#49717=CARTESIAN_POINT('',(14.5,-138.502481404895,1.04975185951051));
#49718=CARTESIAN_POINT('',(14.5,-139.,0.500000000000008));
#49719=CARTESIAN_POINT('',(14.5,-138.502481404895,1.04975185951051));
#49720=CARTESIAN_POINT('',(14.,-138.5,0.547506218943967));
#49721=CARTESIAN_POINT('',(14.,-138.5,0.547506218943967));
#49722=CARTESIAN_POINT('',(14.5,-139.,0.500000000000008));
#49723=CARTESIAN_POINT('Origin',(14.25,-136.034530010839,1.0453001083881));
#49724=CARTESIAN_POINT('',(14.,-136.009654081084,0.796540810835608));
#49725=CARTESIAN_POINT('',(14.5,-136.059405940594,1.2940594059406));
#49726=CARTESIAN_POINT('Origin',(14.5,-138.502481404895,-1.04975185951049));
#49727=CARTESIAN_POINT('',(14.,-138.5,-0.547506218943949));
#49728=CARTESIAN_POINT('',(14.5,-139.,-0.499999999999992));
#49729=CARTESIAN_POINT('',(14.,-138.5,-0.547506218943949));
#49730=CARTESIAN_POINT('',(14.5,-138.502481404895,-1.04975185951049));
#49731=CARTESIAN_POINT('',(14.5,-138.502481404895,-1.04975185951049));
#49732=CARTESIAN_POINT('',(14.5,-139.,-0.499999999999992));
#49733=CARTESIAN_POINT('Origin',(14.25,-138.034530010839,-0.845300108388089));
#49734=CARTESIAN_POINT('',(14.5,-138.059405940594,-1.09405940594059));
#49735=CARTESIAN_POINT('',(14.,-138.009654081084,-0.596540810835591));
#49736=CARTESIAN_POINT('Origin',(14.,-138.751240702448,-0.774875929755241));
#49737=CARTESIAN_POINT('',(14.,-139.,-0.499999999999992));
#49738=CARTESIAN_POINT('',(14.,-138.502481404895,-1.04975185951049));
#49739=CARTESIAN_POINT('Origin',(14.25,-138.75,0.500000000000008));
#49740=CARTESIAN_POINT('',(14.5,-139.,0.500000000000008));
#49741=CARTESIAN_POINT('',(14.,-138.5,0.500000000000008));
#49742=CARTESIAN_POINT('Origin',(14.,-138.751240702448,0.774875929755257));
#49743=CARTESIAN_POINT('',(14.,-138.502481404895,1.04975185951051));
#49744=CARTESIAN_POINT('',(14.,-139.,0.500000000000008));
#49745=CARTESIAN_POINT('Origin',(57.75,-138.034530010839,-0.845300108388089));
#49746=CARTESIAN_POINT('',(58.,-138.009654081084,-0.596540810835592));
#49747=CARTESIAN_POINT('',(57.5,-138.059405940594,-1.09405940594059));
#49748=CARTESIAN_POINT('Origin',(57.75,-138.75,0.500000000000008));
#49749=CARTESIAN_POINT('',(58.,-138.5,0.500000000000008));
#49750=CARTESIAN_POINT('',(57.5,-139.,0.500000000000008));
#49751=CARTESIAN_POINT('Origin',(57.75,-136.034530010839,1.0453001083881));
#49752=CARTESIAN_POINT('',(57.5,-136.059405940594,1.2940594059406));
#49753=CARTESIAN_POINT('',(58.,-136.009654081084,0.796540810835608));
#49754=CARTESIAN_POINT('Origin',(14.,-137.,8.38883057415937E-15));
#49755=CARTESIAN_POINT('Origin',(14.,-135.,1.40000000000001));
#49756=CARTESIAN_POINT('Origin',(14.,-139.,1.00000000000001));
#49757=CARTESIAN_POINT('Origin',(57.5,-138.514640906126,-11.6165508928786));
#49758=CARTESIAN_POINT('',(57.5,-138.066929551123,-11.025529402481));
#49759=CARTESIAN_POINT('',(58.,-138.020683996878,-11.5256475780664));
#49760=CARTESIAN_POINT('',(57.5,-138.066929551123,-11.025529402481));
#49761=CARTESIAN_POINT('',(57.5,-138.514640906126,-11.6165508928786));
#49762=CARTESIAN_POINT('',(57.5,-138.514640906126,-11.6165508928786));
#49763=CARTESIAN_POINT('',(58.,-138.020683996878,-11.5256475780664));
#49764=CARTESIAN_POINT('Origin',(57.5,-137.883945745091,-13.1170438759936));
#49765=CARTESIAN_POINT('',(57.5,-138.427485163379,-12.6127455909703));
#49766=CARTESIAN_POINT('',(58.,-137.925247374536,-12.6164931630349));
#49767=CARTESIAN_POINT('',(57.5,-138.427485163379,-12.6127455909703));
#49768=CARTESIAN_POINT('',(57.5,-137.883945745091,-13.1170438759936));
#49769=CARTESIAN_POINT('',(57.5,-137.883945745091,-13.1170438759936));
#49770=CARTESIAN_POINT('',(58.,-137.925247374536,-12.6164931630349));
#49771=CARTESIAN_POINT('Origin',(14.,-138.020683996878,-11.5256475780664));
#49772=CARTESIAN_POINT('',(14.5,-138.066929551123,-11.025529402481));
#49773=CARTESIAN_POINT('',(14.5,-138.514640906126,-11.6165508928786));
#49774=CARTESIAN_POINT('',(14.5,-138.066929551123,-11.025529402481));
#49775=CARTESIAN_POINT('',(14.,-138.020683996878,-11.5256475780664));
#49776=CARTESIAN_POINT('',(14.,-138.020683996878,-11.5256475780664));
#49777=CARTESIAN_POINT('',(14.5,-138.514640906126,-11.6165508928786));
#49778=CARTESIAN_POINT('Origin',(14.25,-135.607981461541,-10.8148680765323));
#49779=CARTESIAN_POINT('',(14.,-135.561519390865,-11.0605126897207));
#49780=CARTESIAN_POINT('',(14.5,-135.654443532217,-10.5692234633438));
#49781=CARTESIAN_POINT('Origin',(14.5,-137.883945745091,-13.1170438759936));
#49782=CARTESIAN_POINT('',(14.,-137.925247374536,-12.6164931630349));
#49783=CARTESIAN_POINT('',(14.5,-138.427485163379,-12.6127455909703));
#49784=CARTESIAN_POINT('',(14.,-137.925247374536,-12.6164931630349));
#49785=CARTESIAN_POINT('',(14.5,-137.883945745091,-13.1170438759936));
#49786=CARTESIAN_POINT('',(14.5,-137.883945745091,-13.1170438759936));
#49787=CARTESIAN_POINT('',(14.5,-138.427485163379,-12.6127455909703));
#49788=CARTESIAN_POINT('Origin',(14.25,-137.435594191592,-12.8725854741911));
#49789=CARTESIAN_POINT('',(14.5,-137.438694659581,-13.1225662476483));
#49790=CARTESIAN_POINT('',(14.,-137.432493723604,-12.622604700734));
#49791=CARTESIAN_POINT('Origin',(14.,-138.155715454235,-12.864894733482));
#49792=CARTESIAN_POINT('',(14.,-138.427485163379,-12.6127455909703));
#49793=CARTESIAN_POINT('',(14.,-137.883945745091,-13.1170438759936));
#49794=CARTESIAN_POINT('Origin',(14.25,-138.265592231604,-11.5947619571917));
#49795=CARTESIAN_POINT('',(14.5,-138.514640906126,-11.6165508928786));
#49796=CARTESIAN_POINT('',(14.,-138.016543557081,-11.5729730215048));
#49797=CARTESIAN_POINT('Origin',(14.,-138.290785228625,-11.3210401476798));
#49798=CARTESIAN_POINT('',(14.,-138.066929551123,-11.025529402481));
#49799=CARTESIAN_POINT('',(14.,-138.514640906126,-11.6165508928786));
#49800=CARTESIAN_POINT('Origin',(57.75,-137.435594191592,-12.8725854741911));
#49801=CARTESIAN_POINT('',(58.,-137.432493723604,-12.622604700734));
#49802=CARTESIAN_POINT('',(57.5,-137.438694659581,-13.1225662476483));
#49803=CARTESIAN_POINT('Origin',(57.75,-138.265592231604,-11.5947619571917));
#49804=CARTESIAN_POINT('',(58.,-138.016543557081,-11.5729730215048));
#49805=CARTESIAN_POINT('',(57.5,-138.514640906126,-11.6165508928786));
#49806=CARTESIAN_POINT('Origin',(57.75,-135.607981461541,-10.8148680765323));
#49807=CARTESIAN_POINT('',(57.5,-135.654443532217,-10.5692234633438));
#49808=CARTESIAN_POINT('',(58.,-135.561519390865,-11.0605126897207));
#49809=CARTESIAN_POINT('Origin',(14.,-136.478673638569,-11.9403367564291));
#49810=CARTESIAN_POINT('Origin',(14.,-134.608302282232,-10.3713526936054));
#49811=CARTESIAN_POINT('Origin',(14.,-138.5582187775,-11.1184535438327));
#49812=CARTESIAN_POINT('Origin',(57.75,-134.149374290983,-22.5927285851944));
#49813=CARTESIAN_POINT('',(57.7487592975525,-136.777853376953,-23.3307962737601));
#49814=CARTESIAN_POINT('',(58.,-136.490947249372,-23.5110842376314));
#49815=CARTESIAN_POINT('',(58.2319907935076,-136.226023693788,-23.6775586479915));
#49816=CARTESIAN_POINT('',(58.,-134.081679683799,-22.8333890101882));
#49817=CARTESIAN_POINT('',(57.5,-136.580604996376,-23.016899728323));
#49818=CARTESIAN_POINT('',(57.5,-134.217068898167,-22.3520681602006));
#49819=CARTESIAN_POINT('',(50.4896657310027,-131.02190992259,-14.1709199758145));
#49820=CARTESIAN_POINT('Origin',(58.,-134.918662162673,-23.7898003403695));
#49821=CARTESIAN_POINT('',(58.,-136.30080033501,-24.5894609761083));
#49822=CARTESIAN_POINT('',(58.,-136.482697881024,-23.5578687303638));
#49823=CARTESIAN_POINT('',(58.,-135.809389104878,-24.5526029471227));
#49824=CARTESIAN_POINT('Origin',(57.75,-136.728899819277,-23.6012807747805));
#49825=CARTESIAN_POINT('',(57.5,-136.97510175753,-23.6446928191972));
#49826=CARTESIAN_POINT('',(57.5,-136.97510175753,-23.6446928191972));
#49827=CARTESIAN_POINT('',(57.5,-136.801453579863,-24.6295005722094));
#49828=CARTESIAN_POINT('',(57.5,-136.97510175753,-23.6446928191972));
#49829=CARTESIAN_POINT('',(57.5,-136.801453579863,-24.6295005722094));
#49830=CARTESIAN_POINT('Origin',(14.,-136.777853376953,-23.3307962737601));
#49831=CARTESIAN_POINT('',(14.5,-136.580604996376,-23.016899728323));
#49832=CARTESIAN_POINT('',(14.,-136.580604996376,-23.016899728323));
#49833=CARTESIAN_POINT('',(14.5,-136.97510175753,-23.6446928191972));
#49834=CARTESIAN_POINT('',(14.5,-136.580604996376,-23.016899728323));
#49835=CARTESIAN_POINT('',(14.,-136.97510175753,-23.6446928191972));
#49836=CARTESIAN_POINT('Origin',(57.5,-136.216030001563,-25.0845072682928));
#49837=CARTESIAN_POINT('',(57.5,-136.216030001563,-25.0845072682928));
#49838=CARTESIAN_POINT('',(57.5,-136.216030001563,-25.0845072682928));
#49839=CARTESIAN_POINT('',(58.,-136.30080033501,-24.5894609761083));
#49840=CARTESIAN_POINT('Origin',(14.,-136.490947249372,-23.5110842376314));
#49841=CARTESIAN_POINT('',(14.,-136.490947249372,-23.5110842376314));
#49842=CARTESIAN_POINT('',(14.,-136.490947249372,-23.5110842376314));
#49843=CARTESIAN_POINT('',(14.5,-136.97510175753,-23.6446928191972));
#49844=CARTESIAN_POINT('Origin',(14.25,-134.149374290983,-22.5927285851944));
#49845=CARTESIAN_POINT('',(14.,-134.081679683799,-22.8333890101882));
#49846=CARTESIAN_POINT('',(14.5,-134.217068898167,-22.3520681602006));
#49847=CARTESIAN_POINT('Origin',(14.5,-136.216030001563,-25.0845072682928));
#49848=CARTESIAN_POINT('',(14.,-136.30080033501,-24.5894609761083));
#49849=CARTESIAN_POINT('',(14.5,-136.801453579863,-24.6295005722094));
#49850=CARTESIAN_POINT('',(14.,-136.30080033501,-24.5894609761083));
#49851=CARTESIAN_POINT('',(14.5,-136.216030001563,-25.0845072682928));
#49852=CARTESIAN_POINT('',(14.5,-136.216030001563,-25.0845072682928));
#49853=CARTESIAN_POINT('',(14.5,-136.801453579863,-24.6295005722094));
#49854=CARTESIAN_POINT('Origin',(14.25,-135.790690514667,-24.801902691856));
#49855=CARTESIAN_POINT('',(14.5,-135.771991924456,-25.0512024365894));
#49856=CARTESIAN_POINT('',(14.,-135.809389104878,-24.5526029471227));
#49857=CARTESIAN_POINT('Origin',(14.,-136.508741790713,-24.8570039202511));
#49858=CARTESIAN_POINT('',(14.,-136.801453579863,-24.6295005722094));
#49859=CARTESIAN_POINT('',(14.,-136.216030001563,-25.0845072682928));
#49860=CARTESIAN_POINT('Origin',(14.25,-136.728899819277,-23.6012807747805));
#49861=CARTESIAN_POINT('',(14.5,-136.97510175753,-23.6446928191972));
#49862=CARTESIAN_POINT('',(14.,-136.482697881024,-23.5578687303637));
#49863=CARTESIAN_POINT('Origin',(57.75,-135.790690514667,-24.801902691856));
#49864=CARTESIAN_POINT('',(57.5,-135.771991924456,-25.0512024365894));
#49865=CARTESIAN_POINT('Origin',(14.,-133.192154105382,-22.0637731308185));
#49866=CARTESIAN_POINT('Origin',(14.,-137.061925846364,-23.1522889426911));
#49867=CARTESIAN_POINT('Origin',(57.5,-134.393099376732,-35.4928843561058));
#49868=CARTESIAN_POINT('',(57.5,-134.054819567983,-34.8330975492484));
#49869=CARTESIAN_POINT('',(58.,-133.922431977811,-35.3175873497673));
#49870=CARTESIAN_POINT('',(57.5,-134.054819567983,-34.8330975492484));
#49871=CARTESIAN_POINT('',(57.5,-134.393099376732,-35.4928843561058));
#49872=CARTESIAN_POINT('',(57.5,-134.393099376732,-35.4928843561058));
#49873=CARTESIAN_POINT('',(58.,-133.922431977811,-35.3175873497673));
#49874=CARTESIAN_POINT('Origin',(57.5,-133.511428020236,-36.8610624138407));
#49875=CARTESIAN_POINT('',(57.5,-134.134280331629,-36.4588101823949));
#49876=CARTESIAN_POINT('',(58.,-133.639021904261,-36.375288143631));
#49877=CARTESIAN_POINT('',(57.5,-134.134280331629,-36.4588101823949));
#49878=CARTESIAN_POINT('',(57.5,-133.511428020236,-36.8610624138407));
#49879=CARTESIAN_POINT('',(57.5,-133.511428020236,-36.8610624138407));
#49880=CARTESIAN_POINT('',(58.,-133.639021904261,-36.375288143631));
#49881=CARTESIAN_POINT('Origin',(14.,-133.922431977811,-35.3175873497673));
#49882=CARTESIAN_POINT('',(14.5,-134.054819567983,-34.8330975492484));
#49883=CARTESIAN_POINT('',(14.5,-134.393099376732,-35.4928843561058));
#49884=CARTESIAN_POINT('',(14.5,-134.054819567983,-34.8330975492484));
#49885=CARTESIAN_POINT('',(14.,-133.922431977811,-35.3175873497673));
#49886=CARTESIAN_POINT('',(14.,-133.922431977811,-35.3175873497673));
#49887=CARTESIAN_POINT('',(14.5,-134.393099376732,-35.4928843561058));
#49888=CARTESIAN_POINT('Origin',(14.25,-131.669809380463,-34.1986447874607));
#49889=CARTESIAN_POINT('',(14.,-131.581397433607,-34.4324894531108));
#49890=CARTESIAN_POINT('',(14.5,-131.75822132732,-33.9648001218105));
#49891=CARTESIAN_POINT('Origin',(14.5,-133.511428020236,-36.8610624138407));
#49892=CARTESIAN_POINT('',(14.,-133.639021904261,-36.3752881436309));
#49893=CARTESIAN_POINT('',(14.5,-134.134280331629,-36.4588101823949));
#49894=CARTESIAN_POINT('',(14.,-133.639021904261,-36.3752881436309));
#49895=CARTESIAN_POINT('',(14.5,-133.511428020236,-36.8610624138407));
#49896=CARTESIAN_POINT('',(14.5,-133.511428020236,-36.8610624138407));
#49897=CARTESIAN_POINT('',(14.5,-134.134280331629,-36.4588101823949));
#49898=CARTESIAN_POINT('Origin',(14.25,-133.112337690265,-36.5424624542375));
#49899=CARTESIAN_POINT('',(14.5,-133.071982349415,-36.7891838486583));
#49900=CARTESIAN_POINT('',(14.,-133.152693031114,-36.2957410598168));
#49901=CARTESIAN_POINT('Origin',(14.,-133.822854175933,-36.6599362981178));
#49902=CARTESIAN_POINT('',(14.,-134.134280331629,-36.4588101823949));
#49903=CARTESIAN_POINT('',(14.,-133.511428020236,-36.8610624138407));
#49904=CARTESIAN_POINT('Origin',(14.25,-134.151617920159,-35.4281795948302));
#49905=CARTESIAN_POINT('',(14.5,-134.393099376732,-35.4928843561058));
#49906=CARTESIAN_POINT('',(14.,-133.910136463587,-35.3634748335546));
#49907=CARTESIAN_POINT('Origin',(14.,-134.223959472357,-35.1629909526771));
#49908=CARTESIAN_POINT('',(14.,-134.054819567983,-34.8330975492484));
#49909=CARTESIAN_POINT('',(14.,-134.393099376732,-35.4928843561058));
#49910=CARTESIAN_POINT('Origin',(57.75,-133.112337690265,-36.5424624542375));
#49911=CARTESIAN_POINT('',(58.,-133.152693031114,-36.2957410598168));
#49912=CARTESIAN_POINT('',(57.5,-133.071982349415,-36.7891838486583));
#49913=CARTESIAN_POINT('Origin',(57.75,-134.151617920159,-35.4281795948302));
#49914=CARTESIAN_POINT('',(58.,-133.910136463587,-35.3634748335546));
#49915=CARTESIAN_POINT('',(57.5,-134.393099376732,-35.4928843561058));
#49916=CARTESIAN_POINT('Origin',(57.75,-131.669809380463,-34.1986447874607));
#49917=CARTESIAN_POINT('',(57.5,-131.75822132732,-33.9648001218105));
#49918=CARTESIAN_POINT('',(58.,-131.581397433607,-34.4324894531108));
#49919=CARTESIAN_POINT('Origin',(14.,-132.331838201602,-35.4582091790453));
#49920=CARTESIAN_POINT('Origin',(14.,-130.762333212168,-33.5882749320356));
#49921=CARTESIAN_POINT('Origin',(14.,-134.522508899283,-35.0099214429613));
#49922=CARTESIAN_POINT('Origin',(57.5,-129.790723455271,-48.3570826171013));
#49923=CARTESIAN_POINT('',(57.5,-130.446264217578,-48.0106462326609));
#49924=CARTESIAN_POINT('',(58.,-129.960169823373,-47.8842774043812));
#49925=CARTESIAN_POINT('',(57.5,-130.446264217578,-48.0106462326609));
#49926=CARTESIAN_POINT('',(57.5,-129.790723455271,-48.3570826171013));
#49927=CARTESIAN_POINT('',(57.5,-129.790723455271,-48.3570826171013));
#49928=CARTESIAN_POINT('',(58.,-129.960169823373,-47.8842774043812));
#49929=CARTESIAN_POINT('Origin',(14.,-130.118493836425,-48.1838644248811));
#49930=CARTESIAN_POINT('',(14.2512407024475,-130.118493836425,-48.1838644248811));
#49931=CARTESIAN_POINT('',(14.5,-129.790723455271,-48.3570826171013));
#49932=CARTESIAN_POINT('',(14.3353834448875,-130.007625623529,-48.2424554157598));
#49933=CARTESIAN_POINT('',(14.,-129.790723455271,-48.3570826171013));
#49934=CARTESIAN_POINT('',(14.5,-130.446264217578,-48.0106462326609));
#49935=CARTESIAN_POINT('',(14.,-130.446264217578,-48.0106462326609));
#49936=CARTESIAN_POINT('',(14.4305329766294,-130.354733034817,-48.0590181018757));
#49937=CARTESIAN_POINT('Origin',(57.75,-129.420919600612,-48.0049120124002));
#49938=CARTESIAN_POINT('',(58.,-129.482624563588,-47.762646667078));
#49939=CARTESIAN_POINT('',(57.5,-129.359214637636,-48.2471773577224));
#49940=CARTESIAN_POINT('Origin',(57.5,-130.788284360904,-47.070953611875));
#49941=CARTESIAN_POINT('',(57.5,-130.508796018164,-46.3841944650247));
#49942=CARTESIAN_POINT('',(58.,-130.334686134323,-46.8553022968291));
#49943=CARTESIAN_POINT('',(57.5,-130.508796018164,-46.3841944650247));
#49944=CARTESIAN_POINT('',(57.5,-130.788284360904,-47.070953611875));
#49945=CARTESIAN_POINT('',(57.5,-130.788284360904,-47.070953611875));
#49946=CARTESIAN_POINT('',(58.,-130.334686134323,-46.8553022968291));
#49947=CARTESIAN_POINT('Origin',(14.,-130.648540189534,-46.7275740384498));
#49948=CARTESIAN_POINT('',(14.2512407024475,-130.648540189534,-46.7275740384498));
#49949=CARTESIAN_POINT('',(14.5,-130.788284360904,-47.070953611875));
#49950=CARTESIAN_POINT('',(14.2590041943422,-130.65290144458,-46.738290520452));
#49951=CARTESIAN_POINT('',(14.,-130.788284360904,-47.070953611875));
#49952=CARTESIAN_POINT('',(14.5,-130.508796018164,-46.3841944650247));
#49953=CARTESIAN_POINT('',(14.,-130.508796018164,-46.3841944650247));
#49954=CARTESIAN_POINT('',(14.6801520303733,-130.407592981924,-46.13551822277));
#49955=CARTESIAN_POINT('Origin',(57.75,-130.553361205708,-46.9854485760436));
#49956=CARTESIAN_POINT('',(58.,-130.318438050511,-46.8999435402122));
#49957=CARTESIAN_POINT('',(57.5,-130.788284360904,-47.070953611875));
#49958=CARTESIAN_POINT('Origin',(57.75,-128.188157716154,-45.5442886531881));
#49959=CARTESIAN_POINT('',(57.5,-128.296614134382,-45.3190394459863));
#49960=CARTESIAN_POINT('',(58.,-128.079701297925,-45.7695378603898));
#49961=CARTESIAN_POINT('Origin',(14.25,-129.420919600612,-48.0049120124002));
#49962=CARTESIAN_POINT('',(14.,-129.960169823373,-47.8842774043812));
#49963=CARTESIAN_POINT('',(14.5,-130.275254145916,-48.4804925430539));
#49964=CARTESIAN_POINT('',(14.,-129.482624563588,-47.762646667078));
#49965=CARTESIAN_POINT('',(14.5,-129.359214637636,-48.2471773577224));
#49966=CARTESIAN_POINT('Origin',(14.,-130.959294432567,-46.601107301482));
#49967=CARTESIAN_POINT('',(14.5,-130.788284360904,-47.070953611875));
#49968=CARTESIAN_POINT('Origin',(14.25,-130.553361205708,-46.9854485760436));
#49969=CARTESIAN_POINT('',(14.,-130.334686134323,-46.8553022968291));
#49970=CARTESIAN_POINT('',(14.,-130.334686134323,-46.8553022968291));
#49971=CARTESIAN_POINT('',(14.,-130.318438050511,-46.8999435402122));
#49972=CARTESIAN_POINT('Origin',(14.25,-128.188157716154,-45.5442886531881));
#49973=CARTESIAN_POINT('',(14.5,-128.296614134382,-45.3190394459863));
#49974=CARTESIAN_POINT('',(14.,-128.079701297925,-45.7695378603898));
#49975=CARTESIAN_POINT('Origin',(14.,-127.337332006754,-44.857149679865));
#49976=CARTESIAN_POINT('Origin',(14.,-130.275254145916,-48.4804925430539));
#49977=CARTESIAN_POINT('Origin',(57.5,-126.188091528965,-58.2907844884389));
#49978=CARTESIAN_POINT('',(57.5,-125.969521727281,-57.5822796533797));
#49979=CARTESIAN_POINT('',(58.,-125.755014631118,-58.036420101407));
#49980=CARTESIAN_POINT('',(57.5,-125.969521727281,-57.5822796533797));
#49981=CARTESIAN_POINT('',(57.5,-126.188091528965,-58.2907844884389));
#49982=CARTESIAN_POINT('',(57.5,-126.188091528965,-58.2907844884389));
#49983=CARTESIAN_POINT('',(58.,-125.755014631118,-58.036420101407));
#49984=CARTESIAN_POINT('Origin',(57.5,-125.08223311503,-59.4850762228408));
#49985=CARTESIAN_POINT('',(57.5,-125.765473267224,-59.1970922754755));
#49986=CARTESIAN_POINT('',(58.,-125.292242378034,-59.0288384007668));
#49987=CARTESIAN_POINT('',(57.5,-125.765473267224,-59.1970922754755));
#49988=CARTESIAN_POINT('',(57.5,-125.08223311503,-59.4850762228408));
#49989=CARTESIAN_POINT('',(57.5,-125.08223311503,-59.4850762228408));
#49990=CARTESIAN_POINT('',(58.,-125.292242378034,-59.0288384007668));
#49991=CARTESIAN_POINT('Origin',(14.,-125.755014631118,-58.0364201014069));
#49992=CARTESIAN_POINT('',(14.5,-125.969521727281,-57.5822796533797));
#49993=CARTESIAN_POINT('',(14.5,-126.188091528965,-58.2907844884389));
#49994=CARTESIAN_POINT('',(14.5,-125.969521727281,-57.5822796533797));
#49995=CARTESIAN_POINT('',(14.,-125.755014631118,-58.0364201014069));
#49996=CARTESIAN_POINT('',(14.,-125.755014631118,-58.0364201014069));
#49997=CARTESIAN_POINT('',(14.5,-126.188091528965,-58.2907844884389));
#49998=CARTESIAN_POINT('Origin',(14.25,-123.730916769498,-56.5433129818713));
#49999=CARTESIAN_POINT('',(14.,-123.603241298728,-56.7582524481485));
#50000=CARTESIAN_POINT('',(14.5,-123.858592240269,-56.3283735155941));
#50001=CARTESIAN_POINT('Origin',(14.5,-125.08223311503,-59.4850762228408));
#50002=CARTESIAN_POINT('',(14.,-125.292242378034,-59.0288384007668));
#50003=CARTESIAN_POINT('',(14.5,-125.765473267224,-59.1970922754756));
#50004=CARTESIAN_POINT('',(14.,-125.292242378034,-59.0288384007668));
#50005=CARTESIAN_POINT('',(14.5,-125.08223311503,-59.4850762228408));
#50006=CARTESIAN_POINT('',(14.5,-125.08223311503,-59.4850762228408));
#50007=CARTESIAN_POINT('',(14.5,-125.765473267224,-59.1970922754755));
#50008=CARTESIAN_POINT('Origin',(14.25,-124.744530166311,-59.1020152039901));
#50009=CARTESIAN_POINT('',(14.5,-124.661945193235,-59.3379807146521));
#50010=CARTESIAN_POINT('',(14.,-124.827115139388,-58.8660496933282));
#50011=CARTESIAN_POINT('Origin',(14.,-125.423853191127,-59.3410842491582));
#50012=CARTESIAN_POINT('',(14.,-125.765473267224,-59.1970922754755));
#50013=CARTESIAN_POINT('',(14.,-125.08223311503,-59.4850762228408));
#50014=CARTESIAN_POINT('Origin',(14.25,-125.961514582206,-58.1851299230037));
#50015=CARTESIAN_POINT('',(14.5,-126.188091528965,-58.2907844884389));
#50016=CARTESIAN_POINT('',(14.,-125.734937635446,-58.0794753575685));
#50017=CARTESIAN_POINT('Origin',(14.,-126.078806628123,-57.9365320709093));
#50018=CARTESIAN_POINT('',(14.,-125.969521727281,-57.5822796533797));
#50019=CARTESIAN_POINT('',(14.,-126.188091528965,-58.2907844884389));
#50020=CARTESIAN_POINT('Origin',(57.75,-124.744530166311,-59.1020152039901));
#50021=CARTESIAN_POINT('',(58.,-124.827115139388,-58.8660496933282));
#50022=CARTESIAN_POINT('',(57.5,-124.661945193235,-59.3379807146521));
#50023=CARTESIAN_POINT('Origin',(57.75,-125.961514582206,-58.1851299230037));
#50024=CARTESIAN_POINT('',(58.,-125.734937635446,-58.0794753575685));
#50025=CARTESIAN_POINT('',(57.5,-126.188091528965,-58.2907844884389));
#50026=CARTESIAN_POINT('Origin',(57.75,-123.730916769498,-56.5433129818713));
#50027=CARTESIAN_POINT('',(57.5,-123.858592240269,-56.3283735155941));
#50028=CARTESIAN_POINT('',(58.,-123.603241298728,-56.7582524481486));
#50029=CARTESIAN_POINT('Origin',(14.,-124.164166824021,-57.8987018584758));
#50030=CARTESIAN_POINT('Origin',(14.,-122.943216816385,-55.7846344331431));
#50031=CARTESIAN_POINT('Origin',(14.,-126.399400659835,-57.8376305949206));
#50032=CARTESIAN_POINT('Origin',(57.5,-120.627531126037,-69.0669872981078));
#50033=CARTESIAN_POINT('',(57.5,-120.471543313576,-68.3421289244414));
#50034=CARTESIAN_POINT('',(58.,-120.218271533617,-68.7758457056645));
#50035=CARTESIAN_POINT('',(57.5,-120.471543313576,-68.3421289244414));
#50036=CARTESIAN_POINT('',(57.5,-120.627531126037,-69.0669872981078));
#50037=CARTESIAN_POINT('',(57.5,-120.627531126037,-69.0669872981078));
#50038=CARTESIAN_POINT('',(58.,-120.218271533617,-68.7758457056645));
#50039=CARTESIAN_POINT('Origin',(57.5,-119.421791454066,-70.1603524804535));
#50040=CARTESIAN_POINT('',(57.5,-120.127531126037,-69.9330127018922));
#50041=CARTESIAN_POINT('',(58.,-119.670765314673,-69.7241542943354));
#50042=CARTESIAN_POINT('',(57.5,-120.127531126037,-69.9330127018922));
#50043=CARTESIAN_POINT('',(57.5,-119.421791454066,-70.1603524804535));
#50044=CARTESIAN_POINT('',(57.5,-119.421791454066,-70.1603524804535));
#50045=CARTESIAN_POINT('',(58.,-119.670765314673,-69.7241542943354));
#50046=CARTESIAN_POINT('Origin',(14.,-120.218271533617,-68.7758457056646));
#50047=CARTESIAN_POINT('',(14.5,-120.471543313576,-68.3421289244414));
#50048=CARTESIAN_POINT('',(14.5,-120.627531126037,-69.0669872981078));
#50049=CARTESIAN_POINT('',(14.5,-120.471543313576,-68.3421289244414));
#50050=CARTESIAN_POINT('',(14.,-120.218271533617,-68.7758457056646));
#50051=CARTESIAN_POINT('',(14.,-120.218271533617,-68.7758457056646));
#50052=CARTESIAN_POINT('',(14.5,-120.627531126037,-69.0669872981078));
#50053=CARTESIAN_POINT('Origin',(14.25,-118.332008835457,-67.1120085569767));
#50054=CARTESIAN_POINT('',(14.,-118.18608599957,-67.3150024632071));
#50055=CARTESIAN_POINT('',(14.5,-118.477931671344,-66.9090146507463));
#50056=CARTESIAN_POINT('Origin',(14.5,-119.421791454066,-70.1603524804535));
#50057=CARTESIAN_POINT('',(14.,-119.670765314673,-69.7241542943354));
#50058=CARTESIAN_POINT('',(14.5,-120.127531126037,-69.9330127018922));
#50059=CARTESIAN_POINT('',(14.,-119.670765314673,-69.7241542943354));
#50060=CARTESIAN_POINT('',(14.5,-119.421791454066,-70.1603524804535));
#50061=CARTESIAN_POINT('',(14.5,-119.421791454066,-70.1603524804535));
#50062=CARTESIAN_POINT('',(14.5,-120.127531126037,-69.9330127018922));
#50063=CARTESIAN_POINT('Origin',(14.25,-119.118759534638,-69.7493163731052));
#50064=CARTESIAN_POINT('',(14.5,-119.015923072972,-69.9771862090909));
#50065=CARTESIAN_POINT('',(14.,-119.221595996303,-69.5214465371196));
#50066=CARTESIAN_POINT('Origin',(14.,-119.774661290051,-70.0466825911729));
#50067=CARTESIAN_POINT('',(14.,-120.127531126037,-69.9330127018922));
#50068=CARTESIAN_POINT('',(14.,-119.421791454066,-70.1603524804535));
#50069=CARTESIAN_POINT('Origin',(14.25,-120.411024775091,-68.9419872981077));
#50070=CARTESIAN_POINT('',(14.5,-120.627531126037,-69.0669872981077));
#50071=CARTESIAN_POINT('',(14.,-120.194518424145,-68.8169872981078));
#50072=CARTESIAN_POINT('Origin',(14.,-120.549537219807,-68.7045581112746));
#50073=CARTESIAN_POINT('',(14.,-120.471543313576,-68.3421289244414));
#50074=CARTESIAN_POINT('',(14.,-120.627531126037,-69.0669872981078));
#50075=CARTESIAN_POINT('Origin',(57.75,-119.118759534638,-69.7493163731052));
#50076=CARTESIAN_POINT('',(58.,-119.221595996303,-69.5214465371196));
#50077=CARTESIAN_POINT('',(57.5,-119.015923072972,-69.9771862090909));
#50078=CARTESIAN_POINT('Origin',(57.75,-120.411024775091,-68.9419872981077));
#50079=CARTESIAN_POINT('',(58.,-120.194518424145,-68.8169872981077));
#50080=CARTESIAN_POINT('',(57.5,-120.627531126037,-69.0669872981077));
#50081=CARTESIAN_POINT('Origin',(57.75,-118.332008835457,-67.1120085569767));
#50082=CARTESIAN_POINT('',(57.5,-118.477931671344,-66.9090146507463));
#50083=CARTESIAN_POINT('',(58.,-118.18608599957,-67.3150024632071));
#50084=CARTESIAN_POINT('Origin',(14.,-118.645480318468,-68.5));
#50085=CARTESIAN_POINT('Origin',(14.,-117.613429510899,-66.2875644347018));
#50086=CARTESIAN_POINT('Origin',(14.,-120.877531126037,-68.6339745962155));
#50087=CARTESIAN_POINT('Origin',(57.75,-112.032522863357,-77.1699412236247));
#50088=CARTESIAN_POINT('',(57.7487592975525,-114.102813043447,-78.9497009794667));
#50089=CARTESIAN_POINT('',(58.,-113.766594799967,-78.991845596111));
#50090=CARTESIAN_POINT('',(58.2319907935076,-113.456137392641,-79.0307611180075));
#50091=CARTESIAN_POINT('',(58.,-111.869463223246,-77.3594446636108));
#50092=CARTESIAN_POINT('',(57.5,-114.056703712549,-78.5818533282824));
#50093=CARTESIAN_POINT('',(57.5,-112.195582503469,-76.9804377836386));
#50094=CARTESIAN_POINT('',(50.4896657310026,-112.757287667812,-68.2154669449852));
#50095=CARTESIAN_POINT('Origin',(58.,-112.223830067592,-78.5799717800933));
#50096=CARTESIAN_POINT('',(58.,-113.138521468083,-79.8888272731287));
#50097=CARTESIAN_POINT('',(58.,-113.739346352201,-79.0307604124754));
#50098=CARTESIAN_POINT('',(58.,-112.708728519719,-79.6477431945663));
#50099=CARTESIAN_POINT('Origin',(57.75,-113.944134363273,-79.1741545215631));
#50100=CARTESIAN_POINT('',(57.5,-114.148922374345,-79.3175486306509));
#50101=CARTESIAN_POINT('',(57.5,-114.148922374345,-79.3175486306509));
#50102=CARTESIAN_POINT('',(57.5,-113.575345937994,-80.1367006749399));
#50103=CARTESIAN_POINT('',(57.5,-114.148922374345,-79.3175486306509));
#50104=CARTESIAN_POINT('',(57.5,-113.575345937994,-80.1367006749399));
#50105=CARTESIAN_POINT('Origin',(14.,-114.102813043447,-78.9497009794667));
#50106=CARTESIAN_POINT('',(14.5,-114.056703712549,-78.5818533282824));
#50107=CARTESIAN_POINT('',(14.,-114.056703712549,-78.5818533282824));
#50108=CARTESIAN_POINT('',(14.5,-114.148922374345,-79.3175486306509));
#50109=CARTESIAN_POINT('',(14.5,-114.056703712549,-78.5818533282824));
#50110=CARTESIAN_POINT('',(14.,-114.148922374345,-79.3175486306509));
#50111=CARTESIAN_POINT('Origin',(57.5,-112.852477851287,-80.3016660917109));
#50112=CARTESIAN_POINT('',(57.5,-112.852477851287,-80.3016660917109));
#50113=CARTESIAN_POINT('',(57.5,-112.852477851287,-80.3016660917109));
#50114=CARTESIAN_POINT('',(58.,-113.138521468083,-79.8888272731287));
#50115=CARTESIAN_POINT('Origin',(14.,-113.766594799967,-78.991845596111));
#50116=CARTESIAN_POINT('',(14.,-113.766594799967,-78.991845596111));
#50117=CARTESIAN_POINT('',(14.,-113.766594799967,-78.991845596111));
#50118=CARTESIAN_POINT('',(14.5,-114.148922374345,-79.3175486306509));
#50119=CARTESIAN_POINT('Origin',(14.25,-112.032522863357,-77.1699412236247));
#50120=CARTESIAN_POINT('',(14.,-111.869463223246,-77.3594446636108));
#50121=CARTESIAN_POINT('',(14.5,-112.195582503469,-76.9804377836386));
#50122=CARTESIAN_POINT('Origin',(14.5,-112.852477851287,-80.3016660917109));
#50123=CARTESIAN_POINT('',(14.,-113.138521468083,-79.8888272731287));
#50124=CARTESIAN_POINT('',(14.5,-113.575345937994,-80.1367006749399));
#50125=CARTESIAN_POINT('',(14.,-113.138521468083,-79.8888272731287));
#50126=CARTESIAN_POINT('',(14.5,-112.852477851287,-80.3016660917109));
#50127=CARTESIAN_POINT('',(14.5,-112.852477851287,-80.3016660917109));
#50128=CARTESIAN_POINT('',(14.5,-113.575345937994,-80.1367006749399));
#50129=CARTESIAN_POINT('Origin',(14.25,-112.586423217032,-79.8657831288322));
#50130=CARTESIAN_POINT('',(14.5,-112.464117914346,-80.0838230630982));
#50131=CARTESIAN_POINT('',(14.,-112.708728519719,-79.6477431945663));
#50132=CARTESIAN_POINT('Origin',(14.,-113.213911894641,-80.2191833833254));
#50133=CARTESIAN_POINT('',(14.,-113.575345937994,-80.1367006749399));
#50134=CARTESIAN_POINT('',(14.,-112.852477851287,-80.3016660917109));
#50135=CARTESIAN_POINT('Origin',(14.25,-113.944134363273,-79.1741545215631));
#50136=CARTESIAN_POINT('',(14.5,-114.148922374345,-79.3175486306509));
#50137=CARTESIAN_POINT('',(14.,-113.739346352201,-79.0307604124754));
#50138=CARTESIAN_POINT('Origin',(57.75,-112.586423217032,-79.8657831288322));
#50139=CARTESIAN_POINT('',(57.5,-112.464117914346,-80.0838230630982));
#50140=CARTESIAN_POINT('Origin',(14.,-111.388532989905,-76.2860060453866));
#50141=CARTESIAN_POINT('Origin',(14.,-114.435710592521,-78.9079726085064));
#50142=CARTESIAN_POINT('Origin',(57.5,-106.801571398381,-88.9644555248695));
#50143=CARTESIAN_POINT('',(57.5,-106.773823726948,-88.223522379275));
#50144=CARTESIAN_POINT('',(58.,-106.449085585742,-88.6066698449906));
#50145=CARTESIAN_POINT('',(57.5,-106.773823726948,-88.223522379275));
#50146=CARTESIAN_POINT('',(57.5,-106.801571398381,-88.9644555248695));
#50147=CARTESIAN_POINT('',(57.5,-106.801571398381,-88.9644555248695));
#50148=CARTESIAN_POINT('',(58.,-106.449085585742,-88.6066698449906));
#50149=CARTESIAN_POINT('Origin',(57.5,-105.424288749871,-89.8318355365386));
#50150=CARTESIAN_POINT('',(57.5,-106.158783788695,-89.7304999679885));
#50151=CARTESIAN_POINT('',(58.,-105.745225158215,-89.4454980381808));
#50152=CARTESIAN_POINT('',(57.5,-106.158783788695,-89.7304999679885));
#50153=CARTESIAN_POINT('',(57.5,-105.424288749871,-89.8318355365386));
#50154=CARTESIAN_POINT('',(57.5,-105.424288749871,-89.8318355365386));
#50155=CARTESIAN_POINT('',(58.,-105.745225158215,-89.4454980381808));
#50156=CARTESIAN_POINT('Origin',(14.,-106.449085585742,-88.6066698449906));
#50157=CARTESIAN_POINT('',(14.5,-106.773823726948,-88.223522379275));
#50158=CARTESIAN_POINT('',(14.5,-106.801571398381,-88.9644555248695));
#50159=CARTESIAN_POINT('',(14.5,-106.773823726948,-88.223522379275));
#50160=CARTESIAN_POINT('',(14.,-106.449085585742,-88.6066698449906));
#50161=CARTESIAN_POINT('',(14.,-106.449085585742,-88.6066698449906));
#50162=CARTESIAN_POINT('',(14.5,-106.801571398381,-88.9644555248695));
#50163=CARTESIAN_POINT('Origin',(14.25,-104.880401745181,-86.6405640410765));
#50164=CARTESIAN_POINT('',(14.,-104.701446283163,-86.8151347792147));
#50165=CARTESIAN_POINT('',(14.5,-105.059357207198,-86.4659933029383));
#50166=CARTESIAN_POINT('Origin',(14.5,-105.424288749871,-89.8318355365386));
#50167=CARTESIAN_POINT('',(14.,-105.745225158215,-89.4454980381808));
#50168=CARTESIAN_POINT('',(14.5,-106.158783788695,-89.7304999679885));
#50169=CARTESIAN_POINT('',(14.,-105.745225158215,-89.4454980381808));
#50170=CARTESIAN_POINT('',(14.5,-105.424288749871,-89.8318355365386));
#50171=CARTESIAN_POINT('',(14.5,-105.424288749871,-89.8318355365386));
#50172=CARTESIAN_POINT('',(14.5,-106.158783788695,-89.7304999679885));
#50173=CARTESIAN_POINT('Origin',(14.25,-105.197236237204,-89.3744230506705));
#50174=CARTESIAN_POINT('',(14.5,-105.0563929107,-89.5809736676609));
#50175=CARTESIAN_POINT('',(14.,-105.338079563709,-89.1678724336801));
#50176=CARTESIAN_POINT('Origin',(14.,-105.791536269283,-89.7811677522635));
#50177=CARTESIAN_POINT('',(14.,-106.158783788695,-89.7304999679885));
#50178=CARTESIAN_POINT('',(14.,-105.424288749871,-89.8318355365386));
#50179=CARTESIAN_POINT('Origin',(14.25,-106.610060287601,-88.8037586224479));
#50180=CARTESIAN_POINT('',(14.5,-106.801571398381,-88.9644555248695));
#50181=CARTESIAN_POINT('',(14.,-106.418549176822,-88.6430617200262));
#50182=CARTESIAN_POINT('Origin',(14.,-106.787697562665,-88.5939889520722));
#50183=CARTESIAN_POINT('',(14.,-106.773823726948,-88.223522379275));
#50184=CARTESIAN_POINT('',(14.,-106.801571398381,-88.9644555248695));
#50185=CARTESIAN_POINT('Origin',(57.75,-105.197236237204,-89.3744230506705));
#50186=CARTESIAN_POINT('',(58.,-105.338079563709,-89.1678724336801));
#50187=CARTESIAN_POINT('',(57.5,-105.0563929107,-89.5809736676609));
#50188=CARTESIAN_POINT('Origin',(57.75,-106.610060287601,-88.8037586224479));
#50189=CARTESIAN_POINT('',(58.,-106.418549176822,-88.6430617200262));
#50190=CARTESIAN_POINT('',(57.5,-106.801571398381,-88.9644555248695));
#50191=CARTESIAN_POINT('Origin',(57.75,-104.880401745181,-86.6405640410765));
#50192=CARTESIAN_POINT('',(57.5,-105.059357207198,-86.4659933029383));
#50193=CARTESIAN_POINT('',(58.,-104.701446283163,-86.8151347792147));
#50194=CARTESIAN_POINT('Origin',(14.,-104.9480887073,-88.0619025270559));
#50195=CARTESIAN_POINT('Origin',(14.,-104.315902474623,-85.7038650873162));
#50196=CARTESIAN_POINT('Origin',(14.,-107.122965203224,-88.58143330331));
#50197=CARTESIAN_POINT('Origin',(57.5,-97.1937571541419,-98.678330470988));
#50198=CARTESIAN_POINT('',(57.5,-97.9342891943368,-98.6413959755234));
#50199=CARTESIAN_POINT('',(58.,-97.5471438341798,-98.3214345544939));
#50200=CARTESIAN_POINT('',(57.5,-97.9342891943368,-98.6413959755234));
#50201=CARTESIAN_POINT('',(57.5,-97.1937571541419,-98.678330470988));
#50202=CARTESIAN_POINT('',(57.5,-97.1937571541419,-98.678330470988));
#50203=CARTESIAN_POINT('',(58.,-97.5471438341798,-98.3214345544939));
#50204=CARTESIAN_POINT('Origin',(14.,-97.5640231742394,-98.6598632232557));
#50205=CARTESIAN_POINT('',(14.2512407024475,-97.5640231742394,-98.6598632232557));
#50206=CARTESIAN_POINT('',(14.5,-97.1937571541419,-98.678330470988));
#50207=CARTESIAN_POINT('',(14.3353834448875,-97.4387808268383,-98.666109763123));
#50208=CARTESIAN_POINT('',(14.,-97.1937571541419,-98.678330470988));
#50209=CARTESIAN_POINT('',(14.5,-97.9342891943368,-98.6413959755234));
#50210=CARTESIAN_POINT('',(14.,-97.9342891943368,-98.6413959755234));
#50211=CARTESIAN_POINT('',(14.4305329766294,-97.8308909353592,-98.6465530279127));
#50212=CARTESIAN_POINT('Origin',(57.75,-97.0074347697832,-98.2028696473411));
#50213=CARTESIAN_POINT('',(58.,-97.1657442173475,-98.0093803225402));
#50214=CARTESIAN_POINT('',(57.5,-96.8491253222189,-98.3963589721419));
#50215=CARTESIAN_POINT('Origin',(57.5,-98.6413959755234,-97.9342891943368));
#50216=CARTESIAN_POINT('',(57.5,-98.678330470988,-97.1937571541419));
#50217=CARTESIAN_POINT('',(58.,-98.3214345544939,-97.5471438341797));
#50218=CARTESIAN_POINT('',(57.5,-98.678330470988,-97.1937571541419));
#50219=CARTESIAN_POINT('',(57.5,-98.6413959755234,-97.9342891943368));
#50220=CARTESIAN_POINT('',(57.5,-98.6413959755234,-97.9342891943368));
#50221=CARTESIAN_POINT('',(58.,-98.3214345544939,-97.5471438341797));
#50222=CARTESIAN_POINT('Origin',(14.,-98.6598632232557,-97.5640231742394));
#50223=CARTESIAN_POINT('',(14.2512407024475,-98.6598632232557,-97.5640231742394));
#50224=CARTESIAN_POINT('',(14.5,-98.6413959755234,-97.9342891943368));
#50225=CARTESIAN_POINT('',(14.2590041943422,-98.6592868816697,-97.5755787513542));
#50226=CARTESIAN_POINT('',(14.,-98.6413959755234,-97.9342891943368));
#50227=CARTESIAN_POINT('',(14.5,-98.678330470988,-97.1937571541419));
#50228=CARTESIAN_POINT('',(14.,-98.678330470988,-97.1937571541419));
#50229=CARTESIAN_POINT('',(14.6801520303733,-98.69170449241,-96.925609688077));
#50230=CARTESIAN_POINT('Origin',(57.75,-98.4646192802267,-97.7575124990402));
#50231=CARTESIAN_POINT('',(58.,-98.2878425849301,-97.5807358037436));
#50232=CARTESIAN_POINT('',(57.5,-98.6413959755234,-97.9342891943368));
#50233=CARTESIAN_POINT('Origin',(57.75,-96.9300774412053,-95.4517998511728));
#50234=CARTESIAN_POINT('',(57.5,-97.1235667660061,-95.2934904036084));
#50235=CARTESIAN_POINT('',(58.,-96.7365881164045,-95.6101092987371));
#50236=CARTESIAN_POINT('Origin',(14.25,-97.0074347697832,-98.2028696473411));
#50237=CARTESIAN_POINT('',(14.,-97.5471438341798,-98.3214345544939));
#50238=CARTESIAN_POINT('',(14.5,-97.5807358037436,-98.9949493661167));
#50239=CARTESIAN_POINT('',(14.,-97.1657442173475,-98.0093803225402));
#50240=CARTESIAN_POINT('',(14.5,-96.8491253222189,-98.3963589721419));
#50241=CARTESIAN_POINT('Origin',(14.,-98.9949493661167,-97.5807358037436));
#50242=CARTESIAN_POINT('',(14.5,-98.6413959755234,-97.9342891943368));
#50243=CARTESIAN_POINT('Origin',(14.25,-98.4646192802267,-97.7575124990402));
#50244=CARTESIAN_POINT('',(14.,-98.3214345544939,-97.5471438341797));
#50245=CARTESIAN_POINT('',(14.,-98.3214345544939,-97.5471438341797));
#50246=CARTESIAN_POINT('',(14.,-98.2878425849301,-97.5807358037436));
#50247=CARTESIAN_POINT('Origin',(14.25,-96.9300774412053,-95.4517998511728));
#50248=CARTESIAN_POINT('',(14.5,-97.1235667660061,-95.2934904036084));
#50249=CARTESIAN_POINT('',(14.,-96.7365881164044,-95.6101092987371));
#50250=CARTESIAN_POINT('Origin',(14.,-96.4493649538451,-94.4694659665227));
#50251=CARTESIAN_POINT('Origin',(14.,-97.5807358037436,-98.9949493661167));
#50252=CARTESIAN_POINT('Origin',(57.5,-89.7304999679885,-106.158783788695));
#50253=CARTESIAN_POINT('',(57.5,-89.8318355365387,-105.424288749871));
#50254=CARTESIAN_POINT('',(58.,-89.4454980381808,-105.745225158215));
#50255=CARTESIAN_POINT('',(57.5,-89.8318355365387,-105.424288749871));
#50256=CARTESIAN_POINT('',(57.5,-89.7304999679885,-106.158783788695));
#50257=CARTESIAN_POINT('',(57.5,-89.7304999679885,-106.158783788695));
#50258=CARTESIAN_POINT('',(58.,-89.4454980381808,-105.745225158215));
#50259=CARTESIAN_POINT('Origin',(57.5,-88.223522379275,-106.773823726948));
#50260=CARTESIAN_POINT('',(57.5,-88.9644555248695,-106.801571398381));
#50261=CARTESIAN_POINT('',(58.,-88.6066698449906,-106.449085585742));
#50262=CARTESIAN_POINT('',(57.5,-88.9644555248695,-106.801571398381));
#50263=CARTESIAN_POINT('',(57.5,-88.223522379275,-106.773823726948));
#50264=CARTESIAN_POINT('',(57.5,-88.223522379275,-106.773823726948));
#50265=CARTESIAN_POINT('',(58.,-88.6066698449906,-106.449085585742));
#50266=CARTESIAN_POINT('Origin',(14.,-89.4454980381808,-105.745225158215));
#50267=CARTESIAN_POINT('',(14.5,-89.8318355365387,-105.424288749871));
#50268=CARTESIAN_POINT('',(14.5,-89.7304999679885,-106.158783788695));
#50269=CARTESIAN_POINT('',(14.5,-89.8318355365387,-105.424288749871));
#50270=CARTESIAN_POINT('',(14.,-89.4454980381808,-105.745225158215));
#50271=CARTESIAN_POINT('',(14.,-89.4454980381808,-105.745225158215));
#50272=CARTESIAN_POINT('',(14.5,-89.7304999679885,-106.158783788695));
#50273=CARTESIAN_POINT('Origin',(14.25,-88.2420567199213,-103.536589829029));
#50274=CARTESIAN_POINT('',(14.,-88.0355061029309,-103.677433155534));
#50275=CARTESIAN_POINT('',(14.5,-88.4486073369116,-103.395746502524));
#50276=CARTESIAN_POINT('Origin',(14.5,-88.223522379275,-106.773823726948));
#50277=CARTESIAN_POINT('',(14.,-88.6066698449906,-106.449085585742));
#50278=CARTESIAN_POINT('',(14.5,-88.9644555248695,-106.801571398381));
#50279=CARTESIAN_POINT('',(14.,-88.6066698449906,-106.449085585742));
#50280=CARTESIAN_POINT('',(14.5,-88.223522379275,-106.773823726948));
#50281=CARTESIAN_POINT('',(14.5,-88.223522379275,-106.773823726948));
#50282=CARTESIAN_POINT('',(14.5,-88.9644555248695,-106.801571398381));
#50283=CARTESIAN_POINT('Origin',(14.25,-88.0793481490734,-106.283933109481));
#50284=CARTESIAN_POINT('',(14.5,-87.9047774109353,-106.462888571499));
#50285=CARTESIAN_POINT('',(14.,-88.2539188872116,-106.104977647464));
#50286=CARTESIAN_POINT('Origin',(14.,-88.5939889520723,-106.787697562665));
#50287=CARTESIAN_POINT('',(14.,-88.9644555248695,-106.801571398381));
#50288=CARTESIAN_POINT('',(14.,-88.223522379275,-106.773823726948));
#50289=CARTESIAN_POINT('Origin',(14.25,-89.5698030655668,-105.967272677915));
#50290=CARTESIAN_POINT('',(14.5,-89.7304999679885,-106.158783788695));
#50291=CARTESIAN_POINT('',(14.,-89.4091061631452,-105.775761567135));
#50292=CARTESIAN_POINT('Origin',(14.,-89.7811677522636,-105.791536269283));
#50293=CARTESIAN_POINT('',(14.,-89.8318355365387,-105.424288749871));
#50294=CARTESIAN_POINT('',(14.,-89.7304999679885,-106.158783788695));
#50295=CARTESIAN_POINT('Origin',(57.75,-88.0793481490734,-106.283933109481));
#50296=CARTESIAN_POINT('',(58.,-88.2539188872116,-106.104977647464));
#50297=CARTESIAN_POINT('',(57.5,-87.9047774109353,-106.462888571499));
#50298=CARTESIAN_POINT('Origin',(57.75,-89.5698030655668,-105.967272677915));
#50299=CARTESIAN_POINT('',(58.,-89.4091061631452,-105.775761567135));
#50300=CARTESIAN_POINT('',(57.5,-89.7304999679885,-106.158783788695));
#50301=CARTESIAN_POINT('Origin',(57.75,-88.2420567199213,-103.536589829029));
#50302=CARTESIAN_POINT('',(57.5,-88.4486073369116,-103.395746502524));
#50303=CARTESIAN_POINT('',(58.,-88.0355061029309,-103.677433155534));
#50304=CARTESIAN_POINT('Origin',(14.,-88.0619025270559,-104.9480887073));
#50305=CARTESIAN_POINT('Origin',(14.,-87.8487895280494,-102.516097167501));
#50306=CARTESIAN_POINT('Origin',(14.,-90.113522189548,-105.837389983851));
#50307=CARTESIAN_POINT('Origin',(57.5,-80.13670067494,-113.575345937994));
#50308=CARTESIAN_POINT('',(57.5,-80.301666091711,-112.852477851287));
#50309=CARTESIAN_POINT('',(58.,-79.8888272731288,-113.138521468083));
#50310=CARTESIAN_POINT('',(57.5,-80.301666091711,-112.852477851287));
#50311=CARTESIAN_POINT('',(57.5,-80.13670067494,-113.575345937994));
#50312=CARTESIAN_POINT('',(57.5,-80.13670067494,-113.575345937994));
#50313=CARTESIAN_POINT('',(58.,-79.8888272731288,-113.138521468083));
#50314=CARTESIAN_POINT('Origin',(57.5,-78.5818533282825,-114.056703712549));
#50315=CARTESIAN_POINT('',(57.5,-79.317548630651,-114.148922374345));
#50316=CARTESIAN_POINT('',(58.,-78.9918455961111,-113.766594799967));
#50317=CARTESIAN_POINT('',(57.5,-79.317548630651,-114.148922374345));
#50318=CARTESIAN_POINT('',(57.5,-78.5818533282825,-114.056703712549));
#50319=CARTESIAN_POINT('',(57.5,-78.5818533282825,-114.056703712549));
#50320=CARTESIAN_POINT('',(58.,-78.9918455961111,-113.766594799967));
#50321=CARTESIAN_POINT('Origin',(14.,-79.8888272731288,-113.138521468083));
#50322=CARTESIAN_POINT('',(14.5,-80.301666091711,-112.852477851287));
#50323=CARTESIAN_POINT('',(14.5,-80.13670067494,-113.575345937994));
#50324=CARTESIAN_POINT('',(14.5,-80.301666091711,-112.852477851287));
#50325=CARTESIAN_POINT('',(14.,-79.8888272731288,-113.138521468083));
#50326=CARTESIAN_POINT('',(14.,-79.8888272731288,-113.138521468083));
#50327=CARTESIAN_POINT('',(14.5,-80.13670067494,-113.575345937994));
#50328=CARTESIAN_POINT('Origin',(14.25,-78.882460664988,-110.833403841184));
#50329=CARTESIAN_POINT('',(14.,-78.6644207307221,-110.955709143871));
#50330=CARTESIAN_POINT('',(14.5,-79.100500599254,-110.711098538497));
#50331=CARTESIAN_POINT('Origin',(14.5,-78.5818533282825,-114.056703712549));
#50332=CARTESIAN_POINT('',(14.,-78.991845596111,-113.766594799967));
#50333=CARTESIAN_POINT('',(14.5,-79.317548630651,-114.148922374345));
#50334=CARTESIAN_POINT('',(14.,-78.991845596111,-113.766594799967));
#50335=CARTESIAN_POINT('',(14.5,-78.5818533282825,-114.056703712549));
#50336=CARTESIAN_POINT('',(14.5,-78.5818533282825,-114.056703712549));
#50337=CARTESIAN_POINT('',(14.5,-79.317548630651,-114.148922374345));
#50338=CARTESIAN_POINT('Origin',(14.25,-78.4809245051847,-113.556111664665));
#50339=CARTESIAN_POINT('',(14.5,-78.2914210651986,-113.719171304777));
#50340=CARTESIAN_POINT('',(14.,-78.6704279451708,-113.393052024553));
#50341=CARTESIAN_POINT('Origin',(14.,-78.9497009794668,-114.102813043447));
#50342=CARTESIAN_POINT('',(14.,-79.317548630651,-114.148922374345));
#50343=CARTESIAN_POINT('',(14.,-78.5818533282825,-114.056703712549));
#50344=CARTESIAN_POINT('Origin',(14.25,-79.9933065658522,-113.370557926922));
#50345=CARTESIAN_POINT('',(14.5,-80.13670067494,-113.575345937994));
#50346=CARTESIAN_POINT('',(14.,-79.8499124567644,-113.16576991585));
#50347=CARTESIAN_POINT('Origin',(14.,-80.2191833833255,-113.213911894641));
#50348=CARTESIAN_POINT('',(14.,-80.301666091711,-112.852477851287));
#50349=CARTESIAN_POINT('',(14.,-80.13670067494,-113.575345937994));
#50350=CARTESIAN_POINT('Origin',(57.75,-78.4809245051847,-113.556111664665));
#50351=CARTESIAN_POINT('',(58.,-78.6704279451708,-113.393052024553));
#50352=CARTESIAN_POINT('',(57.5,-78.2914210651986,-113.719171304777));
#50353=CARTESIAN_POINT('Origin',(57.75,-79.9933065658522,-113.370557926922));
#50354=CARTESIAN_POINT('',(58.,-79.8499124567644,-113.16576991585));
#50355=CARTESIAN_POINT('',(57.5,-80.13670067494,-113.575345937994));
#50356=CARTESIAN_POINT('Origin',(57.75,-78.882460664988,-110.833403841184));
#50357=CARTESIAN_POINT('',(57.5,-79.100500599254,-110.711098538497));
#50358=CARTESIAN_POINT('',(58.,-78.6644207307221,-110.955709143871));
#50359=CARTESIAN_POINT('Origin',(14.,-78.5799717800934,-112.223830067592));
#50360=CARTESIAN_POINT('Origin',(14.,-78.5796317693959,-109.782518968122));
#50361=CARTESIAN_POINT('Origin',(14.,-80.5462766970845,-113.288557719819));
#50362=CARTESIAN_POINT('Origin',(57.75,-68.9225214538621,-117.286708727069));
#50363=CARTESIAN_POINT('',(57.7487592975525,-70.0466825911729,-119.774661290051));
#50364=CARTESIAN_POINT('',(58.,-69.7241542943354,-119.670765314673));
#50365=CARTESIAN_POINT('',(58.2319907935076,-69.4263379183141,-119.574829785376));
#50366=CARTESIAN_POINT('',(58.,-68.6946516178765,-117.389545188734));
#50367=CARTESIAN_POINT('',(57.5,-70.1603524804535,-119.421791454066));
#50368=CARTESIAN_POINT('',(57.5,-69.1503912898478,-117.183872265404));
#50369=CARTESIAN_POINT('',(50.4896657310027,-73.3637057943502,-109.477497801348));
#50370=CARTESIAN_POINT('Origin',(58.,-68.5,-118.645480318468));
#50371=CARTESIAN_POINT('',(58.,-68.7758457056646,-120.218271533617));
#50372=CARTESIAN_POINT('',(58.,-69.6830127018922,-119.694518424145));
#50373=CARTESIAN_POINT('',(58.,-68.488207543964,-119.818136807139));
#50374=CARTESIAN_POINT('Origin',(57.75,-69.8080127018922,-119.911024775091));
#50375=CARTESIAN_POINT('',(57.5,-69.9330127018922,-120.127531126037));
#50376=CARTESIAN_POINT('',(57.5,-69.9330127018922,-120.127531126037));
#50377=CARTESIAN_POINT('',(57.5,-69.0669872981078,-120.627531126037));
#50378=CARTESIAN_POINT('',(57.5,-69.9330127018922,-120.127531126037));
#50379=CARTESIAN_POINT('',(57.5,-69.0669872981078,-120.627531126037));
#50380=CARTESIAN_POINT('Origin',(14.,-70.0466825911729,-119.774661290051));
#50381=CARTESIAN_POINT('',(14.5,-70.1603524804535,-119.421791454066));
#50382=CARTESIAN_POINT('',(14.,-70.1603524804535,-119.421791454066));
#50383=CARTESIAN_POINT('',(14.5,-69.9330127018922,-120.127531126037));
#50384=CARTESIAN_POINT('',(14.5,-70.1603524804535,-119.421791454066));
#50385=CARTESIAN_POINT('',(14.,-69.9330127018922,-120.127531126037));
#50386=CARTESIAN_POINT('Origin',(57.5,-68.3421289244414,-120.471543313576));
#50387=CARTESIAN_POINT('',(57.5,-68.3421289244414,-120.471543313576));
#50388=CARTESIAN_POINT('',(57.5,-68.3421289244414,-120.471543313576));
#50389=CARTESIAN_POINT('',(58.,-68.7758457056646,-120.218271533617));
#50390=CARTESIAN_POINT('Origin',(14.,-69.7241542943354,-119.670765314673));
#50391=CARTESIAN_POINT('',(14.,-69.7241542943354,-119.670765314673));
#50392=CARTESIAN_POINT('',(14.,-69.7241542943354,-119.670765314673));
#50393=CARTESIAN_POINT('',(14.5,-69.9330127018922,-120.127531126037));
#50394=CARTESIAN_POINT('Origin',(14.25,-68.9225214538621,-117.286708727069));
#50395=CARTESIAN_POINT('',(14.,-68.6946516178764,-117.389545188734));
#50396=CARTESIAN_POINT('',(14.5,-69.1503912898478,-117.183872265404));
#50397=CARTESIAN_POINT('Origin',(14.5,-68.3421289244414,-120.471543313576));
#50398=CARTESIAN_POINT('',(14.,-68.7758457056646,-120.218271533617));
#50399=CARTESIAN_POINT('',(14.5,-69.0669872981078,-120.627531126037));
#50400=CARTESIAN_POINT('',(14.,-68.7758457056646,-120.218271533617));
#50401=CARTESIAN_POINT('',(14.5,-68.3421289244414,-120.471543313576));
#50402=CARTESIAN_POINT('',(14.5,-68.3421289244414,-120.471543313576));
#50403=CARTESIAN_POINT('',(14.5,-69.0669872981078,-120.627531126037));
#50404=CARTESIAN_POINT('Origin',(14.25,-68.2852136377336,-119.964059643026));
#50405=CARTESIAN_POINT('',(14.5,-68.0822197315031,-120.109982478913));
#50406=CARTESIAN_POINT('',(14.,-68.488207543964,-119.818136807139));
#50407=CARTESIAN_POINT('Origin',(14.,-68.7045581112746,-120.549537219807));
#50408=CARTESIAN_POINT('',(14.,-69.0669872981078,-120.627531126037));
#50409=CARTESIAN_POINT('',(14.,-68.3421289244414,-120.471543313576));
#50410=CARTESIAN_POINT('Origin',(14.25,-69.8080127018922,-119.911024775091));
#50411=CARTESIAN_POINT('',(14.5,-69.9330127018922,-120.127531126037));
#50412=CARTESIAN_POINT('',(14.,-69.6830127018922,-119.694518424145));
#50413=CARTESIAN_POINT('Origin',(57.75,-68.2852136377336,-119.964059643026));
#50414=CARTESIAN_POINT('',(57.5,-68.0822197315031,-120.109982478913));
#50415=CARTESIAN_POINT('Origin',(14.,-68.7124355652982,-116.213429510899));
#50416=CARTESIAN_POINT('Origin',(14.,-70.3660254037844,-119.877531126037));
#50417=CARTESIAN_POINT('Origin',(57.5,-59.1970922754756,-125.765473267224));
#50418=CARTESIAN_POINT('',(57.5,-59.4850762228409,-125.08223311503));
#50419=CARTESIAN_POINT('',(58.,-59.0288384007668,-125.292242378034));
#50420=CARTESIAN_POINT('',(57.5,-59.4850762228408,-125.08223311503));
#50421=CARTESIAN_POINT('',(57.5,-59.1970922754756,-125.765473267224));
#50422=CARTESIAN_POINT('',(57.5,-59.1970922754756,-125.765473267224));
#50423=CARTESIAN_POINT('',(58.,-59.0288384007668,-125.292242378034));
#50424=CARTESIAN_POINT('Origin',(57.5,-57.5822796533797,-125.969521727281));
#50425=CARTESIAN_POINT('',(57.5,-58.2907844884389,-126.188091528965));
#50426=CARTESIAN_POINT('',(58.,-58.036420101407,-125.755014631118));
#50427=CARTESIAN_POINT('',(57.5,-58.2907844884389,-126.188091528965));
#50428=CARTESIAN_POINT('',(57.5,-57.5822796533797,-125.969521727281));
#50429=CARTESIAN_POINT('',(57.5,-57.5822796533797,-125.969521727281));
#50430=CARTESIAN_POINT('',(58.,-58.036420101407,-125.755014631118));
#50431=CARTESIAN_POINT('Origin',(14.,-59.0288384007668,-125.292242378034));
#50432=CARTESIAN_POINT('',(14.5,-59.4850762228408,-125.08223311503));
#50433=CARTESIAN_POINT('',(14.5,-59.1970922754756,-125.765473267224));
#50434=CARTESIAN_POINT('',(14.5,-59.4850762228409,-125.08223311503));
#50435=CARTESIAN_POINT('',(14.,-59.0288384007668,-125.292242378034));
#50436=CARTESIAN_POINT('',(14.,-59.0288384007668,-125.292242378034));
#50437=CARTESIAN_POINT('',(14.5,-59.1970922754756,-125.765473267224));
#50438=CARTESIAN_POINT('Origin',(14.25,-58.4380402379161,-122.84739093989));
#50439=CARTESIAN_POINT('',(14.,-58.2020747272541,-122.929975912966));
#50440=CARTESIAN_POINT('',(14.5,-58.674005748578,-122.764805966813));
#50441=CARTESIAN_POINT('Origin',(14.5,-57.5822796533797,-125.969521727281));
#50442=CARTESIAN_POINT('',(14.,-58.036420101407,-125.755014631118));
#50443=CARTESIAN_POINT('',(14.5,-58.2907844884389,-126.188091528965));
#50444=CARTESIAN_POINT('',(14.,-58.036420101407,-125.755014631118));
#50445=CARTESIAN_POINT('',(14.5,-57.5822796533797,-125.969521727281));
#50446=CARTESIAN_POINT('',(14.5,-57.5822796533797,-125.969521727281));
#50447=CARTESIAN_POINT('',(14.5,-58.2907844884389,-126.188091528965));
#50448=CARTESIAN_POINT('Origin',(14.25,-57.56981106276,-125.459008691224));
#50449=CARTESIAN_POINT('',(14.5,-57.3548715964828,-125.586684161994));
#50450=CARTESIAN_POINT('',(14.,-57.7847505290373,-125.331333220453));
#50451=CARTESIAN_POINT('Origin',(14.,-57.9365320709093,-126.078806628123));
#50452=CARTESIAN_POINT('',(14.,-58.2907844884389,-126.188091528965));
#50453=CARTESIAN_POINT('',(14.,-57.5822796533797,-125.969521727281));
#50454=CARTESIAN_POINT('Origin',(14.25,-59.0914377100404,-125.538896320465));
#50455=CARTESIAN_POINT('',(14.5,-59.1970922754756,-125.765473267224));
#50456=CARTESIAN_POINT('',(14.,-58.9857831446052,-125.312319373706));
#50457=CARTESIAN_POINT('Origin',(14.,-59.3410842491582,-125.423853191127));
#50458=CARTESIAN_POINT('',(14.,-59.4850762228409,-125.08223311503));
#50459=CARTESIAN_POINT('',(14.,-59.1970922754756,-125.765473267224));
#50460=CARTESIAN_POINT('Origin',(57.75,-57.56981106276,-125.459008691224));
#50461=CARTESIAN_POINT('',(58.,-57.7847505290373,-125.331333220453));
#50462=CARTESIAN_POINT('',(57.5,-57.3548715964828,-125.586684161994));
#50463=CARTESIAN_POINT('Origin',(57.75,-59.0914377100404,-125.538896320465));
#50464=CARTESIAN_POINT('',(58.,-58.9857831446052,-125.312319373706));
#50465=CARTESIAN_POINT('',(57.5,-59.1970922754756,-125.765473267224));
#50466=CARTESIAN_POINT('Origin',(57.75,-58.4380402379161,-122.84739093989));
#50467=CARTESIAN_POINT('',(57.5,-58.674005748578,-122.764805966813));
#50468=CARTESIAN_POINT('',(58.,-58.2020747272541,-122.929975912966));
#50469=CARTESIAN_POINT('Origin',(14.,-57.8987018584758,-124.164166824021));
#50470=CARTESIAN_POINT('Origin',(14.,-58.3222962368457,-121.759885683511));
#50471=CARTESIAN_POINT('Origin',(14.,-59.6502461689939,-125.554164136354));
#50472=CARTESIAN_POINT('Origin',(57.5,-46.3841944650247,-130.508796018164));
#50473=CARTESIAN_POINT('',(57.5,-47.070953611875,-130.788284360904));
#50474=CARTESIAN_POINT('',(58.,-46.8553022968291,-130.334686134323));
#50475=CARTESIAN_POINT('',(57.5,-47.070953611875,-130.788284360904));
#50476=CARTESIAN_POINT('',(57.5,-46.3841944650247,-130.508796018164));
#50477=CARTESIAN_POINT('',(57.5,-46.3841944650247,-130.508796018164));
#50478=CARTESIAN_POINT('',(58.,-46.8553022968291,-130.334686134323));
#50479=CARTESIAN_POINT('Origin',(14.,-46.7275740384498,-130.648540189534));
#50480=CARTESIAN_POINT('',(14.2512407024475,-46.7275740384498,-130.648540189534));
#50481=CARTESIAN_POINT('',(14.5,-46.3841944650247,-130.508796018164));
#50482=CARTESIAN_POINT('',(14.3353834448874,-46.6114260219129,-130.601271774103));
#50483=CARTESIAN_POINT('',(14.,-46.3841944650247,-130.508796018164));
#50484=CARTESIAN_POINT('',(14.5,-47.070953611875,-130.788284360904));
#50485=CARTESIAN_POINT('',(14.,-47.070953611875,-130.788284360904));
#50486=CARTESIAN_POINT('',(14.4305329766294,-46.975063500081,-130.749260245167));
#50487=CARTESIAN_POINT('Origin',(57.75,-46.4162674639966,-129.99913892906));
#50488=CARTESIAN_POINT('',(58.,-46.6415166711983,-129.890682510832));
#50489=CARTESIAN_POINT('',(57.5,-46.1910182567949,-130.107595347289));
#50490=CARTESIAN_POINT('Origin',(57.5,-48.0106462326609,-130.446264217578));
#50491=CARTESIAN_POINT('',(57.5,-48.3570826171013,-129.790723455271));
#50492=CARTESIAN_POINT('',(58.,-47.8842774043812,-129.960169823373));
#50493=CARTESIAN_POINT('',(57.5,-48.3570826171013,-129.790723455271));
#50494=CARTESIAN_POINT('',(57.5,-48.0106462326609,-130.446264217578));
#50495=CARTESIAN_POINT('',(57.5,-48.0106462326609,-130.446264217578));
#50496=CARTESIAN_POINT('',(58.,-47.8842774043812,-129.960169823373));
#50497=CARTESIAN_POINT('Origin',(14.,-48.1838644248811,-130.118493836425));
#50498=CARTESIAN_POINT('',(14.2512407024475,-48.1838644248811,-130.118493836425));
#50499=CARTESIAN_POINT('',(14.5,-48.0106462326609,-130.446264217578));
#50500=CARTESIAN_POINT('',(14.2590041943422,-48.1784584841,-130.128723173468));
#50501=CARTESIAN_POINT('',(14.,-48.0106462326609,-130.446264217578));
#50502=CARTESIAN_POINT('',(14.5,-48.3570826171013,-129.790723455271));
#50503=CARTESIAN_POINT('',(14.,-48.3570826171013,-129.790723455271));
#50504=CARTESIAN_POINT('',(14.6801520303733,-48.4825276128585,-129.553351424388));
#50505=CARTESIAN_POINT('Origin',(57.75,-47.9251411968295,-130.211341062382));
#50506=CARTESIAN_POINT('',(58.,-47.8396361609981,-129.976417907185));
#50507=CARTESIAN_POINT('',(57.5,-48.0106462326609,-130.446264217578));
#50508=CARTESIAN_POINT('Origin',(57.75,-47.5088102499061,-127.473130330375));
#50509=CARTESIAN_POINT('',(57.5,-47.7510755952283,-127.411425367399));
#50510=CARTESIAN_POINT('',(58.,-47.2665449045839,-127.534835293351));
#50511=CARTESIAN_POINT('Origin',(14.25,-46.4162674639966,-129.99913892906));
#50512=CARTESIAN_POINT('',(14.,-46.8553022968291,-130.334686134323));
#50513=CARTESIAN_POINT('',(14.5,-46.6011073014821,-130.959294432567));
#50514=CARTESIAN_POINT('',(14.,-46.6415166711983,-129.890682510832));
#50515=CARTESIAN_POINT('',(14.5,-46.1910182567949,-130.107595347289));
#50516=CARTESIAN_POINT('Origin',(14.,-48.4804925430539,-130.275254145916));
#50517=CARTESIAN_POINT('',(14.5,-48.0106462326609,-130.446264217578));
#50518=CARTESIAN_POINT('Origin',(14.25,-47.9251411968295,-130.211341062382));
#50519=CARTESIAN_POINT('',(14.,-47.8842774043812,-129.960169823373));
#50520=CARTESIAN_POINT('',(14.,-47.8842774043812,-129.960169823373));
#50521=CARTESIAN_POINT('',(14.,-47.8396361609981,-129.976417907185));
#50522=CARTESIAN_POINT('Origin',(14.25,-47.5088102499061,-127.473130330375));
#50523=CARTESIAN_POINT('',(14.5,-47.7510755952283,-127.411425367399));
#50524=CARTESIAN_POINT('',(14.,-47.2665449045839,-127.534835293351));
#50525=CARTESIAN_POINT('Origin',(14.,-47.4882890180656,-126.379675605442));
#50526=CARTESIAN_POINT('Origin',(14.,-46.6011073014821,-130.959294432567));
#50527=CARTESIAN_POINT('Origin',(57.5,-36.458810182395,-134.134280331629));
#50528=CARTESIAN_POINT('',(57.5,-36.8610624138408,-133.511428020236));
#50529=CARTESIAN_POINT('',(58.,-36.375288143631,-133.639021904261));
#50530=CARTESIAN_POINT('',(57.5,-36.8610624138408,-133.511428020236));
#50531=CARTESIAN_POINT('',(57.5,-36.458810182395,-134.134280331629));
#50532=CARTESIAN_POINT('',(57.5,-36.458810182395,-134.134280331629));
#50533=CARTESIAN_POINT('',(58.,-36.375288143631,-133.639021904261));
#50534=CARTESIAN_POINT('Origin',(57.5,-34.8330975492484,-134.054819567983));
#50535=CARTESIAN_POINT('',(57.5,-35.4928843561059,-134.393099376732));
#50536=CARTESIAN_POINT('',(58.,-35.3175873497673,-133.922431977811));
#50537=CARTESIAN_POINT('',(57.5,-35.4928843561059,-134.393099376732));
#50538=CARTESIAN_POINT('',(57.5,-34.8330975492484,-134.054819567983));
#50539=CARTESIAN_POINT('',(57.5,-34.8330975492484,-134.054819567983));
#50540=CARTESIAN_POINT('',(58.,-35.3175873497673,-133.922431977811));
#50541=CARTESIAN_POINT('Origin',(14.,-36.375288143631,-133.639021904261));
#50542=CARTESIAN_POINT('',(14.5,-36.8610624138408,-133.511428020236));
#50543=CARTESIAN_POINT('',(14.5,-36.458810182395,-134.134280331629));
#50544=CARTESIAN_POINT('',(14.5,-36.8610624138408,-133.511428020236));
#50545=CARTESIAN_POINT('',(14.,-36.375288143631,-133.639021904261));
#50546=CARTESIAN_POINT('',(14.,-36.375288143631,-133.639021904261));
#50547=CARTESIAN_POINT('',(14.5,-36.458810182395,-134.134280331629));
#50548=CARTESIAN_POINT('Origin',(14.25,-36.2180095292904,-131.128722228666));
#50549=CARTESIAN_POINT('',(14.,-35.9712881348696,-131.169077569515));
#50550=CARTESIAN_POINT('',(14.5,-36.4647309237111,-131.088366887817));
#50551=CARTESIAN_POINT('Origin',(14.5,-34.8330975492484,-134.054819567983));
#50552=CARTESIAN_POINT('',(14.,-35.3175873497673,-133.922431977811));
#50553=CARTESIAN_POINT('',(14.5,-35.4928843561059,-134.393099376732));
#50554=CARTESIAN_POINT('',(14.,-35.3175873497673,-133.922431977811));
#50555=CARTESIAN_POINT('',(14.5,-34.8330975492484,-134.054819567983));
#50556=CARTESIAN_POINT('',(14.5,-34.8330975492484,-134.054819567983));
#50557=CARTESIAN_POINT('',(14.5,-35.4928843561059,-134.393099376732));
#50558=CARTESIAN_POINT('Origin',(14.25,-34.9094680429236,-133.549897224021));
#50559=CARTESIAN_POINT('',(14.5,-34.6756233772734,-133.638309170877));
#50560=CARTESIAN_POINT('',(14.,-35.1433127085738,-133.461485277164));
#50561=CARTESIAN_POINT('Origin',(14.,-35.1629909526772,-134.223959472357));
#50562=CARTESIAN_POINT('',(14.,-35.4928843561059,-134.393099376732));
#50563=CARTESIAN_POINT('',(14.,-34.8330975492484,-134.054819567983));
#50564=CARTESIAN_POINT('Origin',(14.25,-36.3941054211193,-133.892798875057));
#50565=CARTESIAN_POINT('',(14.5,-36.458810182395,-134.134280331629));
#50566=CARTESIAN_POINT('',(14.,-36.3294006598437,-133.651317418485));
#50567=CARTESIAN_POINT('Origin',(14.,-36.6599362981179,-133.822854175933));
#50568=CARTESIAN_POINT('',(14.,-36.8610624138408,-133.511428020236));
#50569=CARTESIAN_POINT('',(14.,-36.458810182395,-134.134280331629));
#50570=CARTESIAN_POINT('Origin',(57.75,-34.9094680429236,-133.549897224021));
#50571=CARTESIAN_POINT('',(58.,-35.1433127085738,-133.461485277164));
#50572=CARTESIAN_POINT('',(57.5,-34.6756233772734,-133.638309170877));
#50573=CARTESIAN_POINT('Origin',(57.75,-36.3941054211193,-133.892798875057));
#50574=CARTESIAN_POINT('',(58.,-36.3294006598437,-133.651317418485));
#50575=CARTESIAN_POINT('',(57.5,-36.458810182395,-134.134280331629));
#50576=CARTESIAN_POINT('Origin',(57.75,-36.2180095292904,-131.128722228666));
#50577=CARTESIAN_POINT('',(57.5,-36.4647309237111,-131.088366887817));
#50578=CARTESIAN_POINT('',(58.,-35.9712881348696,-131.169077569515));
#50579=CARTESIAN_POINT('Origin',(14.,-35.4582091790454,-132.331838201602));
#50580=CARTESIAN_POINT('Origin',(14.,-36.292867245645,-130.037639885881));
#50581=CARTESIAN_POINT('Origin',(14.,-36.9417730955395,-134.004870809078));
#50582=CARTESIAN_POINT('Origin',(57.5,-24.6295005722095,-136.801453579863));
#50583=CARTESIAN_POINT('',(57.5,-25.0845072682929,-136.216030001563));
#50584=CARTESIAN_POINT('',(58.,-24.5894609761083,-136.30080033501));
#50585=CARTESIAN_POINT('',(57.5,-25.0845072682929,-136.216030001563));
#50586=CARTESIAN_POINT('',(57.5,-24.6295005722095,-136.801453579863));
#50587=CARTESIAN_POINT('',(57.5,-24.6295005722095,-136.801453579863));
#50588=CARTESIAN_POINT('',(58.,-24.5894609761083,-136.30080033501));
#50589=CARTESIAN_POINT('Origin',(57.5,-23.016899728323,-136.580604996376));
#50590=CARTESIAN_POINT('',(57.5,-23.6446928191973,-136.97510175753));
#50591=CARTESIAN_POINT('',(58.,-23.5110842376315,-136.490947249372));
#50592=CARTESIAN_POINT('',(57.5,-23.6446928191973,-136.97510175753));
#50593=CARTESIAN_POINT('',(57.5,-23.016899728323,-136.580604996376));
#50594=CARTESIAN_POINT('',(57.5,-23.016899728323,-136.580604996376));
#50595=CARTESIAN_POINT('',(58.,-23.5110842376315,-136.490947249372));
#50596=CARTESIAN_POINT('Origin',(14.,-24.5894609761083,-136.30080033501));
#50597=CARTESIAN_POINT('',(14.5,-25.0845072682929,-136.216030001563));
#50598=CARTESIAN_POINT('',(14.5,-24.6295005722095,-136.801453579863));
#50599=CARTESIAN_POINT('',(14.5,-25.0845072682929,-136.216030001563));
#50600=CARTESIAN_POINT('',(14.,-24.5894609761083,-136.30080033501));
#50601=CARTESIAN_POINT('',(14.,-24.5894609761083,-136.30080033501));
#50602=CARTESIAN_POINT('',(14.5,-24.6295005722095,-136.801453579863));
#50603=CARTESIAN_POINT('Origin',(14.25,-24.6515678871247,-133.786345373109));
#50604=CARTESIAN_POINT('',(14.,-24.4022681423913,-133.805043963321));
#50605=CARTESIAN_POINT('',(14.5,-24.900867631858,-133.767646782898));
#50606=CARTESIAN_POINT('Origin',(14.5,-23.016899728323,-136.580604996376));
#50607=CARTESIAN_POINT('',(14.,-23.5110842376315,-136.490947249372));
#50608=CARTESIAN_POINT('',(14.5,-23.6446928191973,-136.97510175753));
#50609=CARTESIAN_POINT('',(14.,-23.5110842376315,-136.490947249372));
#50610=CARTESIAN_POINT('',(14.5,-23.016899728323,-136.580604996376));
#50611=CARTESIAN_POINT('',(14.5,-23.016899728323,-136.580604996376));
#50612=CARTESIAN_POINT('',(14.5,-23.6446928191973,-136.97510175753));
#50613=CARTESIAN_POINT('Origin',(14.25,-23.1369864911308,-136.084260161474));
#50614=CARTESIAN_POINT('',(14.5,-22.896326066137,-136.151954768658));
#50615=CARTESIAN_POINT('',(14.,-23.3776469161246,-136.01656555429));
#50616=CARTESIAN_POINT('Origin',(14.,-23.3307962737602,-136.777853376953));
#50617=CARTESIAN_POINT('',(14.,-23.6446928191973,-136.97510175753));
#50618=CARTESIAN_POINT('',(14.,-23.016899728323,-136.580604996376));
#50619=CARTESIAN_POINT('Origin',(14.25,-24.5860885277927,-136.55525164161));
#50620=CARTESIAN_POINT('',(14.5,-24.6295005722095,-136.801453579863));
#50621=CARTESIAN_POINT('',(14.,-24.542676483376,-136.309049703357));
#50622=CARTESIAN_POINT('Origin',(14.,-24.8570039202512,-136.508741790713));
#50623=CARTESIAN_POINT('',(14.,-25.0845072682929,-136.216030001563));
#50624=CARTESIAN_POINT('',(14.,-24.6295005722095,-136.801453579863));
#50625=CARTESIAN_POINT('Origin',(57.75,-23.1369864911308,-136.084260161474));
#50626=CARTESIAN_POINT('',(58.,-23.3776469161246,-136.01656555429));
#50627=CARTESIAN_POINT('',(57.5,-22.896326066137,-136.151954768658));
#50628=CARTESIAN_POINT('Origin',(57.75,-24.5860885277927,-136.55525164161));
#50629=CARTESIAN_POINT('',(58.,-24.542676483376,-136.309049703357));
#50630=CARTESIAN_POINT('',(57.5,-24.6295005722095,-136.801453579863));
#50631=CARTESIAN_POINT('Origin',(57.75,-24.6515678871247,-133.786345373109));
#50632=CARTESIAN_POINT('',(57.5,-24.900867631858,-133.767646782898));
#50633=CARTESIAN_POINT('',(58.,-24.4022681423913,-133.805043963321));
#50634=CARTESIAN_POINT('Origin',(14.,-23.7898003403695,-134.918662162672));
#50635=CARTESIAN_POINT('Origin',(14.,-24.8212348392527,-132.705939207914));
#50636=CARTESIAN_POINT('Origin',(14.,-25.1219044487156,-136.71462949103));
#50637=CARTESIAN_POINT('Origin',(57.75,-12.8975129283142,-135.425773646859));
#50638=CARTESIAN_POINT('',(57.7487592975525,-12.864894733482,-138.155715454235));
#50639=CARTESIAN_POINT('',(58.,-12.6164931630349,-137.925247374536));
#50640=CARTESIAN_POINT('',(58.2319907935076,-12.3871239689705,-137.712437618128));
#50641=CARTESIAN_POINT('',(58.,-12.647532154857,-135.422673178871));
#50642=CARTESIAN_POINT('',(57.5,-13.1170438759937,-137.883945745091));
#50643=CARTESIAN_POINT('',(57.5,-13.1474937017714,-135.428874114848));
#50644=CARTESIAN_POINT('',(50.4896657310027,-20.2229080267582,-130.225150580314));
#50645=CARTESIAN_POINT('Origin',(58.,-11.9403367564292,-136.478673638569));
#50646=CARTESIAN_POINT('',(58.,-11.5256475780664,-138.020683996878));
#50647=CARTESIAN_POINT('',(58.,-12.5691677195965,-137.929387814333));
#50648=CARTESIAN_POINT('',(58.,-11.4340631148344,-137.536477638499));
#50649=CARTESIAN_POINT('Origin',(57.75,-12.5909566552834,-138.178436488856));
#50650=CARTESIAN_POINT('',(57.5,-12.6127455909704,-138.427485163379));
#50651=CARTESIAN_POINT('',(57.5,-12.6127455909704,-138.427485163379));
#50652=CARTESIAN_POINT('',(57.5,-11.6165508928786,-138.514640906126));
#50653=CARTESIAN_POINT('',(57.5,-12.6127455909704,-138.427485163379));
#50654=CARTESIAN_POINT('',(57.5,-11.6165508928786,-138.514640906126));
#50655=CARTESIAN_POINT('Origin',(14.,-12.864894733482,-138.155715454235));
#50656=CARTESIAN_POINT('',(14.5,-13.1170438759937,-137.883945745091));
#50657=CARTESIAN_POINT('',(14.,-13.1170438759937,-137.883945745091));
#50658=CARTESIAN_POINT('',(14.5,-12.6127455909704,-138.427485163379));
#50659=CARTESIAN_POINT('',(14.5,-13.1170438759937,-137.883945745091));
#50660=CARTESIAN_POINT('',(14.,-12.6127455909704,-138.427485163379));
#50661=CARTESIAN_POINT('Origin',(57.5,-11.025529402481,-138.066929551123));
#50662=CARTESIAN_POINT('',(57.5,-11.025529402481,-138.066929551123));
#50663=CARTESIAN_POINT('',(57.5,-11.025529402481,-138.066929551123));
#50664=CARTESIAN_POINT('',(58.,-11.5256475780664,-138.020683996878));
#50665=CARTESIAN_POINT('Origin',(14.,-12.6164931630349,-137.925247374536));
#50666=CARTESIAN_POINT('',(14.,-12.6164931630349,-137.925247374536));
#50667=CARTESIAN_POINT('',(14.,-12.6164931630349,-137.925247374536));
#50668=CARTESIAN_POINT('',(14.5,-12.6127455909704,-138.427485163379));
#50669=CARTESIAN_POINT('Origin',(14.25,-12.8975129283142,-135.425773646859));
#50670=CARTESIAN_POINT('',(14.,-12.647532154857,-135.422673178871));
#50671=CARTESIAN_POINT('',(14.5,-13.1474937017714,-135.428874114848));
#50672=CARTESIAN_POINT('Origin',(14.5,-11.025529402481,-138.066929551123));
#50673=CARTESIAN_POINT('',(14.,-11.5256475780664,-138.020683996878));
#50674=CARTESIAN_POINT('',(14.5,-11.6165508928786,-138.514640906126));
#50675=CARTESIAN_POINT('',(14.,-11.5256475780664,-138.020683996878));
#50676=CARTESIAN_POINT('',(14.5,-11.025529402481,-138.066929551123));
#50677=CARTESIAN_POINT('',(14.5,-11.025529402481,-138.066929551123));
#50678=CARTESIAN_POINT('',(14.5,-11.6165508928786,-138.514640906126));
#50679=CARTESIAN_POINT('Origin',(14.25,-11.188418501646,-137.582939709175));
#50680=CARTESIAN_POINT('',(14.5,-10.9427738884575,-137.629401779851));
#50681=CARTESIAN_POINT('',(14.,-11.4340631148344,-137.536477638499));
#50682=CARTESIAN_POINT('Origin',(14.,-11.3210401476798,-138.290785228625));
#50683=CARTESIAN_POINT('',(14.,-11.6165508928786,-138.514640906126));
#50684=CARTESIAN_POINT('',(14.,-11.025529402481,-138.066929551123));
#50685=CARTESIAN_POINT('Origin',(14.25,-12.5909566552834,-138.178436488856));
#50686=CARTESIAN_POINT('',(14.5,-12.6127455909704,-138.427485163379));
#50687=CARTESIAN_POINT('',(14.,-12.5691677195965,-137.929387814333));
#50688=CARTESIAN_POINT('Origin',(57.75,-11.188418501646,-137.582939709175));
#50689=CARTESIAN_POINT('',(57.5,-10.9427738884575,-137.629401779851));
#50690=CARTESIAN_POINT('Origin',(14.,-13.1606978482623,-134.364266202539));
#50691=CARTESIAN_POINT('Origin',(14.,-13.1108429400162,-138.383907292005));
#50692=CARTESIAN_POINT('Origin',(57.5,-0.500000000000016,-139.));
#50693=CARTESIAN_POINT('',(57.5,-1.04975185951052,-138.502481404895));
#50694=CARTESIAN_POINT('',(58.,-0.547506218943973,-138.5));
#50695=CARTESIAN_POINT('',(57.5,-1.04975185951052,-138.502481404895));
#50696=CARTESIAN_POINT('',(57.5,-0.500000000000016,-139.));
#50697=CARTESIAN_POINT('',(57.5,-0.500000000000016,-139.));
#50698=CARTESIAN_POINT('',(58.,-0.547506218943973,-138.5));
#50699=CARTESIAN_POINT('Origin',(57.5,1.04975185951048,-138.502481404895));
#50700=CARTESIAN_POINT('',(57.5,0.499999999999983,-139.));
#50701=CARTESIAN_POINT('',(58.,0.54750621894394,-138.5));
#50702=CARTESIAN_POINT('',(57.5,0.499999999999983,-139.));
#50703=CARTESIAN_POINT('',(57.5,1.04975185951048,-138.502481404895));
#50704=CARTESIAN_POINT('',(57.5,1.04975185951048,-138.502481404895));
#50705=CARTESIAN_POINT('',(58.,0.54750621894394,-138.5));
#50706=CARTESIAN_POINT('Origin',(14.,-0.547506218943975,-138.5));
#50707=CARTESIAN_POINT('',(14.5,-1.04975185951052,-138.502481404895));
#50708=CARTESIAN_POINT('',(14.5,-0.500000000000016,-139.));
#50709=CARTESIAN_POINT('',(14.5,-1.04975185951052,-138.502481404895));
#50710=CARTESIAN_POINT('',(14.,-0.547506218943975,-138.5));
#50711=CARTESIAN_POINT('',(14.,-0.547506218943975,-138.5));
#50712=CARTESIAN_POINT('',(14.5,-0.500000000000016,-139.));
#50713=CARTESIAN_POINT('Origin',(14.25,-1.04530010838811,-136.034530010839));
#50714=CARTESIAN_POINT('',(14.,-0.796540810835615,-136.009654081084));
#50715=CARTESIAN_POINT('',(14.5,-1.29405940594061,-136.059405940594));
#50716=CARTESIAN_POINT('Origin',(14.5,1.04975185951048,-138.502481404895));
#50717=CARTESIAN_POINT('',(14.,0.54750621894394,-138.5));
#50718=CARTESIAN_POINT('',(14.5,0.499999999999983,-139.));
#50719=CARTESIAN_POINT('',(14.,0.547506218943941,-138.5));
#50720=CARTESIAN_POINT('',(14.5,1.04975185951048,-138.502481404895));
#50721=CARTESIAN_POINT('',(14.5,1.04975185951048,-138.502481404895));
#50722=CARTESIAN_POINT('',(14.5,0.499999999999983,-139.));
#50723=CARTESIAN_POINT('Origin',(14.25,0.84530010838808,-138.034530010839));
#50724=CARTESIAN_POINT('',(14.5,1.09405940594058,-138.059405940594));
#50725=CARTESIAN_POINT('',(14.,0.596540810835583,-138.009654081084));
#50726=CARTESIAN_POINT('Origin',(14.,0.774875929755232,-138.751240702448));
#50727=CARTESIAN_POINT('',(14.,0.499999999999983,-139.));
#50728=CARTESIAN_POINT('',(14.,1.04975185951048,-138.502481404895));
#50729=CARTESIAN_POINT('Origin',(14.25,-0.500000000000017,-138.75));
#50730=CARTESIAN_POINT('',(14.5,-0.500000000000017,-139.));
#50731=CARTESIAN_POINT('',(14.,-0.500000000000017,-138.5));
#50732=CARTESIAN_POINT('Origin',(14.,-0.774875929755266,-138.751240702448));
#50733=CARTESIAN_POINT('',(14.,-1.04975185951052,-138.502481404895));
#50734=CARTESIAN_POINT('',(14.,-0.500000000000016,-139.));
#50735=CARTESIAN_POINT('Origin',(57.75,0.845300108388081,-138.034530010839));
#50736=CARTESIAN_POINT('',(58.,0.596540810835584,-138.009654081084));
#50737=CARTESIAN_POINT('',(57.5,1.09405940594058,-138.059405940594));
#50738=CARTESIAN_POINT('Origin',(57.75,-0.500000000000017,-138.75));
#50739=CARTESIAN_POINT('',(58.,-0.500000000000017,-138.5));
#50740=CARTESIAN_POINT('',(57.5,-0.500000000000017,-139.));
#50741=CARTESIAN_POINT('Origin',(57.75,-1.04530010838811,-136.034530010839));
#50742=CARTESIAN_POINT('',(57.5,-1.29405940594061,-136.059405940594));
#50743=CARTESIAN_POINT('',(58.,-0.796540810835615,-136.009654081084));
#50744=CARTESIAN_POINT('Origin',(14.,-1.67776611483187E-14,-137.));
#50745=CARTESIAN_POINT('Origin',(14.,-1.40000000000002,-135.));
#50746=CARTESIAN_POINT('Origin',(14.,-1.00000000000002,-139.));
#50747=CARTESIAN_POINT('Origin',(57.5,13.1170438759936,-137.883945745091));
#50748=CARTESIAN_POINT('',(57.5,12.6127455909703,-138.427485163379));
#50749=CARTESIAN_POINT('',(58.,12.6164931630349,-137.925247374536));
#50750=CARTESIAN_POINT('',(57.5,12.6127455909703,-138.427485163379));
#50751=CARTESIAN_POINT('',(57.5,13.1170438759936,-137.883945745091));
#50752=CARTESIAN_POINT('',(57.5,13.1170438759936,-137.883945745091));
#50753=CARTESIAN_POINT('',(58.,12.6164931630349,-137.925247374536));
#50754=CARTESIAN_POINT('Origin',(14.,12.864894733482,-138.155715454235));
#50755=CARTESIAN_POINT('',(14.2512407024475,12.864894733482,-138.155715454235));
#50756=CARTESIAN_POINT('',(14.5,13.1170438759936,-137.883945745091));
#50757=CARTESIAN_POINT('',(14.3353834448875,12.9501840897535,-138.063789448395));
#50758=CARTESIAN_POINT('',(14.,13.1170438759936,-137.883945745091));
#50759=CARTESIAN_POINT('',(14.5,12.6127455909703,-138.427485163379));
#50760=CARTESIAN_POINT('',(14.,12.6127455909703,-138.427485163379));
#50761=CARTESIAN_POINT('',(14.4305329766294,12.6831592420301,-138.351592391039));
#50762=CARTESIAN_POINT('Origin',(57.75,12.8725854741911,-137.435594191592));
#50763=CARTESIAN_POINT('',(58.,12.622604700734,-137.432493723604));
#50764=CARTESIAN_POINT('',(57.5,13.1225662476483,-137.438694659581));
#50765=CARTESIAN_POINT('Origin',(57.5,11.6165508928786,-138.514640906126));
#50766=CARTESIAN_POINT('',(57.5,11.025529402481,-138.066929551123));
#50767=CARTESIAN_POINT('',(58.,11.5256475780664,-138.020683996878));
#50768=CARTESIAN_POINT('',(57.5,11.025529402481,-138.066929551123));
#50769=CARTESIAN_POINT('',(57.5,11.6165508928786,-138.514640906126));
#50770=CARTESIAN_POINT('',(57.5,11.6165508928786,-138.514640906126));
#50771=CARTESIAN_POINT('',(58.,11.5256475780664,-138.020683996878));
#50772=CARTESIAN_POINT('Origin',(14.,11.3210401476798,-138.290785228625));
#50773=CARTESIAN_POINT('',(14.2512407024475,11.3210401476798,-138.290785228625));
#50774=CARTESIAN_POINT('',(14.5,11.6165508928786,-138.514640906126));
#50775=CARTESIAN_POINT('',(14.2590041943422,11.3302626985461,-138.297771507148));
#50776=CARTESIAN_POINT('',(14.,11.6165508928786,-138.514640906126));
#50777=CARTESIAN_POINT('',(14.5,11.025529402481,-138.066929551123));
#50778=CARTESIAN_POINT('',(14.,11.025529402481,-138.066929551123));
#50779=CARTESIAN_POINT('',(14.6801520303733,10.8115198709038,-137.90481277716));
#50780=CARTESIAN_POINT('Origin',(57.75,11.5947619571917,-138.265592231604));
#50781=CARTESIAN_POINT('',(58.,11.5729730215048,-138.016543557081));
#50782=CARTESIAN_POINT('',(57.5,11.6165508928786,-138.514640906126));
#50783=CARTESIAN_POINT('Origin',(57.75,10.8148680765323,-135.607981461541));
#50784=CARTESIAN_POINT('',(57.5,10.5692234633438,-135.654443532217));
#50785=CARTESIAN_POINT('',(58.,11.0605126897207,-135.561519390865));
#50786=CARTESIAN_POINT('Origin',(14.25,12.8725854741911,-137.435594191592));
#50787=CARTESIAN_POINT('',(14.,12.6164931630349,-137.925247374536));
#50788=CARTESIAN_POINT('',(14.5,13.1108429400162,-138.383907292005));
#50789=CARTESIAN_POINT('',(14.,12.622604700734,-137.432493723604));
#50790=CARTESIAN_POINT('',(14.5,13.1225662476483,-137.438694659581));
#50791=CARTESIAN_POINT('Origin',(14.,11.1184535438327,-138.5582187775));
#50792=CARTESIAN_POINT('',(14.5,11.6165508928786,-138.514640906126));
#50793=CARTESIAN_POINT('Origin',(14.25,11.5947619571917,-138.265592231604));
#50794=CARTESIAN_POINT('',(14.,11.5256475780664,-138.020683996878));
#50795=CARTESIAN_POINT('',(14.,11.5256475780664,-138.020683996878));
#50796=CARTESIAN_POINT('',(14.,11.5729730215048,-138.016543557081));
#50797=CARTESIAN_POINT('Origin',(14.25,10.8148680765323,-135.607981461541));
#50798=CARTESIAN_POINT('',(14.5,10.5692234633438,-135.654443532217));
#50799=CARTESIAN_POINT('',(14.,11.0605126897207,-135.561519390865));
#50800=CARTESIAN_POINT('Origin',(14.,10.3713526936054,-134.608302282232));
#50801=CARTESIAN_POINT('Origin',(14.,13.1108429400162,-138.383907292005));
#50802=CARTESIAN_POINT('Origin',(57.5,23.6446928191972,-136.97510175753));
#50803=CARTESIAN_POINT('',(57.5,23.016899728323,-136.580604996376));
#50804=CARTESIAN_POINT('',(58.,23.5110842376314,-136.490947249372));
#50805=CARTESIAN_POINT('',(57.5,23.016899728323,-136.580604996376));
#50806=CARTESIAN_POINT('',(57.5,23.6446928191972,-136.97510175753));
#50807=CARTESIAN_POINT('',(57.5,23.6446928191972,-136.97510175753));
#50808=CARTESIAN_POINT('',(58.,23.5110842376314,-136.490947249372));
#50809=CARTESIAN_POINT('Origin',(57.5,25.0845072682928,-136.216030001563));
#50810=CARTESIAN_POINT('',(57.5,24.6295005722094,-136.801453579863));
#50811=CARTESIAN_POINT('',(58.,24.5894609761082,-136.30080033501));
#50812=CARTESIAN_POINT('',(57.5,24.6295005722094,-136.801453579863));
#50813=CARTESIAN_POINT('',(57.5,25.0845072682928,-136.216030001563));
#50814=CARTESIAN_POINT('',(57.5,25.0845072682928,-136.216030001563));
#50815=CARTESIAN_POINT('',(58.,24.5894609761082,-136.30080033501));
#50816=CARTESIAN_POINT('Origin',(14.,23.5110842376314,-136.490947249372));
#50817=CARTESIAN_POINT('',(14.5,23.016899728323,-136.580604996376));
#50818=CARTESIAN_POINT('',(14.5,23.6446928191972,-136.97510175753));
#50819=CARTESIAN_POINT('',(14.5,23.016899728323,-136.580604996376));
#50820=CARTESIAN_POINT('',(14.,23.5110842376314,-136.490947249372));
#50821=CARTESIAN_POINT('',(14.,23.5110842376314,-136.490947249372));
#50822=CARTESIAN_POINT('',(14.5,23.6446928191972,-136.97510175753));
#50823=CARTESIAN_POINT('Origin',(14.25,22.5927285851944,-134.149374290983));
#50824=CARTESIAN_POINT('',(14.,22.8333890101882,-134.081679683799));
#50825=CARTESIAN_POINT('',(14.5,22.3520681602006,-134.217068898167));
#50826=CARTESIAN_POINT('Origin',(14.5,25.0845072682928,-136.216030001563));
#50827=CARTESIAN_POINT('',(14.,24.5894609761082,-136.30080033501));
#50828=CARTESIAN_POINT('',(14.5,24.6295005722094,-136.801453579863));
#50829=CARTESIAN_POINT('',(14.,24.5894609761082,-136.30080033501));
#50830=CARTESIAN_POINT('',(14.5,25.0845072682928,-136.216030001563));
#50831=CARTESIAN_POINT('',(14.5,25.0845072682928,-136.216030001563));
#50832=CARTESIAN_POINT('',(14.5,24.6295005722094,-136.801453579863));
#50833=CARTESIAN_POINT('Origin',(14.25,24.801902691856,-135.790690514667));
#50834=CARTESIAN_POINT('',(14.5,25.0512024365893,-135.771991924456));
#50835=CARTESIAN_POINT('',(14.,24.5526029471226,-135.809389104878));
#50836=CARTESIAN_POINT('Origin',(14.,24.8570039202511,-136.508741790713));
#50837=CARTESIAN_POINT('',(14.,24.6295005722094,-136.801453579863));
#50838=CARTESIAN_POINT('',(14.,25.0845072682928,-136.216030001563));
#50839=CARTESIAN_POINT('Origin',(14.25,23.6012807747804,-136.728899819277));
#50840=CARTESIAN_POINT('',(14.5,23.6446928191972,-136.97510175753));
#50841=CARTESIAN_POINT('',(14.,23.5578687303637,-136.482697881024));
#50842=CARTESIAN_POINT('Origin',(14.,23.3307962737601,-136.777853376953));
#50843=CARTESIAN_POINT('',(14.,23.016899728323,-136.580604996376));
#50844=CARTESIAN_POINT('',(14.,23.6446928191972,-136.97510175753));
#50845=CARTESIAN_POINT('Origin',(57.75,24.801902691856,-135.790690514667));
#50846=CARTESIAN_POINT('',(58.,24.5526029471226,-135.809389104878));
#50847=CARTESIAN_POINT('',(57.5,25.0512024365893,-135.771991924456));
#50848=CARTESIAN_POINT('Origin',(57.75,23.6012807747804,-136.728899819277));
#50849=CARTESIAN_POINT('',(58.,23.5578687303637,-136.482697881024));
#50850=CARTESIAN_POINT('',(57.5,23.6446928191972,-136.97510175753));
#50851=CARTESIAN_POINT('Origin',(57.75,22.5927285851944,-134.149374290983));
#50852=CARTESIAN_POINT('',(57.5,22.3520681602006,-134.217068898167));
#50853=CARTESIAN_POINT('',(58.,22.8333890101882,-134.081679683799));
#50854=CARTESIAN_POINT('Origin',(14.,23.7898003403694,-134.918662162673));
#50855=CARTESIAN_POINT('Origin',(14.,22.0637731308185,-133.192154105382));
#50856=CARTESIAN_POINT('Origin',(14.,23.1522889426911,-137.061925846364));
#50857=CARTESIAN_POINT('Origin',(57.5,35.4928843561059,-134.393099376732));
#50858=CARTESIAN_POINT('',(57.5,34.8330975492484,-134.054819567983));
#50859=CARTESIAN_POINT('',(58.,35.3175873497673,-133.922431977811));
#50860=CARTESIAN_POINT('',(57.5,34.8330975492484,-134.054819567983));
#50861=CARTESIAN_POINT('',(57.5,35.4928843561059,-134.393099376732));
#50862=CARTESIAN_POINT('',(57.5,35.4928843561059,-134.393099376732));
#50863=CARTESIAN_POINT('',(58.,35.3175873497673,-133.922431977811));
#50864=CARTESIAN_POINT('Origin',(57.5,36.8610624138407,-133.511428020236));
#50865=CARTESIAN_POINT('',(57.5,36.4588101823949,-134.134280331629));
#50866=CARTESIAN_POINT('',(58.,36.375288143631,-133.639021904261));
#50867=CARTESIAN_POINT('',(57.5,36.4588101823949,-134.134280331629));
#50868=CARTESIAN_POINT('',(57.5,36.8610624138407,-133.511428020236));
#50869=CARTESIAN_POINT('',(57.5,36.8610624138407,-133.511428020236));
#50870=CARTESIAN_POINT('',(58.,36.375288143631,-133.639021904261));
#50871=CARTESIAN_POINT('Origin',(14.,35.3175873497673,-133.922431977811));
#50872=CARTESIAN_POINT('',(14.5,34.8330975492484,-134.054819567983));
#50873=CARTESIAN_POINT('',(14.5,35.4928843561059,-134.393099376732));
#50874=CARTESIAN_POINT('',(14.5,34.8330975492484,-134.054819567983));
#50875=CARTESIAN_POINT('',(14.,35.3175873497673,-133.922431977811));
#50876=CARTESIAN_POINT('',(14.,35.3175873497673,-133.922431977811));
#50877=CARTESIAN_POINT('',(14.5,35.4928843561059,-134.393099376732));
#50878=CARTESIAN_POINT('Origin',(14.25,34.1986447874607,-131.669809380463));
#50879=CARTESIAN_POINT('',(14.,34.4324894531109,-131.581397433607));
#50880=CARTESIAN_POINT('',(14.5,33.9648001218105,-131.75822132732));
#50881=CARTESIAN_POINT('Origin',(14.5,36.8610624138407,-133.511428020236));
#50882=CARTESIAN_POINT('',(14.,36.375288143631,-133.639021904261));
#50883=CARTESIAN_POINT('',(14.5,36.4588101823949,-134.134280331629));
#50884=CARTESIAN_POINT('',(14.,36.375288143631,-133.639021904261));
#50885=CARTESIAN_POINT('',(14.5,36.8610624138407,-133.511428020236));
#50886=CARTESIAN_POINT('',(14.5,36.8610624138407,-133.511428020236));
#50887=CARTESIAN_POINT('',(14.5,36.4588101823949,-134.134280331629));
#50888=CARTESIAN_POINT('Origin',(14.25,36.5424624542376,-133.112337690265));
#50889=CARTESIAN_POINT('',(14.5,36.7891838486583,-133.071982349415));
#50890=CARTESIAN_POINT('',(14.,36.2957410598168,-133.152693031114));
#50891=CARTESIAN_POINT('Origin',(14.,36.6599362981178,-133.822854175933));
#50892=CARTESIAN_POINT('',(14.,36.4588101823949,-134.134280331629));
#50893=CARTESIAN_POINT('',(14.,36.8610624138407,-133.511428020236));
#50894=CARTESIAN_POINT('Origin',(14.25,35.4281795948302,-134.151617920159));
#50895=CARTESIAN_POINT('',(14.5,35.4928843561059,-134.393099376732));
#50896=CARTESIAN_POINT('',(14.,35.3634748335546,-133.910136463587));
#50897=CARTESIAN_POINT('Origin',(14.,35.1629909526771,-134.223959472357));
#50898=CARTESIAN_POINT('',(14.,34.8330975492484,-134.054819567983));
#50899=CARTESIAN_POINT('',(14.,35.4928843561059,-134.393099376732));
#50900=CARTESIAN_POINT('Origin',(57.75,36.5424624542376,-133.112337690265));
#50901=CARTESIAN_POINT('',(58.,36.2957410598168,-133.152693031114));
#50902=CARTESIAN_POINT('',(57.5,36.7891838486583,-133.071982349415));
#50903=CARTESIAN_POINT('Origin',(57.75,35.4281795948302,-134.151617920159));
#50904=CARTESIAN_POINT('',(58.,35.3634748335546,-133.910136463587));
#50905=CARTESIAN_POINT('',(57.5,35.4928843561059,-134.393099376732));
#50906=CARTESIAN_POINT('Origin',(57.75,34.1986447874607,-131.669809380463));
#50907=CARTESIAN_POINT('',(57.5,33.9648001218105,-131.75822132732));
#50908=CARTESIAN_POINT('',(58.,34.4324894531109,-131.581397433607));
#50909=CARTESIAN_POINT('Origin',(14.,35.4582091790453,-132.331838201602));
#50910=CARTESIAN_POINT('Origin',(14.,33.5882749320356,-130.762333212168));
#50911=CARTESIAN_POINT('Origin',(14.,35.0099214429613,-134.522508899283));
#50912=CARTESIAN_POINT('Origin',(57.75,45.5442886531881,-128.188157716154));
#50913=CARTESIAN_POINT('',(57.7487592975525,46.7275740384498,-130.648540189534));
#50914=CARTESIAN_POINT('',(58.,46.8553022968291,-130.334686134323));
#50915=CARTESIAN_POINT('',(58.2319907935076,46.9732440941815,-130.044879384841));
#50916=CARTESIAN_POINT('',(58.,45.7695378603898,-128.079701297925));
#50917=CARTESIAN_POINT('',(57.5,46.3841944650246,-130.508796018164));
#50918=CARTESIAN_POINT('',(57.5,45.3190394459863,-128.296614134382));
#50919=CARTESIAN_POINT('',(50.4896657310026,36.7073477519961,-126.570638276569));
#50920=CARTESIAN_POINT('Origin',(58.,46.8567596356166,-128.737889047669));
#50921=CARTESIAN_POINT('',(58.,47.8842774043812,-129.960169823373));
#50922=CARTESIAN_POINT('',(58.,46.8999435402121,-130.318438050511));
#50923=CARTESIAN_POINT('',(58.,47.762646667078,-129.482624563588));
#50924=CARTESIAN_POINT('Origin',(57.75,46.9854485760436,-130.553361205708));
#50925=CARTESIAN_POINT('',(57.5,47.070953611875,-130.788284360904));
#50926=CARTESIAN_POINT('',(57.5,47.070953611875,-130.788284360904));
#50927=CARTESIAN_POINT('',(57.5,48.0106462326609,-130.446264217578));
#50928=CARTESIAN_POINT('',(57.5,47.070953611875,-130.788284360904));
#50929=CARTESIAN_POINT('',(57.5,48.0106462326609,-130.446264217578));
#50930=CARTESIAN_POINT('Origin',(14.,46.7275740384498,-130.648540189534));
#50931=CARTESIAN_POINT('',(14.5,46.3841944650246,-130.508796018164));
#50932=CARTESIAN_POINT('',(14.,46.3841944650246,-130.508796018164));
#50933=CARTESIAN_POINT('',(14.5,47.070953611875,-130.788284360904));
#50934=CARTESIAN_POINT('',(14.5,46.3841944650246,-130.508796018164));
#50935=CARTESIAN_POINT('',(14.,47.070953611875,-130.788284360904));
#50936=CARTESIAN_POINT('Origin',(57.5,48.3570826171013,-129.790723455271));
#50937=CARTESIAN_POINT('',(57.5,48.3570826171013,-129.790723455271));
#50938=CARTESIAN_POINT('',(57.5,48.3570826171013,-129.790723455271));
#50939=CARTESIAN_POINT('',(58.,47.8842774043812,-129.960169823373));
#50940=CARTESIAN_POINT('Origin',(14.,46.8553022968291,-130.334686134323));
#50941=CARTESIAN_POINT('',(14.,46.8553022968291,-130.334686134323));
#50942=CARTESIAN_POINT('',(14.,46.8553022968291,-130.334686134323));
#50943=CARTESIAN_POINT('',(14.5,47.070953611875,-130.788284360904));
#50944=CARTESIAN_POINT('Origin',(14.25,45.544288653188,-128.188157716154));
#50945=CARTESIAN_POINT('',(14.,45.7695378603898,-128.079701297925));
#50946=CARTESIAN_POINT('',(14.5,45.3190394459863,-128.296614134382));
#50947=CARTESIAN_POINT('Origin',(14.5,48.3570826171013,-129.790723455271));
#50948=CARTESIAN_POINT('',(14.,47.8842774043812,-129.960169823373));
#50949=CARTESIAN_POINT('',(14.5,48.0106462326609,-130.446264217578));
#50950=CARTESIAN_POINT('',(14.,47.8842774043812,-129.960169823373));
#50951=CARTESIAN_POINT('',(14.5,48.3570826171013,-129.790723455271));
#50952=CARTESIAN_POINT('',(14.5,48.3570826171013,-129.790723455271));
#50953=CARTESIAN_POINT('',(14.5,48.0106462326609,-130.446264217578));
#50954=CARTESIAN_POINT('Origin',(14.25,48.0049120124002,-129.420919600612));
#50955=CARTESIAN_POINT('',(14.5,48.2471773577224,-129.359214637636));
#50956=CARTESIAN_POINT('',(14.,47.762646667078,-129.482624563588));
#50957=CARTESIAN_POINT('Origin',(14.,48.1838644248811,-130.118493836425));
#50958=CARTESIAN_POINT('',(14.,48.0106462326609,-130.446264217578));
#50959=CARTESIAN_POINT('',(14.,48.3570826171013,-129.790723455271));
#50960=CARTESIAN_POINT('Origin',(14.25,46.9854485760436,-130.553361205708));
#50961=CARTESIAN_POINT('',(14.5,47.070953611875,-130.788284360904));
#50962=CARTESIAN_POINT('',(14.,46.8999435402122,-130.318438050511));
#50963=CARTESIAN_POINT('Origin',(57.75,48.0049120124002,-129.420919600612));
#50964=CARTESIAN_POINT('',(57.5,48.2471773577224,-129.359214637636));
#50965=CARTESIAN_POINT('Origin',(14.,44.857149679865,-127.337332006754));
#50966=CARTESIAN_POINT('Origin',(14.,46.601107301482,-130.959294432567));
#50967=CARTESIAN_POINT('Origin',(57.5,58.2907844884389,-126.188091528965));
#50968=CARTESIAN_POINT('',(57.5,57.5822796533797,-125.969521727281));
#50969=CARTESIAN_POINT('',(58.,58.036420101407,-125.755014631118));
#50970=CARTESIAN_POINT('',(57.5,57.5822796533797,-125.969521727281));
#50971=CARTESIAN_POINT('',(57.5,58.2907844884389,-126.188091528965));
#50972=CARTESIAN_POINT('',(57.5,58.2907844884389,-126.188091528965));
#50973=CARTESIAN_POINT('',(58.,58.036420101407,-125.755014631118));
#50974=CARTESIAN_POINT('Origin',(57.5,59.4850762228408,-125.08223311503));
#50975=CARTESIAN_POINT('',(57.5,59.1970922754755,-125.765473267224));
#50976=CARTESIAN_POINT('',(58.,59.0288384007667,-125.292242378034));
#50977=CARTESIAN_POINT('',(57.5,59.1970922754755,-125.765473267224));
#50978=CARTESIAN_POINT('',(57.5,59.4850762228408,-125.08223311503));
#50979=CARTESIAN_POINT('',(57.5,59.4850762228408,-125.08223311503));
#50980=CARTESIAN_POINT('',(58.,59.0288384007667,-125.292242378034));
#50981=CARTESIAN_POINT('Origin',(14.,58.0364201014069,-125.755014631118));
#50982=CARTESIAN_POINT('',(14.5,57.5822796533797,-125.969521727281));
#50983=CARTESIAN_POINT('',(14.5,58.2907844884389,-126.188091528965));
#50984=CARTESIAN_POINT('',(14.5,57.5822796533797,-125.969521727281));
#50985=CARTESIAN_POINT('',(14.,58.0364201014069,-125.755014631118));
#50986=CARTESIAN_POINT('',(14.,58.0364201014069,-125.755014631118));
#50987=CARTESIAN_POINT('',(14.5,58.2907844884389,-126.188091528965));
#50988=CARTESIAN_POINT('Origin',(14.25,56.5433129818713,-123.730916769498));
#50989=CARTESIAN_POINT('',(14.,56.7582524481486,-123.603241298728));
#50990=CARTESIAN_POINT('',(14.5,56.3283735155941,-123.858592240269));
#50991=CARTESIAN_POINT('Origin',(14.5,59.4850762228408,-125.08223311503));
#50992=CARTESIAN_POINT('',(14.,59.0288384007667,-125.292242378034));
#50993=CARTESIAN_POINT('',(14.5,59.1970922754755,-125.765473267224));
#50994=CARTESIAN_POINT('',(14.,59.0288384007667,-125.292242378034));
#50995=CARTESIAN_POINT('',(14.5,59.4850762228408,-125.08223311503));
#50996=CARTESIAN_POINT('',(14.5,59.4850762228408,-125.08223311503));
#50997=CARTESIAN_POINT('',(14.5,59.1970922754755,-125.765473267224));
#50998=CARTESIAN_POINT('Origin',(14.25,59.1020152039901,-124.744530166311));
#50999=CARTESIAN_POINT('',(14.5,59.3379807146521,-124.661945193235));
#51000=CARTESIAN_POINT('',(14.,58.8660496933282,-124.827115139388));
#51001=CARTESIAN_POINT('Origin',(14.,59.3410842491582,-125.423853191127));
#51002=CARTESIAN_POINT('',(14.,59.1970922754755,-125.765473267224));
#51003=CARTESIAN_POINT('',(14.,59.4850762228408,-125.08223311503));
#51004=CARTESIAN_POINT('Origin',(14.25,58.1851299230037,-125.961514582206));
#51005=CARTESIAN_POINT('',(14.5,58.2907844884389,-126.188091528965));
#51006=CARTESIAN_POINT('',(14.,58.0794753575685,-125.734937635446));
#51007=CARTESIAN_POINT('Origin',(14.,57.9365320709093,-126.078806628123));
#51008=CARTESIAN_POINT('',(14.,57.5822796533797,-125.969521727281));
#51009=CARTESIAN_POINT('',(14.,58.2907844884389,-126.188091528965));
#51010=CARTESIAN_POINT('Origin',(57.75,59.1020152039901,-124.744530166311));
#51011=CARTESIAN_POINT('',(58.,58.8660496933282,-124.827115139388));
#51012=CARTESIAN_POINT('',(57.5,59.3379807146521,-124.661945193235));
#51013=CARTESIAN_POINT('Origin',(57.75,58.1851299230037,-125.961514582206));
#51014=CARTESIAN_POINT('',(58.,58.0794753575685,-125.734937635446));
#51015=CARTESIAN_POINT('',(57.5,58.2907844884389,-126.188091528965));
#51016=CARTESIAN_POINT('Origin',(57.75,56.5433129818713,-123.730916769498));
#51017=CARTESIAN_POINT('',(57.5,56.3283735155941,-123.858592240269));
#51018=CARTESIAN_POINT('',(58.,56.7582524481486,-123.603241298728));
#51019=CARTESIAN_POINT('Origin',(14.,57.8987018584758,-124.164166824021));
#51020=CARTESIAN_POINT('Origin',(14.,55.7846344331431,-122.943216816385));
#51021=CARTESIAN_POINT('Origin',(14.,57.8376305949206,-126.399400659835));
#51022=CARTESIAN_POINT('Origin',(57.5,70.1603524804535,-119.421791454066));
#51023=CARTESIAN_POINT('',(57.5,69.9330127018922,-120.127531126037));
#51024=CARTESIAN_POINT('',(58.,69.7241542943354,-119.670765314673));
#51025=CARTESIAN_POINT('',(57.5,69.9330127018922,-120.127531126037));
#51026=CARTESIAN_POINT('',(57.5,70.1603524804535,-119.421791454066));
#51027=CARTESIAN_POINT('',(57.5,70.1603524804535,-119.421791454066));
#51028=CARTESIAN_POINT('',(58.,69.7241542943354,-119.670765314673));
#51029=CARTESIAN_POINT('Origin',(14.,70.0466825911729,-119.774661290051));
#51030=CARTESIAN_POINT('',(14.2512407024475,70.0466825911729,-119.774661290051));
#51031=CARTESIAN_POINT('',(14.5,70.1603524804535,-119.421791454066));
#51032=CARTESIAN_POINT('',(14.3353834448874,70.0851313901163,-119.655303195635));
#51033=CARTESIAN_POINT('',(14.,70.1603524804535,-119.421791454066));
#51034=CARTESIAN_POINT('',(14.5,69.9330127018922,-120.127531126037));
#51035=CARTESIAN_POINT('',(14.,69.9330127018922,-120.127531126037));
#51036=CARTESIAN_POINT('',(14.4305329766294,69.9647554706364,-120.028990820672));
#51037=CARTESIAN_POINT('Origin',(57.75,69.7493163731052,-119.118759534638));
#51038=CARTESIAN_POINT('',(58.,69.5214465371195,-119.221595996303));
#51039=CARTESIAN_POINT('',(57.5,69.9771862090909,-119.015923072972));
#51040=CARTESIAN_POINT('Origin',(57.5,69.0669872981077,-120.627531126037));
#51041=CARTESIAN_POINT('',(57.5,68.3421289244414,-120.471543313576));
#51042=CARTESIAN_POINT('',(58.,68.7758457056645,-120.218271533617));
#51043=CARTESIAN_POINT('',(57.5,68.3421289244414,-120.471543313576));
#51044=CARTESIAN_POINT('',(57.5,69.0669872981077,-120.627531126037));
#51045=CARTESIAN_POINT('',(57.5,69.0669872981077,-120.627531126037));
#51046=CARTESIAN_POINT('',(58.,68.7758457056645,-120.218271533617));
#51047=CARTESIAN_POINT('Origin',(14.,68.7045581112746,-120.549537219807));
#51048=CARTESIAN_POINT('',(14.2512407024475,68.7045581112746,-120.549537219807));
#51049=CARTESIAN_POINT('',(14.5,69.0669872981077,-120.627531126037));
#51050=CARTESIAN_POINT('',(14.2590041943422,68.7158691098264,-120.551971320018));
#51051=CARTESIAN_POINT('',(14.,69.0669872981077,-120.627531126037));
#51052=CARTESIAN_POINT('',(14.5,68.3421289244414,-120.471543313576));
#51053=CARTESIAN_POINT('',(14.,68.3421289244414,-120.471543313576));
#51054=CARTESIAN_POINT('',(14.6801520303733,68.0796569102617,-120.415059955155));
#51055=CARTESIAN_POINT('Origin',(57.75,68.9419872981077,-120.411024775091));
#51056=CARTESIAN_POINT('',(58.,68.8169872981077,-120.194518424145));
#51057=CARTESIAN_POINT('',(57.5,69.0669872981077,-120.627531126037));
#51058=CARTESIAN_POINT('Origin',(57.75,67.1120085569767,-118.332008835457));
#51059=CARTESIAN_POINT('',(57.5,66.9090146507462,-118.477931671344));
#51060=CARTESIAN_POINT('',(58.,67.3150024632071,-118.18608599957));
#51061=CARTESIAN_POINT('Origin',(14.25,69.7493163731052,-119.118759534638));
#51062=CARTESIAN_POINT('',(14.,69.7241542943354,-119.670765314673));
#51063=CARTESIAN_POINT('',(14.5,70.3660254037844,-119.877531126037));
#51064=CARTESIAN_POINT('',(14.,69.5214465371195,-119.221595996303));
#51065=CARTESIAN_POINT('',(14.5,69.9771862090909,-119.015923072972));
#51066=CARTESIAN_POINT('Origin',(14.,68.6339745962155,-120.877531126037));
#51067=CARTESIAN_POINT('',(14.5,69.0669872981077,-120.627531126037));
#51068=CARTESIAN_POINT('Origin',(14.25,68.9419872981077,-120.411024775091));
#51069=CARTESIAN_POINT('',(14.,68.7758457056645,-120.218271533617));
#51070=CARTESIAN_POINT('',(14.,68.7758457056645,-120.218271533617));
#51071=CARTESIAN_POINT('',(14.,68.8169872981077,-120.194518424145));
#51072=CARTESIAN_POINT('Origin',(14.25,67.1120085569767,-118.332008835457));
#51073=CARTESIAN_POINT('',(14.5,66.9090146507462,-118.477931671344));
#51074=CARTESIAN_POINT('',(14.,67.3150024632071,-118.18608599957));
#51075=CARTESIAN_POINT('Origin',(14.,66.2875644347017,-117.613429510899));
#51076=CARTESIAN_POINT('Origin',(14.,70.3660254037844,-119.877531126037));
#51077=CARTESIAN_POINT('Origin',(57.5,79.3175486306509,-114.148922374345));
#51078=CARTESIAN_POINT('',(57.5,78.5818533282824,-114.056703712549));
#51079=CARTESIAN_POINT('',(58.,78.9918455961109,-113.766594799967));
#51080=CARTESIAN_POINT('',(57.5,78.5818533282824,-114.056703712549));
#51081=CARTESIAN_POINT('',(57.5,79.3175486306509,-114.148922374345));
#51082=CARTESIAN_POINT('',(57.5,79.3175486306509,-114.148922374345));
#51083=CARTESIAN_POINT('',(58.,78.9918455961109,-113.766594799967));
#51084=CARTESIAN_POINT('Origin',(57.5,80.3016660917108,-112.852477851287));
#51085=CARTESIAN_POINT('',(57.5,80.1367006749398,-113.575345937994));
#51086=CARTESIAN_POINT('',(58.,79.8888272731287,-113.138521468083));
#51087=CARTESIAN_POINT('',(57.5,80.1367006749398,-113.575345937994));
#51088=CARTESIAN_POINT('',(57.5,80.3016660917108,-112.852477851287));
#51089=CARTESIAN_POINT('',(57.5,80.3016660917108,-112.852477851287));
#51090=CARTESIAN_POINT('',(58.,79.8888272731287,-113.138521468083));
#51091=CARTESIAN_POINT('Origin',(14.,78.9918455961109,-113.766594799967));
#51092=CARTESIAN_POINT('',(14.5,78.5818533282824,-114.056703712549));
#51093=CARTESIAN_POINT('',(14.5,79.3175486306509,-114.148922374345));
#51094=CARTESIAN_POINT('',(14.5,78.5818533282824,-114.056703712549));
#51095=CARTESIAN_POINT('',(14.,78.9918455961109,-113.766594799967));
#51096=CARTESIAN_POINT('',(14.,78.9918455961109,-113.766594799967));
#51097=CARTESIAN_POINT('',(14.5,79.3175486306509,-114.148922374345));
#51098=CARTESIAN_POINT('Origin',(14.25,77.1699412236247,-112.032522863357));
#51099=CARTESIAN_POINT('',(14.,77.3594446636108,-111.869463223246));
#51100=CARTESIAN_POINT('',(14.5,76.9804377836386,-112.195582503469));
#51101=CARTESIAN_POINT('Origin',(14.5,80.3016660917108,-112.852477851287));
#51102=CARTESIAN_POINT('',(14.,79.8888272731287,-113.138521468083));
#51103=CARTESIAN_POINT('',(14.5,80.1367006749398,-113.575345937994));
#51104=CARTESIAN_POINT('',(14.,79.8888272731287,-113.138521468083));
#51105=CARTESIAN_POINT('',(14.5,80.3016660917108,-112.852477851287));
#51106=CARTESIAN_POINT('',(14.5,80.3016660917108,-112.852477851287));
#51107=CARTESIAN_POINT('',(14.5,80.1367006749398,-113.575345937994));
#51108=CARTESIAN_POINT('Origin',(14.25,79.8657831288322,-112.586423217032));
#51109=CARTESIAN_POINT('',(14.5,80.0838230630982,-112.464117914346));
#51110=CARTESIAN_POINT('',(14.,79.6477431945662,-112.708728519719));
#51111=CARTESIAN_POINT('Origin',(14.,80.2191833833253,-113.213911894641));
#51112=CARTESIAN_POINT('',(14.,80.1367006749398,-113.575345937994));
#51113=CARTESIAN_POINT('',(14.,80.3016660917108,-112.852477851287));
#51114=CARTESIAN_POINT('Origin',(14.25,79.1741545215631,-113.944134363273));
#51115=CARTESIAN_POINT('',(14.5,79.3175486306509,-114.148922374345));
#51116=CARTESIAN_POINT('',(14.,79.0307604124753,-113.739346352201));
#51117=CARTESIAN_POINT('Origin',(14.,78.9497009794667,-114.102813043447));
#51118=CARTESIAN_POINT('',(14.,78.5818533282824,-114.056703712549));
#51119=CARTESIAN_POINT('',(14.,79.3175486306509,-114.148922374345));
#51120=CARTESIAN_POINT('Origin',(57.75,79.8657831288322,-112.586423217032));
#51121=CARTESIAN_POINT('',(58.,79.6477431945662,-112.708728519719));
#51122=CARTESIAN_POINT('',(57.5,80.0838230630982,-112.464117914346));
#51123=CARTESIAN_POINT('Origin',(57.75,79.1741545215631,-113.944134363273));
#51124=CARTESIAN_POINT('',(58.,79.0307604124753,-113.739346352201));
#51125=CARTESIAN_POINT('',(57.5,79.3175486306509,-114.148922374345));
#51126=CARTESIAN_POINT('Origin',(57.75,77.1699412236247,-112.032522863357));
#51127=CARTESIAN_POINT('',(57.5,76.9804377836386,-112.195582503469));
#51128=CARTESIAN_POINT('',(58.,77.3594446636108,-111.869463223246));
#51129=CARTESIAN_POINT('Origin',(14.,78.5799717800933,-112.223830067592));
#51130=CARTESIAN_POINT('Origin',(14.,76.2860060453866,-111.388532989905));
#51131=CARTESIAN_POINT('Origin',(14.,78.9079726085064,-114.435710592521));
#51132=CARTESIAN_POINT('Origin',(57.5,88.9644555248695,-106.801571398381));
#51133=CARTESIAN_POINT('',(57.5,88.223522379275,-106.773823726948));
#51134=CARTESIAN_POINT('',(58.,88.6066698449906,-106.449085585742));
#51135=CARTESIAN_POINT('',(57.5,88.223522379275,-106.773823726948));
#51136=CARTESIAN_POINT('',(57.5,88.9644555248695,-106.801571398381));
#51137=CARTESIAN_POINT('',(57.5,88.9644555248695,-106.801571398381));
#51138=CARTESIAN_POINT('',(58.,88.6066698449906,-106.449085585742));
#51139=CARTESIAN_POINT('Origin',(57.5,89.8318355365387,-105.424288749871));
#51140=CARTESIAN_POINT('',(57.5,89.7304999679885,-106.158783788695));
#51141=CARTESIAN_POINT('',(58.,89.4454980381808,-105.745225158215));
#51142=CARTESIAN_POINT('',(57.5,89.7304999679885,-106.158783788695));
#51143=CARTESIAN_POINT('',(57.5,89.8318355365387,-105.424288749871));
#51144=CARTESIAN_POINT('',(57.5,89.8318355365387,-105.424288749871));
#51145=CARTESIAN_POINT('',(58.,89.4454980381808,-105.745225158215));
#51146=CARTESIAN_POINT('Origin',(14.,88.6066698449906,-106.449085585742));
#51147=CARTESIAN_POINT('',(14.5,88.223522379275,-106.773823726948));
#51148=CARTESIAN_POINT('',(14.5,88.9644555248695,-106.801571398381));
#51149=CARTESIAN_POINT('',(14.5,88.223522379275,-106.773823726948));
#51150=CARTESIAN_POINT('',(14.,88.6066698449906,-106.449085585742));
#51151=CARTESIAN_POINT('',(14.,88.6066698449906,-106.449085585742));
#51152=CARTESIAN_POINT('',(14.5,88.9644555248695,-106.801571398381));
#51153=CARTESIAN_POINT('Origin',(14.25,86.6405640410765,-104.880401745181));
#51154=CARTESIAN_POINT('',(14.,86.8151347792147,-104.701446283163));
#51155=CARTESIAN_POINT('',(14.5,86.4659933029384,-105.059357207198));
#51156=CARTESIAN_POINT('Origin',(14.5,89.8318355365387,-105.424288749871));
#51157=CARTESIAN_POINT('',(14.,89.4454980381808,-105.745225158215));
#51158=CARTESIAN_POINT('',(14.5,89.7304999679885,-106.158783788695));
#51159=CARTESIAN_POINT('',(14.,89.4454980381808,-105.745225158215));
#51160=CARTESIAN_POINT('',(14.5,89.8318355365387,-105.424288749871));
#51161=CARTESIAN_POINT('',(14.5,89.8318355365387,-105.424288749871));
#51162=CARTESIAN_POINT('',(14.5,89.7304999679885,-106.158783788695));
#51163=CARTESIAN_POINT('Origin',(14.25,89.3744230506705,-105.197236237204));
#51164=CARTESIAN_POINT('',(14.5,89.5809736676609,-105.0563929107));
#51165=CARTESIAN_POINT('',(14.,89.1678724336801,-105.338079563709));
#51166=CARTESIAN_POINT('Origin',(14.,89.7811677522636,-105.791536269283));
#51167=CARTESIAN_POINT('',(14.,89.7304999679885,-106.158783788695));
#51168=CARTESIAN_POINT('',(14.,89.8318355365387,-105.424288749871));
#51169=CARTESIAN_POINT('Origin',(14.25,88.8037586224479,-106.610060287601));
#51170=CARTESIAN_POINT('',(14.5,88.9644555248695,-106.801571398381));
#51171=CARTESIAN_POINT('',(14.,88.6430617200262,-106.418549176822));
#51172=CARTESIAN_POINT('Origin',(14.,88.5939889520722,-106.787697562665));
#51173=CARTESIAN_POINT('',(14.,88.223522379275,-106.773823726948));
#51174=CARTESIAN_POINT('',(14.,88.9644555248695,-106.801571398381));
#51175=CARTESIAN_POINT('Origin',(57.75,89.3744230506705,-105.197236237204));
#51176=CARTESIAN_POINT('',(58.,89.1678724336801,-105.338079563709));
#51177=CARTESIAN_POINT('',(57.5,89.5809736676609,-105.0563929107));
#51178=CARTESIAN_POINT('Origin',(57.75,88.8037586224478,-106.610060287601));
#51179=CARTESIAN_POINT('',(58.,88.6430617200262,-106.418549176822));
#51180=CARTESIAN_POINT('',(57.5,88.9644555248695,-106.801571398381));
#51181=CARTESIAN_POINT('Origin',(57.75,86.6405640410765,-104.880401745181));
#51182=CARTESIAN_POINT('',(57.5,86.4659933029383,-105.059357207198));
#51183=CARTESIAN_POINT('',(58.,86.8151347792147,-104.701446283163));
#51184=CARTESIAN_POINT('Origin',(14.,88.0619025270559,-104.9480887073));
#51185=CARTESIAN_POINT('Origin',(14.,85.7038650873162,-104.315902474623));
#51186=CARTESIAN_POINT('Origin',(14.,88.58143330331,-107.122965203225));
#51187=CARTESIAN_POINT('Origin',(57.75,95.4517998511728,-96.9300774412053));
#51188=CARTESIAN_POINT('',(57.7487592975525,97.5640231742394,-98.6598632232557));
#51189=CARTESIAN_POINT('',(58.,97.5471438341798,-98.3214345544939));
#51190=CARTESIAN_POINT('',(58.2319907935076,97.5315577788306,-98.0089360833189));
#51191=CARTESIAN_POINT('',(58.,95.6101092987371,-96.7365881164045));
#51192=CARTESIAN_POINT('',(57.5,97.1937571541419,-98.6783304709881));
#51193=CARTESIAN_POINT('',(57.5,95.2934904036084,-97.1235667660061));
#51194=CARTESIAN_POINT('',(50.4896657310025,86.7592182449509,-99.1987595801943));
#51195=CARTESIAN_POINT('Origin',(58.,96.873629022557,-96.873629022557));
#51196=CARTESIAN_POINT('',(58.,98.3214345544939,-97.5471438341798));
#51197=CARTESIAN_POINT('',(58.,97.5807358037436,-98.2878425849301));
#51198=CARTESIAN_POINT('',(58.,98.0093803225402,-97.1657442173475));
#51199=CARTESIAN_POINT('Origin',(57.75,97.7575124990402,-98.4646192802268));
#51200=CARTESIAN_POINT('',(57.5,97.9342891943369,-98.6413959755234));
#51201=CARTESIAN_POINT('',(57.5,97.9342891943369,-98.6413959755234));
#51202=CARTESIAN_POINT('',(57.5,98.6413959755234,-97.9342891943369));
#51203=CARTESIAN_POINT('',(57.5,97.9342891943368,-98.6413959755234));
#51204=CARTESIAN_POINT('',(57.5,98.6413959755234,-97.9342891943369));
#51205=CARTESIAN_POINT('Origin',(14.,97.5640231742394,-98.6598632232557));
#51206=CARTESIAN_POINT('',(14.5,97.1937571541419,-98.6783304709881));
#51207=CARTESIAN_POINT('',(14.,97.1937571541419,-98.6783304709881));
#51208=CARTESIAN_POINT('',(14.5,97.9342891943368,-98.6413959755234));
#51209=CARTESIAN_POINT('',(14.5,97.1937571541419,-98.6783304709881));
#51210=CARTESIAN_POINT('',(14.,97.9342891943368,-98.6413959755234));
#51211=CARTESIAN_POINT('Origin',(57.5,98.678330470988,-97.1937571541419));
#51212=CARTESIAN_POINT('',(57.5,98.678330470988,-97.1937571541419));
#51213=CARTESIAN_POINT('',(57.5,98.678330470988,-97.1937571541419));
#51214=CARTESIAN_POINT('',(58.,98.3214345544939,-97.5471438341798));
#51215=CARTESIAN_POINT('Origin',(14.,97.5471438341798,-98.3214345544939));
#51216=CARTESIAN_POINT('',(14.,97.5471438341798,-98.3214345544939));
#51217=CARTESIAN_POINT('',(14.,97.5471438341798,-98.3214345544939));
#51218=CARTESIAN_POINT('',(14.5,97.9342891943369,-98.6413959755234));
#51219=CARTESIAN_POINT('Origin',(14.25,95.4517998511728,-96.9300774412053));
#51220=CARTESIAN_POINT('',(14.,95.6101092987371,-96.7365881164045));
#51221=CARTESIAN_POINT('',(14.5,95.2934904036084,-97.1235667660061));
#51222=CARTESIAN_POINT('Origin',(14.5,98.678330470988,-97.1937571541419));
#51223=CARTESIAN_POINT('',(14.,98.3214345544939,-97.5471438341798));
#51224=CARTESIAN_POINT('',(14.5,98.6413959755234,-97.9342891943369));
#51225=CARTESIAN_POINT('',(14.,98.3214345544939,-97.5471438341798));
#51226=CARTESIAN_POINT('',(14.5,98.678330470988,-97.1937571541419));
#51227=CARTESIAN_POINT('',(14.5,98.678330470988,-97.1937571541419));
#51228=CARTESIAN_POINT('',(14.5,98.6413959755234,-97.9342891943369));
#51229=CARTESIAN_POINT('Origin',(14.25,98.2028696473411,-97.0074347697832));
#51230=CARTESIAN_POINT('',(14.5,98.3963589721419,-96.8491253222189));
#51231=CARTESIAN_POINT('',(14.,98.0093803225402,-97.1657442173475));
#51232=CARTESIAN_POINT('Origin',(14.,98.6598632232557,-97.5640231742394));
#51233=CARTESIAN_POINT('',(14.,98.6413959755234,-97.9342891943369));
#51234=CARTESIAN_POINT('',(14.,98.678330470988,-97.1937571541419));
#51235=CARTESIAN_POINT('Origin',(14.25,97.7575124990402,-98.4646192802268));
#51236=CARTESIAN_POINT('',(14.5,97.9342891943368,-98.6413959755234));
#51237=CARTESIAN_POINT('',(14.,97.5807358037436,-98.2878425849301));
#51238=CARTESIAN_POINT('Origin',(57.75,98.2028696473411,-97.0074347697832));
#51239=CARTESIAN_POINT('',(57.5,98.3963589721419,-96.8491253222189));
#51240=CARTESIAN_POINT('Origin',(14.,94.4694659665227,-96.4493649538451));
#51241=CARTESIAN_POINT('Origin',(14.,97.5807358037436,-98.9949493661167));
#51242=CARTESIAN_POINT('Origin',(57.5,106.158783788695,-89.7304999679885));
#51243=CARTESIAN_POINT('',(57.5,105.424288749871,-89.8318355365387));
#51244=CARTESIAN_POINT('',(58.,105.745225158215,-89.4454980381808));
#51245=CARTESIAN_POINT('',(57.5,105.424288749871,-89.8318355365387));
#51246=CARTESIAN_POINT('',(57.5,106.158783788695,-89.7304999679885));
#51247=CARTESIAN_POINT('',(57.5,106.158783788695,-89.7304999679885));
#51248=CARTESIAN_POINT('',(58.,105.745225158215,-89.4454980381808));
#51249=CARTESIAN_POINT('Origin',(57.5,106.773823726948,-88.223522379275));
#51250=CARTESIAN_POINT('',(57.5,106.801571398381,-88.9644555248695));
#51251=CARTESIAN_POINT('',(58.,106.449085585742,-88.6066698449906));
#51252=CARTESIAN_POINT('',(57.5,106.801571398381,-88.9644555248695));
#51253=CARTESIAN_POINT('',(57.5,106.773823726948,-88.223522379275));
#51254=CARTESIAN_POINT('',(57.5,106.773823726948,-88.223522379275));
#51255=CARTESIAN_POINT('',(58.,106.449085585742,-88.6066698449906));
#51256=CARTESIAN_POINT('Origin',(14.,105.745225158215,-89.4454980381808));
#51257=CARTESIAN_POINT('',(14.5,105.424288749871,-89.8318355365387));
#51258=CARTESIAN_POINT('',(14.5,106.158783788695,-89.7304999679885));
#51259=CARTESIAN_POINT('',(14.5,105.424288749871,-89.8318355365387));
#51260=CARTESIAN_POINT('',(14.,105.745225158215,-89.4454980381808));
#51261=CARTESIAN_POINT('',(14.,105.745225158215,-89.4454980381808));
#51262=CARTESIAN_POINT('',(14.5,106.158783788695,-89.7304999679885));
#51263=CARTESIAN_POINT('Origin',(14.25,103.536589829029,-88.2420567199213));
#51264=CARTESIAN_POINT('',(14.,103.677433155534,-88.0355061029309));
#51265=CARTESIAN_POINT('',(14.5,103.395746502524,-88.4486073369116));
#51266=CARTESIAN_POINT('Origin',(14.5,106.773823726948,-88.223522379275));
#51267=CARTESIAN_POINT('',(14.,106.449085585742,-88.6066698449906));
#51268=CARTESIAN_POINT('',(14.5,106.801571398381,-88.9644555248695));
#51269=CARTESIAN_POINT('',(14.,106.449085585742,-88.6066698449906));
#51270=CARTESIAN_POINT('',(14.5,106.773823726948,-88.223522379275));
#51271=CARTESIAN_POINT('',(14.5,106.773823726948,-88.223522379275));
#51272=CARTESIAN_POINT('',(14.5,106.801571398381,-88.9644555248695));
#51273=CARTESIAN_POINT('Origin',(14.25,106.283933109481,-88.0793481490734));
#51274=CARTESIAN_POINT('',(14.5,106.462888571499,-87.9047774109353));
#51275=CARTESIAN_POINT('',(14.,106.104977647464,-88.2539188872116));
#51276=CARTESIAN_POINT('Origin',(14.,106.787697562665,-88.5939889520723));
#51277=CARTESIAN_POINT('',(14.,106.801571398381,-88.9644555248695));
#51278=CARTESIAN_POINT('',(14.,106.773823726948,-88.223522379275));
#51279=CARTESIAN_POINT('Origin',(14.25,105.967272677915,-89.5698030655668));
#51280=CARTESIAN_POINT('',(14.5,106.158783788695,-89.7304999679885));
#51281=CARTESIAN_POINT('',(14.,105.775761567135,-89.4091061631452));
#51282=CARTESIAN_POINT('Origin',(14.,105.791536269283,-89.7811677522636));
#51283=CARTESIAN_POINT('',(14.,105.424288749871,-89.8318355365387));
#51284=CARTESIAN_POINT('',(14.,106.158783788695,-89.7304999679885));
#51285=CARTESIAN_POINT('Origin',(57.75,106.283933109481,-88.0793481490734));
#51286=CARTESIAN_POINT('',(58.,106.104977647464,-88.2539188872116));
#51287=CARTESIAN_POINT('',(57.5,106.462888571499,-87.9047774109353));
#51288=CARTESIAN_POINT('Origin',(57.75,105.967272677915,-89.5698030655668));
#51289=CARTESIAN_POINT('',(58.,105.775761567135,-89.4091061631452));
#51290=CARTESIAN_POINT('',(57.5,106.158783788695,-89.7304999679885));
#51291=CARTESIAN_POINT('Origin',(57.75,103.536589829029,-88.2420567199213));
#51292=CARTESIAN_POINT('',(57.5,103.395746502524,-88.4486073369116));
#51293=CARTESIAN_POINT('',(58.,103.677433155534,-88.0355061029309));
#51294=CARTESIAN_POINT('Origin',(14.,104.9480887073,-88.0619025270559));
#51295=CARTESIAN_POINT('Origin',(14.,102.516097167501,-87.8487895280494));
#51296=CARTESIAN_POINT('Origin',(14.,105.837389983851,-90.113522189548));
#51297=CARTESIAN_POINT('Origin',(57.5,114.056703712549,-78.5818533282825));
#51298=CARTESIAN_POINT('',(57.5,114.148922374345,-79.317548630651));
#51299=CARTESIAN_POINT('',(58.,113.766594799967,-78.9918455961111));
#51300=CARTESIAN_POINT('',(57.5,114.148922374345,-79.317548630651));
#51301=CARTESIAN_POINT('',(57.5,114.056703712549,-78.5818533282825));
#51302=CARTESIAN_POINT('',(57.5,114.056703712549,-78.5818533282825));
#51303=CARTESIAN_POINT('',(58.,113.766594799967,-78.9918455961111));
#51304=CARTESIAN_POINT('Origin',(14.,114.102813043447,-78.9497009794668));
#51305=CARTESIAN_POINT('',(14.2512407024475,114.102813043447,-78.9497009794668));
#51306=CARTESIAN_POINT('',(14.5,114.056703712549,-78.5818533282825));
#51307=CARTESIAN_POINT('',(14.3353834448875,114.087216578945,-78.825276644476));
#51308=CARTESIAN_POINT('',(14.,114.056703712549,-78.5818533282825));
#51309=CARTESIAN_POINT('',(14.5,114.148922374345,-79.317548630651));
#51310=CARTESIAN_POINT('',(14.,114.148922374345,-79.317548630651));
#51311=CARTESIAN_POINT('',(14.4305329766294,114.136046160276,-79.2148257108122));
#51312=CARTESIAN_POINT('Origin',(57.75,113.556111664665,-78.4809245051847));
#51313=CARTESIAN_POINT('',(58.,113.393052024553,-78.6704279451708));
#51314=CARTESIAN_POINT('',(57.5,113.719171304777,-78.2914210651986));
#51315=CARTESIAN_POINT('Origin',(57.5,113.575345937994,-80.13670067494));
#51316=CARTESIAN_POINT('',(57.5,112.852477851287,-80.301666091711));
#51317=CARTESIAN_POINT('',(58.,113.138521468083,-79.8888272731288));
#51318=CARTESIAN_POINT('',(57.5,112.852477851287,-80.301666091711));
#51319=CARTESIAN_POINT('',(57.5,113.575345937994,-80.13670067494));
#51320=CARTESIAN_POINT('',(57.5,113.575345937994,-80.13670067494));
#51321=CARTESIAN_POINT('',(58.,113.138521468083,-79.8888272731288));
#51322=CARTESIAN_POINT('Origin',(14.,113.213911894641,-80.2191833833255));
#51323=CARTESIAN_POINT('',(14.2512407024475,113.213911894641,-80.2191833833255));
#51324=CARTESIAN_POINT('',(14.5,113.575345937994,-80.13670067494));
#51325=CARTESIAN_POINT('',(14.2590041943422,113.225191835908,-80.2166091927553));
#51326=CARTESIAN_POINT('',(14.,113.575345937994,-80.13670067494));
#51327=CARTESIAN_POINT('',(14.5,112.852477851287,-80.301666091711));
#51328=CARTESIAN_POINT('',(14.,112.852477851287,-80.301666091711));
#51329=CARTESIAN_POINT('',(14.6801520303733,112.590726522204,-80.3614002505245));
#51330=CARTESIAN_POINT('Origin',(57.75,113.370557926922,-79.9933065658522));
#51331=CARTESIAN_POINT('',(58.,113.16576991585,-79.8499124567644));
#51332=CARTESIAN_POINT('',(57.5,113.575345937994,-80.13670067494));
#51333=CARTESIAN_POINT('Origin',(57.75,110.833403841184,-78.882460664988));
#51334=CARTESIAN_POINT('',(57.5,110.711098538497,-79.100500599254));
#51335=CARTESIAN_POINT('',(58.,110.955709143871,-78.6644207307221));
#51336=CARTESIAN_POINT('Origin',(14.25,113.556111664665,-78.4809245051847));
#51337=CARTESIAN_POINT('',(14.,113.766594799967,-78.991845596111));
#51338=CARTESIAN_POINT('',(14.5,114.435710592521,-78.9079726085065));
#51339=CARTESIAN_POINT('',(14.,113.393052024553,-78.6704279451708));
#51340=CARTESIAN_POINT('',(14.5,113.719171304777,-78.2914210651986));
#51341=CARTESIAN_POINT('Origin',(14.,113.288557719819,-80.5462766970845));
#51342=CARTESIAN_POINT('',(14.5,113.575345937994,-80.13670067494));
#51343=CARTESIAN_POINT('Origin',(14.25,113.370557926922,-79.9933065658522));
#51344=CARTESIAN_POINT('',(14.,113.138521468083,-79.8888272731288));
#51345=CARTESIAN_POINT('',(14.,113.138521468083,-79.8888272731288));
#51346=CARTESIAN_POINT('',(14.,113.16576991585,-79.8499124567644));
#51347=CARTESIAN_POINT('Origin',(14.25,110.833403841184,-78.882460664988));
#51348=CARTESIAN_POINT('',(14.5,110.711098538497,-79.100500599254));
#51349=CARTESIAN_POINT('',(14.,110.955709143871,-78.6644207307221));
#51350=CARTESIAN_POINT('Origin',(14.,109.782518968122,-78.5796317693959));
#51351=CARTESIAN_POINT('Origin',(14.,114.435710592521,-78.9079726085065));
#51352=CARTESIAN_POINT('Origin',(57.5,120.127531126037,-69.9330127018923));
#51353=CARTESIAN_POINT('',(57.5,119.421791454066,-70.1603524804536));
#51354=CARTESIAN_POINT('',(58.,119.670765314673,-69.7241542943355));
#51355=CARTESIAN_POINT('',(57.5,119.421791454066,-70.1603524804536));
#51356=CARTESIAN_POINT('',(57.5,120.127531126037,-69.9330127018923));
#51357=CARTESIAN_POINT('',(57.5,120.127531126037,-69.9330127018923));
#51358=CARTESIAN_POINT('',(58.,119.670765314673,-69.7241542943355));
#51359=CARTESIAN_POINT('Origin',(57.5,120.471543313576,-68.3421289244415));
#51360=CARTESIAN_POINT('',(57.5,120.627531126037,-69.0669872981079));
#51361=CARTESIAN_POINT('',(58.,120.218271533617,-68.7758457056646));
#51362=CARTESIAN_POINT('',(57.5,120.627531126037,-69.0669872981079));
#51363=CARTESIAN_POINT('',(57.5,120.471543313576,-68.3421289244415));
#51364=CARTESIAN_POINT('',(57.5,120.471543313576,-68.3421289244415));
#51365=CARTESIAN_POINT('',(58.,120.218271533617,-68.7758457056646));
#51366=CARTESIAN_POINT('Origin',(14.,119.670765314673,-69.7241542943355));
#51367=CARTESIAN_POINT('',(14.5,119.421791454066,-70.1603524804536));
#51368=CARTESIAN_POINT('',(14.5,120.127531126037,-69.9330127018923));
#51369=CARTESIAN_POINT('',(14.5,119.421791454066,-70.1603524804536));
#51370=CARTESIAN_POINT('',(14.,119.670765314673,-69.7241542943355));
#51371=CARTESIAN_POINT('',(14.,119.670765314673,-69.7241542943355));
#51372=CARTESIAN_POINT('',(14.5,120.127531126037,-69.9330127018923));
#51373=CARTESIAN_POINT('Origin',(14.25,117.286708727069,-68.9225214538622));
#51374=CARTESIAN_POINT('',(14.,117.389545188734,-68.6946516178765));
#51375=CARTESIAN_POINT('',(14.5,117.183872265403,-69.1503912898478));
#51376=CARTESIAN_POINT('Origin',(14.5,120.471543313576,-68.3421289244415));
#51377=CARTESIAN_POINT('',(14.,120.218271533617,-68.7758457056646));
#51378=CARTESIAN_POINT('',(14.5,120.627531126037,-69.0669872981079));
#51379=CARTESIAN_POINT('',(14.,120.218271533617,-68.7758457056646));
#51380=CARTESIAN_POINT('',(14.5,120.471543313576,-68.3421289244415));
#51381=CARTESIAN_POINT('',(14.5,120.471543313576,-68.3421289244415));
#51382=CARTESIAN_POINT('',(14.5,120.627531126037,-69.0669872981079));
#51383=CARTESIAN_POINT('Origin',(14.25,119.964059643026,-68.2852136377336));
#51384=CARTESIAN_POINT('',(14.5,120.109982478913,-68.0822197315032));
#51385=CARTESIAN_POINT('',(14.,119.818136807139,-68.488207543964));
#51386=CARTESIAN_POINT('Origin',(14.,120.549537219807,-68.7045581112747));
#51387=CARTESIAN_POINT('',(14.,120.627531126037,-69.0669872981079));
#51388=CARTESIAN_POINT('',(14.,120.471543313576,-68.3421289244415));
#51389=CARTESIAN_POINT('Origin',(14.25,119.911024775091,-69.8080127018923));
#51390=CARTESIAN_POINT('',(14.5,120.127531126037,-69.9330127018923));
#51391=CARTESIAN_POINT('',(14.,119.694518424145,-69.6830127018923));
#51392=CARTESIAN_POINT('Origin',(14.,119.774661290051,-70.0466825911729));
#51393=CARTESIAN_POINT('',(14.,119.421791454066,-70.1603524804536));
#51394=CARTESIAN_POINT('',(14.,120.127531126037,-69.9330127018923));
#51395=CARTESIAN_POINT('Origin',(57.75,119.964059643026,-68.2852136377336));
#51396=CARTESIAN_POINT('',(58.,119.818136807139,-68.4882075439641));
#51397=CARTESIAN_POINT('',(57.5,120.109982478913,-68.0822197315032));
#51398=CARTESIAN_POINT('Origin',(57.75,119.911024775091,-69.8080127018923));
#51399=CARTESIAN_POINT('',(58.,119.694518424145,-69.6830127018923));
#51400=CARTESIAN_POINT('',(57.5,120.127531126037,-69.9330127018923));
#51401=CARTESIAN_POINT('Origin',(57.75,117.286708727069,-68.9225214538622));
#51402=CARTESIAN_POINT('',(57.5,117.183872265403,-69.1503912898478));
#51403=CARTESIAN_POINT('',(58.,117.389545188734,-68.6946516178765));
#51404=CARTESIAN_POINT('Origin',(14.,118.645480318468,-68.5000000000001));
#51405=CARTESIAN_POINT('Origin',(14.,116.213429510899,-68.7124355652983));
#51406=CARTESIAN_POINT('Origin',(14.,119.877531126037,-70.3660254037845));
#51407=CARTESIAN_POINT('Origin',(57.5,125.765473267224,-59.1970922754756));
#51408=CARTESIAN_POINT('',(57.5,125.08223311503,-59.4850762228409));
#51409=CARTESIAN_POINT('',(58.,125.292242378034,-59.0288384007668));
#51410=CARTESIAN_POINT('',(57.5,125.08223311503,-59.4850762228409));
#51411=CARTESIAN_POINT('',(57.5,125.765473267224,-59.1970922754756));
#51412=CARTESIAN_POINT('',(57.5,125.765473267224,-59.1970922754756));
#51413=CARTESIAN_POINT('',(58.,125.292242378034,-59.0288384007668));
#51414=CARTESIAN_POINT('Origin',(57.5,125.969521727281,-57.5822796533798));
#51415=CARTESIAN_POINT('',(57.5,126.188091528965,-58.290784488439));
#51416=CARTESIAN_POINT('',(58.,125.755014631118,-58.036420101407));
#51417=CARTESIAN_POINT('',(57.5,126.188091528965,-58.290784488439));
#51418=CARTESIAN_POINT('',(57.5,125.969521727281,-57.5822796533798));
#51419=CARTESIAN_POINT('',(57.5,125.969521727281,-57.5822796533798));
#51420=CARTESIAN_POINT('',(58.,125.755014631118,-58.036420101407));
#51421=CARTESIAN_POINT('Origin',(14.,125.292242378034,-59.0288384007668));
#51422=CARTESIAN_POINT('',(14.5,125.08223311503,-59.4850762228409));
#51423=CARTESIAN_POINT('',(14.5,125.765473267224,-59.1970922754756));
#51424=CARTESIAN_POINT('',(14.5,125.08223311503,-59.4850762228409));
#51425=CARTESIAN_POINT('',(14.,125.292242378034,-59.0288384007668));
#51426=CARTESIAN_POINT('',(14.,125.292242378034,-59.0288384007668));
#51427=CARTESIAN_POINT('',(14.5,125.765473267224,-59.1970922754756));
#51428=CARTESIAN_POINT('Origin',(14.25,122.84739093989,-58.4380402379162));
#51429=CARTESIAN_POINT('',(14.,122.929975912966,-58.2020747272542));
#51430=CARTESIAN_POINT('',(14.5,122.764805966813,-58.6740057485781));
#51431=CARTESIAN_POINT('Origin',(14.5,125.969521727281,-57.5822796533798));
#51432=CARTESIAN_POINT('',(14.,125.755014631118,-58.036420101407));
#51433=CARTESIAN_POINT('',(14.5,126.188091528965,-58.290784488439));
#51434=CARTESIAN_POINT('',(14.,125.755014631118,-58.036420101407));
#51435=CARTESIAN_POINT('',(14.5,125.969521727281,-57.5822796533798));
#51436=CARTESIAN_POINT('',(14.5,125.969521727281,-57.5822796533798));
#51437=CARTESIAN_POINT('',(14.5,126.188091528965,-58.290784488439));
#51438=CARTESIAN_POINT('Origin',(14.25,125.459008691224,-57.5698110627601));
#51439=CARTESIAN_POINT('',(14.5,125.586684161994,-57.3548715964829));
#51440=CARTESIAN_POINT('',(14.,125.331333220453,-57.7847505290374));
#51441=CARTESIAN_POINT('Origin',(14.,126.078806628123,-57.9365320709094));
#51442=CARTESIAN_POINT('',(14.,126.188091528965,-58.290784488439));
#51443=CARTESIAN_POINT('',(14.,125.969521727281,-57.5822796533798));
#51444=CARTESIAN_POINT('Origin',(14.25,125.538896320465,-59.0914377100405));
#51445=CARTESIAN_POINT('',(14.5,125.765473267224,-59.1970922754756));
#51446=CARTESIAN_POINT('',(14.,125.312319373706,-58.9857831446053));
#51447=CARTESIAN_POINT('Origin',(14.,125.423853191127,-59.3410842491583));
#51448=CARTESIAN_POINT('',(14.,125.08223311503,-59.4850762228409));
#51449=CARTESIAN_POINT('',(14.,125.765473267224,-59.1970922754756));
#51450=CARTESIAN_POINT('Origin',(57.75,125.459008691224,-57.5698110627601));
#51451=CARTESIAN_POINT('',(58.,125.331333220453,-57.7847505290374));
#51452=CARTESIAN_POINT('',(57.5,125.586684161994,-57.3548715964829));
#51453=CARTESIAN_POINT('Origin',(57.75,125.538896320465,-59.0914377100405));
#51454=CARTESIAN_POINT('',(58.,125.312319373706,-58.9857831446053));
#51455=CARTESIAN_POINT('',(57.5,125.765473267224,-59.1970922754756));
#51456=CARTESIAN_POINT('Origin',(57.75,122.84739093989,-58.4380402379162));
#51457=CARTESIAN_POINT('',(57.5,122.764805966813,-58.6740057485781));
#51458=CARTESIAN_POINT('',(58.,122.929975912966,-58.2020747272542));
#51459=CARTESIAN_POINT('Origin',(14.,124.164166824021,-57.8987018584759));
#51460=CARTESIAN_POINT('Origin',(14.,121.759885683511,-58.3222962368458));
#51461=CARTESIAN_POINT('Origin',(14.,125.554164136354,-59.6502461689939));
#51462=CARTESIAN_POINT('Origin',(57.75,127.473130330375,-47.5088102499062));
#51463=CARTESIAN_POINT('',(57.7487592975525,130.118493836425,-48.1838644248812));
#51464=CARTESIAN_POINT('',(58.,129.960169823373,-47.8842774043812));
#51465=CARTESIAN_POINT('',(58.2319907935076,129.813976499357,-47.6076445581374));
#51466=CARTESIAN_POINT('',(58.,127.534835293351,-47.266544904584));
#51467=CARTESIAN_POINT('',(57.5,129.790723455271,-48.3570826171013));
#51468=CARTESIAN_POINT('',(57.5,127.411425367399,-47.7510755952284));
#51469=CARTESIAN_POINT('',(50.4896657310027,120.553762433226,-53.2385782672432));
#51470=CARTESIAN_POINT('Origin',(58.,128.737889047669,-46.8567596356167));
#51471=CARTESIAN_POINT('',(58.,130.334686134323,-46.8553022968292));
#51472=CARTESIAN_POINT('',(58.,129.976417907185,-47.8396361609982));
#51473=CARTESIAN_POINT('',(58.,129.890682510832,-46.6415166711984));
#51474=CARTESIAN_POINT('Origin',(57.75,130.211341062382,-47.9251411968296));
#51475=CARTESIAN_POINT('',(57.5,130.446264217578,-48.010646232661));
#51476=CARTESIAN_POINT('',(57.5,130.446264217578,-48.010646232661));
#51477=CARTESIAN_POINT('',(57.5,130.788284360904,-47.0709536118751));
#51478=CARTESIAN_POINT('',(57.5,130.446264217578,-48.010646232661));
#51479=CARTESIAN_POINT('',(57.5,130.788284360904,-47.0709536118751));
#51480=CARTESIAN_POINT('Origin',(14.,130.118493836425,-48.1838644248812));
#51481=CARTESIAN_POINT('',(14.5,129.790723455271,-48.3570826171013));
#51482=CARTESIAN_POINT('',(14.,129.790723455271,-48.3570826171013));
#51483=CARTESIAN_POINT('',(14.5,130.446264217578,-48.010646232661));
#51484=CARTESIAN_POINT('',(14.5,129.790723455271,-48.3570826171013));
#51485=CARTESIAN_POINT('',(14.,130.446264217578,-48.010646232661));
#51486=CARTESIAN_POINT('Origin',(57.5,130.508796018163,-46.3841944650247));
#51487=CARTESIAN_POINT('',(57.5,130.508796018163,-46.3841944650247));
#51488=CARTESIAN_POINT('',(57.5,130.508796018163,-46.3841944650247));
#51489=CARTESIAN_POINT('',(58.,130.334686134323,-46.8553022968292));
#51490=CARTESIAN_POINT('Origin',(14.,129.960169823373,-47.8842774043812));
#51491=CARTESIAN_POINT('',(14.,129.960169823373,-47.8842774043812));
#51492=CARTESIAN_POINT('',(14.,129.960169823373,-47.8842774043812));
#51493=CARTESIAN_POINT('',(14.5,130.446264217578,-48.010646232661));
#51494=CARTESIAN_POINT('Origin',(14.25,127.473130330375,-47.5088102499062));
#51495=CARTESIAN_POINT('',(14.,127.534835293351,-47.266544904584));
#51496=CARTESIAN_POINT('',(14.5,127.411425367399,-47.7510755952284));
#51497=CARTESIAN_POINT('Origin',(14.5,130.508796018163,-46.3841944650247));
#51498=CARTESIAN_POINT('',(14.,130.334686134323,-46.8553022968292));
#51499=CARTESIAN_POINT('',(14.5,130.788284360904,-47.0709536118751));
#51500=CARTESIAN_POINT('',(14.,130.334686134323,-46.8553022968292));
#51501=CARTESIAN_POINT('',(14.5,130.508796018163,-46.3841944650247));
#51502=CARTESIAN_POINT('',(14.5,130.508796018163,-46.3841944650247));
#51503=CARTESIAN_POINT('',(14.5,130.788284360904,-47.0709536118751));
#51504=CARTESIAN_POINT('Origin',(14.25,129.99913892906,-46.4162674639967));
#51505=CARTESIAN_POINT('',(14.5,130.107595347289,-46.191018256795));
#51506=CARTESIAN_POINT('',(14.,129.890682510832,-46.6415166711984));
#51507=CARTESIAN_POINT('Origin',(14.,130.648540189534,-46.7275740384499));
#51508=CARTESIAN_POINT('',(14.,130.788284360904,-47.0709536118751));
#51509=CARTESIAN_POINT('',(14.,130.508796018163,-46.3841944650247));
#51510=CARTESIAN_POINT('Origin',(14.25,130.211341062382,-47.9251411968296));
#51511=CARTESIAN_POINT('',(14.5,130.446264217578,-48.010646232661));
#51512=CARTESIAN_POINT('',(14.,129.976417907185,-47.8396361609982));
#51513=CARTESIAN_POINT('Origin',(57.75,129.99913892906,-46.4162674639967));
#51514=CARTESIAN_POINT('',(57.5,130.107595347289,-46.191018256795));
#51515=CARTESIAN_POINT('Origin',(14.,126.379675605442,-47.4882890180656));
#51516=CARTESIAN_POINT('Origin',(14.,130.275254145916,-48.480492543054));
#51517=CARTESIAN_POINT('Origin',(57.5,134.134280331629,-36.4588101823949));
#51518=CARTESIAN_POINT('',(57.5,133.511428020236,-36.8610624138407));
#51519=CARTESIAN_POINT('',(58.,133.639021904261,-36.375288143631));
#51520=CARTESIAN_POINT('',(57.5,133.511428020236,-36.8610624138407));
#51521=CARTESIAN_POINT('',(57.5,134.134280331629,-36.4588101823949));
#51522=CARTESIAN_POINT('',(57.5,134.134280331629,-36.4588101823949));
#51523=CARTESIAN_POINT('',(58.,133.639021904261,-36.375288143631));
#51524=CARTESIAN_POINT('Origin',(57.5,134.054819567983,-34.8330975492484));
#51525=CARTESIAN_POINT('',(57.5,134.393099376732,-35.4928843561058));
#51526=CARTESIAN_POINT('',(58.,133.922431977811,-35.3175873497673));
#51527=CARTESIAN_POINT('',(57.5,134.393099376732,-35.4928843561058));
#51528=CARTESIAN_POINT('',(57.5,134.054819567983,-34.8330975492484));
#51529=CARTESIAN_POINT('',(57.5,134.054819567983,-34.8330975492484));
#51530=CARTESIAN_POINT('',(58.,133.922431977811,-35.3175873497673));
#51531=CARTESIAN_POINT('Origin',(14.,133.639021904261,-36.375288143631));
#51532=CARTESIAN_POINT('',(14.5,133.511428020236,-36.8610624138407));
#51533=CARTESIAN_POINT('',(14.5,134.134280331629,-36.4588101823949));
#51534=CARTESIAN_POINT('',(14.5,133.511428020236,-36.8610624138407));
#51535=CARTESIAN_POINT('',(14.,133.639021904261,-36.3752881436309));
#51536=CARTESIAN_POINT('',(14.,133.639021904261,-36.375288143631));
#51537=CARTESIAN_POINT('',(14.5,134.134280331629,-36.4588101823949));
#51538=CARTESIAN_POINT('Origin',(14.25,131.128722228666,-36.2180095292903));
#51539=CARTESIAN_POINT('',(14.,131.169077569515,-35.9712881348695));
#51540=CARTESIAN_POINT('',(14.5,131.088366887817,-36.4647309237111));
#51541=CARTESIAN_POINT('Origin',(14.5,134.054819567983,-34.8330975492484));
#51542=CARTESIAN_POINT('',(14.,133.922431977811,-35.3175873497673));
#51543=CARTESIAN_POINT('',(14.5,134.393099376732,-35.4928843561058));
#51544=CARTESIAN_POINT('',(14.,133.922431977811,-35.3175873497673));
#51545=CARTESIAN_POINT('',(14.5,134.054819567983,-34.8330975492484));
#51546=CARTESIAN_POINT('',(14.5,134.054819567983,-34.8330975492484));
#51547=CARTESIAN_POINT('',(14.5,134.393099376732,-35.4928843561058));
#51548=CARTESIAN_POINT('Origin',(14.25,133.549897224021,-34.9094680429235));
#51549=CARTESIAN_POINT('',(14.5,133.638309170877,-34.6756233772733));
#51550=CARTESIAN_POINT('',(14.,133.461485277164,-35.1433127085737));
#51551=CARTESIAN_POINT('Origin',(14.,134.223959472357,-35.1629909526771));
#51552=CARTESIAN_POINT('',(14.,134.393099376732,-35.4928843561058));
#51553=CARTESIAN_POINT('',(14.,134.054819567983,-34.8330975492484));
#51554=CARTESIAN_POINT('Origin',(14.25,133.892798875057,-36.3941054211193));
#51555=CARTESIAN_POINT('',(14.5,134.134280331629,-36.4588101823949));
#51556=CARTESIAN_POINT('',(14.,133.651317418485,-36.3294006598436));
#51557=CARTESIAN_POINT('Origin',(14.,133.822854175933,-36.6599362981178));
#51558=CARTESIAN_POINT('',(14.,133.511428020236,-36.8610624138407));
#51559=CARTESIAN_POINT('',(14.,134.134280331629,-36.4588101823949));
#51560=CARTESIAN_POINT('Origin',(57.75,133.549897224021,-34.9094680429235));
#51561=CARTESIAN_POINT('',(58.,133.461485277164,-35.1433127085737));
#51562=CARTESIAN_POINT('',(57.5,133.638309170877,-34.6756233772733));
#51563=CARTESIAN_POINT('Origin',(57.75,133.892798875057,-36.3941054211193));
#51564=CARTESIAN_POINT('',(58.,133.651317418485,-36.3294006598436));
#51565=CARTESIAN_POINT('',(57.5,134.134280331629,-36.4588101823949));
#51566=CARTESIAN_POINT('Origin',(57.75,131.128722228666,-36.2180095292903));
#51567=CARTESIAN_POINT('',(57.5,131.088366887817,-36.4647309237111));
#51568=CARTESIAN_POINT('',(58.,131.169077569515,-35.9712881348695));
#51569=CARTESIAN_POINT('Origin',(14.,132.331838201602,-35.4582091790453));
#51570=CARTESIAN_POINT('Origin',(14.,130.037639885881,-36.292867245645));
#51571=CARTESIAN_POINT('Origin',(14.,134.004870809078,-36.9417730955394));
#51572=CARTESIAN_POINT('Origin',(57.5,136.580604996376,-23.016899728323));
#51573=CARTESIAN_POINT('',(57.5,136.97510175753,-23.6446928191972));
#51574=CARTESIAN_POINT('',(58.,136.490947249372,-23.5110842376315));
#51575=CARTESIAN_POINT('',(57.5,136.97510175753,-23.6446928191972));
#51576=CARTESIAN_POINT('',(57.5,136.580604996376,-23.016899728323));
#51577=CARTESIAN_POINT('',(57.5,136.580604996376,-23.016899728323));
#51578=CARTESIAN_POINT('',(58.,136.490947249372,-23.5110842376315));
#51579=CARTESIAN_POINT('Origin',(14.,136.777853376953,-23.3307962737601));
#51580=CARTESIAN_POINT('',(14.2512407024475,136.777853376953,-23.3307962737601));
#51581=CARTESIAN_POINT('',(14.5,136.580604996376,-23.016899728323));
#51582=CARTESIAN_POINT('',(14.3353834448875,136.711134183553,-23.2246208807783));
#51583=CARTESIAN_POINT('',(14.,136.580604996376,-23.016899728323));
#51584=CARTESIAN_POINT('',(14.5,136.97510175753,-23.6446928191972));
#51585=CARTESIAN_POINT('',(14.,136.97510175753,-23.6446928191972));
#51586=CARTESIAN_POINT('',(14.4305329766294,136.920019362628,-23.5570359602482));
#51587=CARTESIAN_POINT('Origin',(57.75,136.084260161474,-23.1369864911307));
#51588=CARTESIAN_POINT('',(58.,136.01656555429,-23.3776469161245));
#51589=CARTESIAN_POINT('',(57.5,136.151954768658,-22.8963260661369));
#51590=CARTESIAN_POINT('Origin',(57.5,136.801453579863,-24.6295005722094));
#51591=CARTESIAN_POINT('',(57.5,136.216030001563,-25.0845072682928));
#51592=CARTESIAN_POINT('',(58.,136.30080033501,-24.5894609761083));
#51593=CARTESIAN_POINT('',(57.5,136.216030001563,-25.0845072682928));
#51594=CARTESIAN_POINT('',(57.5,136.801453579863,-24.6295005722094));
#51595=CARTESIAN_POINT('',(57.5,136.801453579863,-24.6295005722094));
#51596=CARTESIAN_POINT('',(58.,136.30080033501,-24.5894609761083));
#51597=CARTESIAN_POINT('Origin',(14.,136.508741790713,-24.8570039202511));
#51598=CARTESIAN_POINT('',(14.2512407024475,136.508741790713,-24.8570039202511));
#51599=CARTESIAN_POINT('',(14.5,136.801453579863,-24.6295005722094));
#51600=CARTESIAN_POINT('',(14.2590041943422,136.517876989377,-24.8499038021212));
#51601=CARTESIAN_POINT('',(14.,136.801453579863,-24.6295005722094));
#51602=CARTESIAN_POINT('',(14.5,136.216030001563,-25.0845072682928));
#51603=CARTESIAN_POINT('',(14.,136.216030001563,-25.0845072682928));
#51604=CARTESIAN_POINT('',(14.6801520303733,136.004047480112,-25.2492656932831));
#51605=CARTESIAN_POINT('Origin',(57.75,136.55525164161,-24.5860885277927));
#51606=CARTESIAN_POINT('',(58.,136.309049703357,-24.542676483376));
#51607=CARTESIAN_POINT('',(57.5,136.801453579863,-24.6295005722094));
#51608=CARTESIAN_POINT('Origin',(57.75,133.786345373109,-24.6515678871246));
#51609=CARTESIAN_POINT('',(57.5,133.767646782898,-24.9008676318579));
#51610=CARTESIAN_POINT('',(58.,133.805043963321,-24.4022681423913));
#51611=CARTESIAN_POINT('Origin',(14.25,136.084260161474,-23.1369864911307));
#51612=CARTESIAN_POINT('',(14.,136.490947249372,-23.5110842376314));
#51613=CARTESIAN_POINT('',(14.5,137.061925846364,-23.1522889426911));
#51614=CARTESIAN_POINT('',(14.,136.01656555429,-23.3776469161245));
#51615=CARTESIAN_POINT('',(14.5,136.151954768658,-22.8963260661369));
#51616=CARTESIAN_POINT('Origin',(14.,136.71462949103,-25.1219044487155));
#51617=CARTESIAN_POINT('',(14.5,136.801453579863,-24.6295005722094));
#51618=CARTESIAN_POINT('Origin',(14.25,136.55525164161,-24.5860885277927));
#51619=CARTESIAN_POINT('',(14.,136.30080033501,-24.5894609761083));
#51620=CARTESIAN_POINT('',(14.,136.30080033501,-24.5894609761083));
#51621=CARTESIAN_POINT('',(14.,136.309049703357,-24.542676483376));
#51622=CARTESIAN_POINT('Origin',(14.25,133.786345373109,-24.6515678871246));
#51623=CARTESIAN_POINT('',(14.5,133.767646782898,-24.9008676318579));
#51624=CARTESIAN_POINT('',(14.,133.805043963321,-24.4022681423913));
#51625=CARTESIAN_POINT('Origin',(14.,132.705939207914,-24.8212348392527));
#51626=CARTESIAN_POINT('Origin',(14.,137.061925846364,-23.1522889426911));
#51627=CARTESIAN_POINT('Origin',(57.5,138.427485163379,-12.6127455909704));
#51628=CARTESIAN_POINT('',(57.5,137.883945745091,-13.1170438759937));
#51629=CARTESIAN_POINT('',(58.,137.925247374536,-12.6164931630349));
#51630=CARTESIAN_POINT('',(57.5,137.883945745091,-13.1170438759937));
#51631=CARTESIAN_POINT('',(57.5,138.427485163379,-12.6127455909704));
#51632=CARTESIAN_POINT('',(57.5,138.427485163379,-12.6127455909704));
#51633=CARTESIAN_POINT('',(58.,137.925247374536,-12.6164931630349));
#51634=CARTESIAN_POINT('Origin',(57.5,138.066929551123,-11.025529402481));
#51635=CARTESIAN_POINT('',(57.5,138.514640906126,-11.6165508928786));
#51636=CARTESIAN_POINT('',(58.,138.020683996878,-11.5256475780664));
#51637=CARTESIAN_POINT('',(57.5,138.514640906126,-11.6165508928786));
#51638=CARTESIAN_POINT('',(57.5,138.066929551123,-11.025529402481));
#51639=CARTESIAN_POINT('',(57.5,138.066929551123,-11.025529402481));
#51640=CARTESIAN_POINT('',(58.,138.020683996878,-11.5256475780664));
#51641=CARTESIAN_POINT('Origin',(14.,137.925247374536,-12.6164931630349));
#51642=CARTESIAN_POINT('',(14.5,137.883945745091,-13.1170438759937));
#51643=CARTESIAN_POINT('',(14.5,138.427485163379,-12.6127455909704));
#51644=CARTESIAN_POINT('',(14.5,137.883945745091,-13.1170438759937));
#51645=CARTESIAN_POINT('',(14.,137.925247374536,-12.6164931630349));
#51646=CARTESIAN_POINT('',(14.,137.925247374536,-12.6164931630349));
#51647=CARTESIAN_POINT('',(14.5,138.427485163379,-12.6127455909704));
#51648=CARTESIAN_POINT('Origin',(14.25,135.425773646859,-12.8975129283142));
#51649=CARTESIAN_POINT('',(14.,135.422673178871,-12.647532154857));
#51650=CARTESIAN_POINT('',(14.5,135.428874114848,-13.1474937017714));
#51651=CARTESIAN_POINT('Origin',(14.5,138.066929551123,-11.025529402481));
#51652=CARTESIAN_POINT('',(14.,138.020683996878,-11.5256475780664));
#51653=CARTESIAN_POINT('',(14.5,138.514640906126,-11.6165508928786));
#51654=CARTESIAN_POINT('',(14.,138.020683996878,-11.5256475780664));
#51655=CARTESIAN_POINT('',(14.5,138.066929551123,-11.025529402481));
#51656=CARTESIAN_POINT('',(14.5,138.066929551123,-11.025529402481));
#51657=CARTESIAN_POINT('',(14.5,138.514640906126,-11.6165508928786));
#51658=CARTESIAN_POINT('Origin',(14.25,137.582939709175,-11.188418501646));
#51659=CARTESIAN_POINT('',(14.5,137.629401779851,-10.9427738884575));
#51660=CARTESIAN_POINT('',(14.,137.536477638499,-11.4340631148344));
#51661=CARTESIAN_POINT('Origin',(14.,138.290785228625,-11.3210401476798));
#51662=CARTESIAN_POINT('',(14.,138.514640906126,-11.6165508928786));
#51663=CARTESIAN_POINT('',(14.,138.066929551123,-11.025529402481));
#51664=CARTESIAN_POINT('Origin',(14.25,138.178436488856,-12.5909566552835));
#51665=CARTESIAN_POINT('',(14.5,138.427485163379,-12.6127455909704));
#51666=CARTESIAN_POINT('',(14.,137.929387814333,-12.5691677195965));
#51667=CARTESIAN_POINT('Origin',(14.,138.155715454235,-12.864894733482));
#51668=CARTESIAN_POINT('',(14.,137.883945745091,-13.1170438759937));
#51669=CARTESIAN_POINT('',(14.,138.427485163379,-12.6127455909704));
#51670=CARTESIAN_POINT('Origin',(57.75,137.582939709175,-11.188418501646));
#51671=CARTESIAN_POINT('',(58.,137.536477638499,-11.4340631148344));
#51672=CARTESIAN_POINT('',(57.5,137.629401779851,-10.9427738884575));
#51673=CARTESIAN_POINT('Origin',(57.75,138.178436488856,-12.5909566552835));
#51674=CARTESIAN_POINT('',(58.,137.929387814333,-12.5691677195965));
#51675=CARTESIAN_POINT('',(57.5,138.427485163379,-12.6127455909704));
#51676=CARTESIAN_POINT('Origin',(57.75,135.425773646859,-12.8975129283142));
#51677=CARTESIAN_POINT('',(57.5,135.428874114848,-13.1474937017714));
#51678=CARTESIAN_POINT('',(58.,135.422673178871,-12.647532154857));
#51679=CARTESIAN_POINT('Origin',(14.,136.478673638569,-11.9403367564292));
#51680=CARTESIAN_POINT('Origin',(14.,134.364266202539,-13.1606978482623));
#51681=CARTESIAN_POINT('Origin',(14.,138.383907292005,-13.1108429400162));
#51682=CARTESIAN_POINT('Origin',(57.5,139.,-0.500000000000025));
#51683=CARTESIAN_POINT('',(57.5,138.502481404895,-1.04975185951052));
#51684=CARTESIAN_POINT('',(58.,138.5,-0.547506218943981));
#51685=CARTESIAN_POINT('',(57.5,138.502481404895,-1.04975185951052));
#51686=CARTESIAN_POINT('',(57.5,139.,-0.500000000000025));
#51687=CARTESIAN_POINT('',(57.5,139.,-0.500000000000025));
#51688=CARTESIAN_POINT('',(58.,138.5,-0.547506218943981));
#51689=CARTESIAN_POINT('Origin',(57.5,138.502481404895,1.04975185951047));
#51690=CARTESIAN_POINT('',(57.5,139.,0.499999999999975));
#51691=CARTESIAN_POINT('',(58.,138.5,0.547506218943931));
#51692=CARTESIAN_POINT('',(57.5,139.,0.499999999999975));
#51693=CARTESIAN_POINT('',(57.5,138.502481404895,1.04975185951047));
#51694=CARTESIAN_POINT('',(57.5,138.502481404895,1.04975185951047));
#51695=CARTESIAN_POINT('',(58.,138.5,0.547506218943931));
#51696=CARTESIAN_POINT('Origin',(14.,138.5,-0.547506218943981));
#51697=CARTESIAN_POINT('',(14.5,138.502481404895,-1.04975185951052));
#51698=CARTESIAN_POINT('',(14.5,139.,-0.500000000000025));
#51699=CARTESIAN_POINT('',(14.5,138.502481404895,-1.04975185951052));
#51700=CARTESIAN_POINT('',(14.,138.5,-0.547506218943981));
#51701=CARTESIAN_POINT('',(14.,138.5,-0.547506218943981));
#51702=CARTESIAN_POINT('',(14.5,139.,-0.500000000000025));
#51703=CARTESIAN_POINT('Origin',(14.25,136.034530010839,-1.04530010838812));
#51704=CARTESIAN_POINT('',(14.,136.009654081084,-0.796540810835624));
#51705=CARTESIAN_POINT('',(14.5,136.059405940594,-1.29405940594062));
#51706=CARTESIAN_POINT('Origin',(14.5,138.502481404895,1.04975185951047));
#51707=CARTESIAN_POINT('',(14.,138.5,0.54750621894393));
#51708=CARTESIAN_POINT('',(14.5,139.,0.499999999999975));
#51709=CARTESIAN_POINT('',(14.,138.5,0.54750621894393));
#51710=CARTESIAN_POINT('',(14.5,138.502481404895,1.04975185951047));
#51711=CARTESIAN_POINT('',(14.5,138.502481404895,1.04975185951047));
#51712=CARTESIAN_POINT('',(14.5,139.,0.499999999999975));
#51713=CARTESIAN_POINT('Origin',(14.25,138.034530010839,0.845300108388072));
#51714=CARTESIAN_POINT('',(14.5,138.059405940594,1.09405940594057));
#51715=CARTESIAN_POINT('',(14.,138.009654081084,0.596540810835574));
#51716=CARTESIAN_POINT('Origin',(14.,138.751240702448,0.774875929755224));
#51717=CARTESIAN_POINT('',(14.,139.,0.499999999999975));
#51718=CARTESIAN_POINT('',(14.,138.502481404895,1.04975185951047));
#51719=CARTESIAN_POINT('Origin',(14.25,138.75,-0.500000000000025));
#51720=CARTESIAN_POINT('',(14.5,139.,-0.500000000000026));
#51721=CARTESIAN_POINT('',(14.,138.5,-0.500000000000025));
#51722=CARTESIAN_POINT('Origin',(14.,138.751240702448,-0.774875929755274));
#51723=CARTESIAN_POINT('',(14.,138.502481404895,-1.04975185951052));
#51724=CARTESIAN_POINT('',(14.,139.,-0.500000000000025));
#51725=CARTESIAN_POINT('Origin',(57.75,138.034530010839,0.845300108388072));
#51726=CARTESIAN_POINT('',(58.,138.009654081084,0.596540810835575));
#51727=CARTESIAN_POINT('',(57.5,138.059405940594,1.09405940594057));
#51728=CARTESIAN_POINT('Origin',(57.75,138.75,-0.500000000000025));
#51729=CARTESIAN_POINT('',(58.,138.5,-0.500000000000025));
#51730=CARTESIAN_POINT('',(57.5,139.,-0.500000000000026));
#51731=CARTESIAN_POINT('Origin',(57.75,136.034530010839,-1.04530010838812));
#51732=CARTESIAN_POINT('',(57.5,136.059405940594,-1.29405940594062));
#51733=CARTESIAN_POINT('',(58.,136.009654081084,-0.796540810835624));
#51734=CARTESIAN_POINT('Origin',(14.,137.,-2.51664917224781E-14));
#51735=CARTESIAN_POINT('Origin',(14.,135.,-1.40000000000002));
#51736=CARTESIAN_POINT('Origin',(14.,139.,-1.00000000000003));
#51737=CARTESIAN_POINT('Origin',(57.75,135.607981461541,10.8148680765323));
#51738=CARTESIAN_POINT('',(57.7487592975525,138.290785228625,11.3210401476798));
#51739=CARTESIAN_POINT('',(58.,138.020683996878,11.5256475780664));
#51740=CARTESIAN_POINT('',(58.2319907935076,137.771277756289,11.7145781122933));
#51741=CARTESIAN_POINT('',(58.,135.561519390865,11.0605126897207));
#51742=CARTESIAN_POINT('',(57.5,138.066929551123,11.025529402481));
#51743=CARTESIAN_POINT('',(57.5,135.654443532217,10.5692234633438));
#51744=CARTESIAN_POINT('',(50.4896657310026,131.758409054648,2.69768347146864));
#51745=CARTESIAN_POINT('Origin',(58.,136.478673638569,11.9403367564291));
#51746=CARTESIAN_POINT('',(58.,137.925247374536,12.6164931630348));
#51747=CARTESIAN_POINT('',(58.,138.016543557081,11.5729730215047));
#51748=CARTESIAN_POINT('',(58.,137.432493723604,12.6226047007339));
#51749=CARTESIAN_POINT('Origin',(57.75,138.265592231604,11.5947619571917));
#51750=CARTESIAN_POINT('',(57.5,138.514640906126,11.6165508928786));
#51751=CARTESIAN_POINT('',(57.5,138.514640906126,11.6165508928786));
#51752=CARTESIAN_POINT('',(57.5,138.427485163379,12.6127455909703));
#51753=CARTESIAN_POINT('',(57.5,138.514640906126,11.6165508928786));
#51754=CARTESIAN_POINT('',(57.5,138.427485163379,12.6127455909703));
#51755=CARTESIAN_POINT('Origin',(14.,138.290785228625,11.3210401476798));
#51756=CARTESIAN_POINT('',(14.5,138.066929551123,11.025529402481));
#51757=CARTESIAN_POINT('',(14.,138.066929551123,11.025529402481));
#51758=CARTESIAN_POINT('',(14.5,138.514640906126,11.6165508928786));
#51759=CARTESIAN_POINT('',(14.5,138.066929551123,11.025529402481));
#51760=CARTESIAN_POINT('',(14.,138.514640906126,11.6165508928786));
#51761=CARTESIAN_POINT('Origin',(57.5,137.883945745091,13.1170438759936));
#51762=CARTESIAN_POINT('',(57.5,137.883945745091,13.1170438759936));
#51763=CARTESIAN_POINT('',(57.5,137.883945745091,13.1170438759936));
#51764=CARTESIAN_POINT('',(58.,137.925247374536,12.6164931630348));
#51765=CARTESIAN_POINT('Origin',(14.,138.020683996878,11.5256475780664));
#51766=CARTESIAN_POINT('',(14.,138.020683996878,11.5256475780664));
#51767=CARTESIAN_POINT('',(14.,138.020683996878,11.5256475780664));
#51768=CARTESIAN_POINT('',(14.5,138.514640906126,11.6165508928786));
#51769=CARTESIAN_POINT('Origin',(14.25,135.607981461541,10.8148680765323));
#51770=CARTESIAN_POINT('',(14.,135.561519390865,11.0605126897207));
#51771=CARTESIAN_POINT('',(14.5,135.654443532217,10.5692234633438));
#51772=CARTESIAN_POINT('Origin',(14.5,137.883945745091,13.1170438759936));
#51773=CARTESIAN_POINT('',(14.,137.925247374536,12.6164931630348));
#51774=CARTESIAN_POINT('',(14.5,138.427485163379,12.6127455909703));
#51775=CARTESIAN_POINT('',(14.,137.925247374536,12.6164931630348));
#51776=CARTESIAN_POINT('',(14.5,137.883945745091,13.1170438759936));
#51777=CARTESIAN_POINT('',(14.5,137.883945745091,13.1170438759936));
#51778=CARTESIAN_POINT('',(14.5,138.427485163379,12.6127455909703));
#51779=CARTESIAN_POINT('Origin',(14.25,137.435594191592,12.8725854741911));
#51780=CARTESIAN_POINT('',(14.5,137.438694659581,13.1225662476483));
#51781=CARTESIAN_POINT('',(14.,137.432493723604,12.6226047007339));
#51782=CARTESIAN_POINT('Origin',(14.,138.155715454235,12.864894733482));
#51783=CARTESIAN_POINT('',(14.,138.427485163379,12.6127455909703));
#51784=CARTESIAN_POINT('',(14.,137.883945745091,13.1170438759936));
#51785=CARTESIAN_POINT('Origin',(14.25,138.265592231604,11.5947619571917));
#51786=CARTESIAN_POINT('',(14.5,138.514640906126,11.6165508928786));
#51787=CARTESIAN_POINT('',(14.,138.016543557081,11.5729730215047));
#51788=CARTESIAN_POINT('Origin',(57.75,137.435594191592,12.8725854741911));
#51789=CARTESIAN_POINT('',(57.5,137.438694659581,13.1225662476483));
#51790=CARTESIAN_POINT('Origin',(14.,134.608302282232,10.3713526936054));
#51791=CARTESIAN_POINT('Origin',(14.,138.5582187775,11.1184535438327));
#51792=CARTESIAN_POINT('Origin',(57.5,136.97510175753,23.6446928191972));
#51793=CARTESIAN_POINT('',(57.5,136.580604996376,23.016899728323));
#51794=CARTESIAN_POINT('',(58.,136.490947249372,23.5110842376314));
#51795=CARTESIAN_POINT('',(57.5,136.580604996376,23.0168997283229));
#51796=CARTESIAN_POINT('',(57.5,136.97510175753,23.6446928191972));
#51797=CARTESIAN_POINT('',(57.5,136.97510175753,23.6446928191972));
#51798=CARTESIAN_POINT('',(58.,136.490947249372,23.5110842376314));
#51799=CARTESIAN_POINT('Origin',(57.5,136.216030001563,25.0845072682928));
#51800=CARTESIAN_POINT('',(57.5,136.801453579863,24.6295005722094));
#51801=CARTESIAN_POINT('',(58.,136.30080033501,24.5894609761082));
#51802=CARTESIAN_POINT('',(57.5,136.801453579863,24.6295005722094));
#51803=CARTESIAN_POINT('',(57.5,136.216030001563,25.0845072682928));
#51804=CARTESIAN_POINT('',(57.5,136.216030001563,25.0845072682928));
#51805=CARTESIAN_POINT('',(58.,136.30080033501,24.5894609761082));
#51806=CARTESIAN_POINT('Origin',(14.,136.490947249372,23.5110842376314));
#51807=CARTESIAN_POINT('',(14.5,136.580604996376,23.0168997283229));
#51808=CARTESIAN_POINT('',(14.5,136.97510175753,23.6446928191972));
#51809=CARTESIAN_POINT('',(14.5,136.580604996376,23.016899728323));
#51810=CARTESIAN_POINT('',(14.,136.490947249372,23.5110842376314));
#51811=CARTESIAN_POINT('',(14.,136.490947249372,23.5110842376314));
#51812=CARTESIAN_POINT('',(14.5,136.97510175753,23.6446928191972));
#51813=CARTESIAN_POINT('Origin',(14.25,134.149374290983,22.5927285851944));
#51814=CARTESIAN_POINT('',(14.,134.081679683799,22.8333890101882));
#51815=CARTESIAN_POINT('',(14.5,134.217068898167,22.3520681602006));
#51816=CARTESIAN_POINT('Origin',(14.5,136.216030001563,25.0845072682928));
#51817=CARTESIAN_POINT('',(14.,136.30080033501,24.5894609761082));
#51818=CARTESIAN_POINT('',(14.5,136.801453579863,24.6295005722094));
#51819=CARTESIAN_POINT('',(14.,136.30080033501,24.5894609761082));
#51820=CARTESIAN_POINT('',(14.5,136.216030001563,25.0845072682928));
#51821=CARTESIAN_POINT('',(14.5,136.216030001563,25.0845072682928));
#51822=CARTESIAN_POINT('',(14.5,136.801453579863,24.6295005722094));
#51823=CARTESIAN_POINT('Origin',(14.25,135.790690514667,24.801902691856));
#51824=CARTESIAN_POINT('',(14.5,135.771991924456,25.0512024365893));
#51825=CARTESIAN_POINT('',(14.,135.809389104878,24.5526029471226));
#51826=CARTESIAN_POINT('Origin',(14.,136.508741790713,24.8570039202511));
#51827=CARTESIAN_POINT('',(14.,136.801453579863,24.6295005722094));
#51828=CARTESIAN_POINT('',(14.,136.216030001563,25.0845072682928));
#51829=CARTESIAN_POINT('Origin',(14.25,136.728899819277,23.6012807747804));
#51830=CARTESIAN_POINT('',(14.5,136.97510175753,23.6446928191972));
#51831=CARTESIAN_POINT('',(14.,136.482697881024,23.5578687303637));
#51832=CARTESIAN_POINT('Origin',(14.,136.777853376953,23.3307962737601));
#51833=CARTESIAN_POINT('',(14.,136.580604996376,23.016899728323));
#51834=CARTESIAN_POINT('',(14.,136.97510175753,23.6446928191972));
#51835=CARTESIAN_POINT('Origin',(57.75,135.790690514667,24.801902691856));
#51836=CARTESIAN_POINT('',(58.,135.809389104878,24.5526029471226));
#51837=CARTESIAN_POINT('',(57.5,135.771991924456,25.0512024365893));
#51838=CARTESIAN_POINT('Origin',(57.75,136.728899819277,23.6012807747804));
#51839=CARTESIAN_POINT('',(58.,136.482697881024,23.5578687303637));
#51840=CARTESIAN_POINT('',(57.5,136.97510175753,23.6446928191972));
#51841=CARTESIAN_POINT('Origin',(57.75,134.149374290983,22.5927285851944));
#51842=CARTESIAN_POINT('',(57.5,134.217068898167,22.3520681602006));
#51843=CARTESIAN_POINT('',(58.,134.081679683799,22.8333890101882));
#51844=CARTESIAN_POINT('Origin',(14.,134.918662162673,23.7898003403694));
#51845=CARTESIAN_POINT('Origin',(14.,133.192154105382,22.0637731308185));
#51846=CARTESIAN_POINT('Origin',(14.,137.061925846364,23.1522889426911));
#51847=CARTESIAN_POINT('Origin',(57.5,133.511428020236,36.8610624138407));
#51848=CARTESIAN_POINT('',(57.5,134.134280331629,36.4588101823948));
#51849=CARTESIAN_POINT('',(58.,133.639021904261,36.3752881436309));
#51850=CARTESIAN_POINT('',(57.5,134.134280331629,36.4588101823948));
#51851=CARTESIAN_POINT('',(57.5,133.511428020236,36.8610624138407));
#51852=CARTESIAN_POINT('',(57.5,133.511428020236,36.8610624138407));
#51853=CARTESIAN_POINT('',(58.,133.639021904261,36.3752881436309));
#51854=CARTESIAN_POINT('Origin',(14.,133.822854175933,36.6599362981178));
#51855=CARTESIAN_POINT('',(14.2512407024475,133.822854175933,36.6599362981178));
#51856=CARTESIAN_POINT('',(14.5,133.511428020236,36.8610624138407));
#51857=CARTESIAN_POINT('',(14.3353834448874,133.717514391388,36.7279671340291));
#51858=CARTESIAN_POINT('',(14.,133.511428020236,36.8610624138407));
#51859=CARTESIAN_POINT('',(14.5,134.134280331629,36.4588101823948));
#51860=CARTESIAN_POINT('',(14.,134.134280331629,36.4588101823948));
#51861=CARTESIAN_POINT('',(14.4305329766294,134.047313338842,36.5149754502615));
#51862=CARTESIAN_POINT('Origin',(57.75,133.112337690265,36.5424624542375));
#51863=CARTESIAN_POINT('',(58.,133.152693031114,36.2957410598167));
#51864=CARTESIAN_POINT('',(57.5,133.071982349415,36.7891838486583));
#51865=CARTESIAN_POINT('Origin',(57.5,134.393099376732,35.4928843561058));
#51866=CARTESIAN_POINT('',(57.5,134.054819567983,34.8330975492483));
#51867=CARTESIAN_POINT('',(58.,133.922431977811,35.3175873497672));
#51868=CARTESIAN_POINT('',(57.5,134.054819567983,34.8330975492483));
#51869=CARTESIAN_POINT('',(57.5,134.393099376732,35.4928843561058));
#51870=CARTESIAN_POINT('',(57.5,134.393099376732,35.4928843561058));
#51871=CARTESIAN_POINT('',(58.,133.922431977811,35.3175873497672));
#51872=CARTESIAN_POINT('Origin',(14.,134.223959472357,35.1629909526771));
#51873=CARTESIAN_POINT('',(14.2512407024475,134.223959472357,35.1629909526771));
#51874=CARTESIAN_POINT('',(14.5,134.393099376732,35.4928843561058));
#51875=CARTESIAN_POINT('',(14.2590041943422,134.22923813446,35.1732865468069));
#51876=CARTESIAN_POINT('',(14.,134.393099376732,35.4928843561058));
#51877=CARTESIAN_POINT('',(14.5,134.054819567983,34.8330975492483));
#51878=CARTESIAN_POINT('',(14.,134.054819567983,34.8330975492483));
#51879=CARTESIAN_POINT('',(14.6801520303733,133.932328077252,34.5941880209647));
#51880=CARTESIAN_POINT('Origin',(57.75,134.151617920159,35.4281795948302));
#51881=CARTESIAN_POINT('',(58.,133.910136463587,35.3634748335545));
#51882=CARTESIAN_POINT('',(57.5,134.393099376732,35.4928843561058));
#51883=CARTESIAN_POINT('Origin',(57.75,131.669809380463,34.1986447874606));
#51884=CARTESIAN_POINT('',(57.5,131.75822132732,33.9648001218104));
#51885=CARTESIAN_POINT('',(58.,131.581397433607,34.4324894531108));
#51886=CARTESIAN_POINT('Origin',(14.25,133.112337690265,36.5424624542375));
#51887=CARTESIAN_POINT('',(14.,133.639021904261,36.3752881436309));
#51888=CARTESIAN_POINT('',(14.5,134.004870809078,36.9417730955394));
#51889=CARTESIAN_POINT('',(14.,133.152693031114,36.2957410598167));
#51890=CARTESIAN_POINT('',(14.5,133.071982349415,36.7891838486583));
#51891=CARTESIAN_POINT('Origin',(14.,134.522508899283,35.0099214429613));
#51892=CARTESIAN_POINT('',(14.5,134.393099376732,35.4928843561058));
#51893=CARTESIAN_POINT('Origin',(14.25,134.151617920159,35.4281795948302));
#51894=CARTESIAN_POINT('',(14.,133.922431977811,35.3175873497672));
#51895=CARTESIAN_POINT('',(14.,133.922431977811,35.3175873497672));
#51896=CARTESIAN_POINT('',(14.,133.910136463587,35.3634748335545));
#51897=CARTESIAN_POINT('Origin',(14.25,131.669809380463,34.1986447874606));
#51898=CARTESIAN_POINT('',(14.5,131.75822132732,33.9648001218104));
#51899=CARTESIAN_POINT('',(14.,131.581397433607,34.4324894531108));
#51900=CARTESIAN_POINT('Origin',(14.,130.762333212168,33.5882749320355));
#51901=CARTESIAN_POINT('Origin',(14.,134.004870809078,36.9417730955394));
#51902=CARTESIAN_POINT('Origin',(57.5,130.788284360904,47.0709536118749));
#51903=CARTESIAN_POINT('',(57.5,130.508796018164,46.3841944650246));
#51904=CARTESIAN_POINT('',(58.,130.334686134323,46.855302296829));
#51905=CARTESIAN_POINT('',(57.5,130.508796018164,46.3841944650246));
#51906=CARTESIAN_POINT('',(57.5,130.788284360904,47.0709536118749));
#51907=CARTESIAN_POINT('',(57.5,130.788284360904,47.0709536118749));
#51908=CARTESIAN_POINT('',(58.,130.334686134323,46.855302296829));
#51909=CARTESIAN_POINT('Origin',(57.5,129.790723455271,48.3570826171012));
#51910=CARTESIAN_POINT('',(57.5,130.446264217578,48.0106462326609));
#51911=CARTESIAN_POINT('',(58.,129.960169823373,47.8842774043811));
#51912=CARTESIAN_POINT('',(57.5,130.446264217578,48.0106462326609));
#51913=CARTESIAN_POINT('',(57.5,129.790723455271,48.3570826171012));
#51914=CARTESIAN_POINT('',(57.5,129.790723455271,48.3570826171012));
#51915=CARTESIAN_POINT('',(58.,129.960169823373,47.8842774043811));
#51916=CARTESIAN_POINT('Origin',(14.,130.334686134323,46.855302296829));
#51917=CARTESIAN_POINT('',(14.5,130.508796018164,46.3841944650246));
#51918=CARTESIAN_POINT('',(14.5,130.788284360904,47.0709536118749));
#51919=CARTESIAN_POINT('',(14.5,130.508796018164,46.3841944650246));
#51920=CARTESIAN_POINT('',(14.,130.334686134323,46.855302296829));
#51921=CARTESIAN_POINT('',(14.,130.334686134323,46.855302296829));
#51922=CARTESIAN_POINT('',(14.5,130.788284360904,47.0709536118749));
#51923=CARTESIAN_POINT('Origin',(14.25,128.188157716154,45.544288653188));
#51924=CARTESIAN_POINT('',(14.,128.079701297925,45.7695378603897));
#51925=CARTESIAN_POINT('',(14.5,128.296614134382,45.3190394459863));
#51926=CARTESIAN_POINT('Origin',(14.5,129.790723455271,48.3570826171012));
#51927=CARTESIAN_POINT('',(14.,129.960169823373,47.8842774043811));
#51928=CARTESIAN_POINT('',(14.5,130.446264217578,48.0106462326609));
#51929=CARTESIAN_POINT('',(14.,129.960169823373,47.8842774043811));
#51930=CARTESIAN_POINT('',(14.5,129.790723455271,48.3570826171012));
#51931=CARTESIAN_POINT('',(14.5,129.790723455271,48.3570826171012));
#51932=CARTESIAN_POINT('',(14.5,130.446264217578,48.0106462326609));
#51933=CARTESIAN_POINT('Origin',(14.25,129.420919600612,48.0049120124002));
#51934=CARTESIAN_POINT('',(14.5,129.359214637636,48.2471773577224));
#51935=CARTESIAN_POINT('',(14.,129.482624563588,47.762646667078));
#51936=CARTESIAN_POINT('Origin',(14.,130.118493836425,48.183864424881));
#51937=CARTESIAN_POINT('',(14.,130.446264217578,48.0106462326609));
#51938=CARTESIAN_POINT('',(14.,129.790723455271,48.3570826171012));
#51939=CARTESIAN_POINT('Origin',(14.25,130.553361205708,46.9854485760435));
#51940=CARTESIAN_POINT('',(14.5,130.788284360904,47.0709536118749));
#51941=CARTESIAN_POINT('',(14.,130.318438050511,46.8999435402121));
#51942=CARTESIAN_POINT('Origin',(14.,130.648540189534,46.7275740384498));
#51943=CARTESIAN_POINT('',(14.,130.508796018164,46.3841944650246));
#51944=CARTESIAN_POINT('',(14.,130.788284360904,47.0709536118749));
#51945=CARTESIAN_POINT('Origin',(57.75,129.420919600612,48.0049120124002));
#51946=CARTESIAN_POINT('',(58.,129.482624563588,47.762646667078));
#51947=CARTESIAN_POINT('',(57.5,129.359214637636,48.2471773577224));
#51948=CARTESIAN_POINT('Origin',(57.75,130.553361205708,46.9854485760435));
#51949=CARTESIAN_POINT('',(58.,130.318438050511,46.8999435402121));
#51950=CARTESIAN_POINT('',(57.5,130.788284360904,47.0709536118749));
#51951=CARTESIAN_POINT('Origin',(57.75,128.188157716154,45.544288653188));
#51952=CARTESIAN_POINT('',(57.5,128.296614134382,45.3190394459863));
#51953=CARTESIAN_POINT('',(58.,128.079701297925,45.7695378603897));
#51954=CARTESIAN_POINT('Origin',(14.,128.737889047669,46.8567596356165));
#51955=CARTESIAN_POINT('Origin',(14.,127.337332006754,44.8571496798649));
#51956=CARTESIAN_POINT('Origin',(14.,130.959294432567,46.601107301482));
#51957=CARTESIAN_POINT('Origin',(57.5,126.188091528965,58.2907844884388));
#51958=CARTESIAN_POINT('',(57.5,125.969521727281,57.5822796533796));
#51959=CARTESIAN_POINT('',(58.,125.755014631118,58.0364201014069));
#51960=CARTESIAN_POINT('',(57.5,125.969521727281,57.5822796533796));
#51961=CARTESIAN_POINT('',(57.5,126.188091528965,58.2907844884388));
#51962=CARTESIAN_POINT('',(57.5,126.188091528965,58.2907844884388));
#51963=CARTESIAN_POINT('',(58.,125.755014631118,58.0364201014069));
#51964=CARTESIAN_POINT('Origin',(57.5,125.08223311503,59.4850762228408));
#51965=CARTESIAN_POINT('',(57.5,125.765473267224,59.1970922754755));
#51966=CARTESIAN_POINT('',(58.,125.292242378034,59.0288384007667));
#51967=CARTESIAN_POINT('',(57.5,125.765473267224,59.1970922754755));
#51968=CARTESIAN_POINT('',(57.5,125.08223311503,59.4850762228408));
#51969=CARTESIAN_POINT('',(57.5,125.08223311503,59.4850762228408));
#51970=CARTESIAN_POINT('',(58.,125.292242378034,59.0288384007667));
#51971=CARTESIAN_POINT('Origin',(14.,125.755014631118,58.0364201014069));
#51972=CARTESIAN_POINT('',(14.5,125.969521727281,57.5822796533796));
#51973=CARTESIAN_POINT('',(14.5,126.188091528965,58.2907844884388));
#51974=CARTESIAN_POINT('',(14.5,125.969521727281,57.5822796533796));
#51975=CARTESIAN_POINT('',(14.,125.755014631118,58.0364201014069));
#51976=CARTESIAN_POINT('',(14.,125.755014631118,58.0364201014069));
#51977=CARTESIAN_POINT('',(14.5,126.188091528965,58.2907844884388));
#51978=CARTESIAN_POINT('Origin',(14.25,123.730916769498,56.5433129818712));
#51979=CARTESIAN_POINT('',(14.,123.603241298728,56.7582524481485));
#51980=CARTESIAN_POINT('',(14.5,123.858592240269,56.328373515594));
#51981=CARTESIAN_POINT('Origin',(14.5,125.08223311503,59.4850762228408));
#51982=CARTESIAN_POINT('',(14.,125.292242378034,59.0288384007667));
#51983=CARTESIAN_POINT('',(14.5,125.765473267224,59.1970922754755));
#51984=CARTESIAN_POINT('',(14.,125.292242378034,59.0288384007667));
#51985=CARTESIAN_POINT('',(14.5,125.08223311503,59.4850762228408));
#51986=CARTESIAN_POINT('',(14.5,125.08223311503,59.4850762228408));
#51987=CARTESIAN_POINT('',(14.5,125.765473267224,59.1970922754755));
#51988=CARTESIAN_POINT('Origin',(14.25,124.744530166311,59.1020152039901));
#51989=CARTESIAN_POINT('',(14.5,124.661945193235,59.337980714652));
#51990=CARTESIAN_POINT('',(14.,124.827115139388,58.8660496933281));
#51991=CARTESIAN_POINT('Origin',(14.,125.423853191127,59.3410842491581));
#51992=CARTESIAN_POINT('',(14.,125.765473267224,59.1970922754755));
#51993=CARTESIAN_POINT('',(14.,125.08223311503,59.4850762228408));
#51994=CARTESIAN_POINT('Origin',(14.25,125.961514582206,58.1851299230036));
#51995=CARTESIAN_POINT('',(14.5,126.188091528965,58.2907844884388));
#51996=CARTESIAN_POINT('',(14.,125.734937635446,58.0794753575685));
#51997=CARTESIAN_POINT('Origin',(14.,126.078806628123,57.9365320709092));
#51998=CARTESIAN_POINT('',(14.,125.969521727281,57.5822796533796));
#51999=CARTESIAN_POINT('',(14.,126.188091528965,58.2907844884388));
#52000=CARTESIAN_POINT('Origin',(57.75,124.744530166311,59.1020152039901));
#52001=CARTESIAN_POINT('',(58.,124.827115139388,58.8660496933281));
#52002=CARTESIAN_POINT('',(57.5,124.661945193235,59.337980714652));
#52003=CARTESIAN_POINT('Origin',(57.75,125.961514582206,58.1851299230036));
#52004=CARTESIAN_POINT('',(58.,125.734937635446,58.0794753575685));
#52005=CARTESIAN_POINT('',(57.5,126.188091528965,58.2907844884388));
#52006=CARTESIAN_POINT('Origin',(57.75,123.730916769498,56.5433129818712));
#52007=CARTESIAN_POINT('',(57.5,123.858592240269,56.328373515594));
#52008=CARTESIAN_POINT('',(58.,123.603241298728,56.7582524481485));
#52009=CARTESIAN_POINT('Origin',(14.,124.164166824021,57.8987018584757));
#52010=CARTESIAN_POINT('Origin',(14.,122.943216816385,55.784634433143));
#52011=CARTESIAN_POINT('Origin',(14.,126.399400659835,57.8376305949205));
#52012=CARTESIAN_POINT('Origin',(57.75,118.332008835457,67.1120085569767));
#52013=CARTESIAN_POINT('',(57.7487592975525,120.549537219807,68.7045581112747));
#52014=CARTESIAN_POINT('',(58.,120.218271533617,68.7758457056646));
#52015=CARTESIAN_POINT('',(58.2319907935076,119.912387221671,68.8416712881784));
#52016=CARTESIAN_POINT('',(58.,118.18608599957,67.3150024632071));
#52017=CARTESIAN_POINT('',(57.5,120.471543313576,68.3421289244415));
#52018=CARTESIAN_POINT('',(57.5,118.477931671344,66.9090146507463));
#52019=CARTESIAN_POINT('',(50.4896657310029,118.273581834349,58.1284413415477));
#52020=CARTESIAN_POINT('Origin',(58.,118.645480318468,68.5));
#52021=CARTESIAN_POINT('',(58.,119.670765314673,69.7241542943354));
#52022=CARTESIAN_POINT('',(58.,120.194518424145,68.8169872981078));
#52023=CARTESIAN_POINT('',(58.,119.221595996303,69.5214465371196));
#52024=CARTESIAN_POINT('Origin',(57.75,120.411024775091,68.9419872981078));
#52025=CARTESIAN_POINT('',(57.5,120.627531126037,69.0669872981078));
#52026=CARTESIAN_POINT('',(57.5,120.627531126037,69.0669872981078));
#52027=CARTESIAN_POINT('',(57.5,120.127531126037,69.9330127018922));
#52028=CARTESIAN_POINT('',(57.5,120.627531126037,69.0669872981078));
#52029=CARTESIAN_POINT('',(57.5,120.127531126037,69.9330127018922));
#52030=CARTESIAN_POINT('Origin',(14.,120.549537219807,68.7045581112747));
#52031=CARTESIAN_POINT('',(14.5,120.471543313576,68.3421289244415));
#52032=CARTESIAN_POINT('',(14.,120.471543313576,68.3421289244415));
#52033=CARTESIAN_POINT('',(14.5,120.627531126037,69.0669872981078));
#52034=CARTESIAN_POINT('',(14.5,120.471543313576,68.3421289244415));
#52035=CARTESIAN_POINT('',(14.,120.627531126037,69.0669872981078));
#52036=CARTESIAN_POINT('Origin',(57.5,119.421791454066,70.1603524804536));
#52037=CARTESIAN_POINT('',(57.5,119.421791454066,70.1603524804536));
#52038=CARTESIAN_POINT('',(57.5,119.421791454066,70.1603524804536));
#52039=CARTESIAN_POINT('',(58.,119.670765314673,69.7241542943354));
#52040=CARTESIAN_POINT('Origin',(14.,120.218271533617,68.7758457056646));
#52041=CARTESIAN_POINT('',(14.,120.218271533617,68.7758457056646));
#52042=CARTESIAN_POINT('',(14.,120.218271533617,68.7758457056646));
#52043=CARTESIAN_POINT('',(14.5,120.627531126037,69.0669872981078));
#52044=CARTESIAN_POINT('Origin',(14.25,118.332008835457,67.1120085569767));
#52045=CARTESIAN_POINT('',(14.,118.18608599957,67.3150024632071));
#52046=CARTESIAN_POINT('',(14.5,118.477931671344,66.9090146507463));
#52047=CARTESIAN_POINT('Origin',(14.5,119.421791454066,70.1603524804536));
#52048=CARTESIAN_POINT('',(14.,119.670765314673,69.7241542943354));
#52049=CARTESIAN_POINT('',(14.5,120.127531126037,69.9330127018922));
#52050=CARTESIAN_POINT('',(14.,119.670765314673,69.7241542943354));
#52051=CARTESIAN_POINT('',(14.5,119.421791454066,70.1603524804536));
#52052=CARTESIAN_POINT('',(14.5,119.421791454066,70.1603524804536));
#52053=CARTESIAN_POINT('',(14.5,120.127531126037,69.9330127018922));
#52054=CARTESIAN_POINT('Origin',(14.25,119.118759534638,69.7493163731053));
#52055=CARTESIAN_POINT('',(14.5,119.015923072972,69.9771862090909));
#52056=CARTESIAN_POINT('',(14.,119.221595996303,69.5214465371196));
#52057=CARTESIAN_POINT('Origin',(14.,119.774661290051,70.0466825911729));
#52058=CARTESIAN_POINT('',(14.,120.127531126037,69.9330127018922));
#52059=CARTESIAN_POINT('',(14.,119.421791454066,70.1603524804536));
#52060=CARTESIAN_POINT('Origin',(14.25,120.411024775091,68.9419872981078));
#52061=CARTESIAN_POINT('',(14.5,120.627531126037,69.0669872981078));
#52062=CARTESIAN_POINT('',(14.,120.194518424145,68.8169872981078));
#52063=CARTESIAN_POINT('Origin',(57.75,119.118759534638,69.7493163731053));
#52064=CARTESIAN_POINT('',(57.5,119.015923072972,69.9771862090909));
#52065=CARTESIAN_POINT('Origin',(14.,117.613429510899,66.2875644347018));
#52066=CARTESIAN_POINT('Origin',(14.,120.877531126037,68.6339745962156));
#52067=CARTESIAN_POINT('Origin',(57.5,114.148922374345,79.3175486306509));
#52068=CARTESIAN_POINT('',(57.5,114.056703712549,78.5818533282825));
#52069=CARTESIAN_POINT('',(58.,113.766594799967,78.991845596111));
#52070=CARTESIAN_POINT('',(57.5,114.056703712549,78.5818533282825));
#52071=CARTESIAN_POINT('',(57.5,114.148922374345,79.3175486306509));
#52072=CARTESIAN_POINT('',(57.5,114.148922374345,79.3175486306509));
#52073=CARTESIAN_POINT('',(58.,113.766594799967,78.991845596111));
#52074=CARTESIAN_POINT('Origin',(57.5,112.852477851287,80.3016660917109));
#52075=CARTESIAN_POINT('',(57.5,113.575345937994,80.1367006749399));
#52076=CARTESIAN_POINT('',(58.,113.138521468083,79.8888272731288));
#52077=CARTESIAN_POINT('',(57.5,113.575345937994,80.1367006749399));
#52078=CARTESIAN_POINT('',(57.5,112.852477851287,80.3016660917109));
#52079=CARTESIAN_POINT('',(57.5,112.852477851287,80.3016660917109));
#52080=CARTESIAN_POINT('',(58.,113.138521468083,79.8888272731288));
#52081=CARTESIAN_POINT('Origin',(14.,113.766594799967,78.991845596111));
#52082=CARTESIAN_POINT('',(14.5,114.056703712549,78.5818533282825));
#52083=CARTESIAN_POINT('',(14.5,114.148922374345,79.3175486306509));
#52084=CARTESIAN_POINT('',(14.5,114.056703712549,78.5818533282825));
#52085=CARTESIAN_POINT('',(14.,113.766594799967,78.991845596111));
#52086=CARTESIAN_POINT('',(14.,113.766594799967,78.991845596111));
#52087=CARTESIAN_POINT('',(14.5,114.148922374345,79.3175486306509));
#52088=CARTESIAN_POINT('Origin',(14.25,112.032522863357,77.1699412236247));
#52089=CARTESIAN_POINT('',(14.,111.869463223246,77.3594446636108));
#52090=CARTESIAN_POINT('',(14.5,112.195582503469,76.9804377836387));
#52091=CARTESIAN_POINT('Origin',(14.5,112.852477851287,80.3016660917109));
#52092=CARTESIAN_POINT('',(14.,113.138521468083,79.8888272731288));
#52093=CARTESIAN_POINT('',(14.5,113.575345937994,80.1367006749399));
#52094=CARTESIAN_POINT('',(14.,113.138521468083,79.8888272731288));
#52095=CARTESIAN_POINT('',(14.5,112.852477851287,80.3016660917109));
#52096=CARTESIAN_POINT('',(14.5,112.852477851287,80.3016660917109));
#52097=CARTESIAN_POINT('',(14.5,113.575345937994,80.1367006749399));
#52098=CARTESIAN_POINT('Origin',(14.25,112.586423217032,79.8657831288323));
#52099=CARTESIAN_POINT('',(14.5,112.464117914346,80.0838230630982));
#52100=CARTESIAN_POINT('',(14.,112.708728519719,79.6477431945663));
#52101=CARTESIAN_POINT('Origin',(14.,113.213911894641,80.2191833833254));
#52102=CARTESIAN_POINT('',(14.,113.575345937994,80.1367006749399));
#52103=CARTESIAN_POINT('',(14.,112.852477851287,80.3016660917109));
#52104=CARTESIAN_POINT('Origin',(14.25,113.944134363273,79.1741545215632));
#52105=CARTESIAN_POINT('',(14.5,114.148922374345,79.3175486306509));
#52106=CARTESIAN_POINT('',(14.,113.739346352201,79.0307604124754));
#52107=CARTESIAN_POINT('Origin',(14.,114.102813043447,78.9497009794667));
#52108=CARTESIAN_POINT('',(14.,114.056703712549,78.5818533282825));
#52109=CARTESIAN_POINT('',(14.,114.148922374345,79.3175486306509));
#52110=CARTESIAN_POINT('Origin',(57.75,112.586423217032,79.8657831288323));
#52111=CARTESIAN_POINT('',(58.,112.708728519719,79.6477431945663));
#52112=CARTESIAN_POINT('',(57.5,112.464117914346,80.0838230630982));
#52113=CARTESIAN_POINT('Origin',(57.75,113.944134363273,79.1741545215632));
#52114=CARTESIAN_POINT('',(58.,113.739346352201,79.0307604124754));
#52115=CARTESIAN_POINT('',(57.5,114.148922374345,79.3175486306509));
#52116=CARTESIAN_POINT('Origin',(57.75,112.032522863357,77.1699412236247));
#52117=CARTESIAN_POINT('',(57.5,112.195582503469,76.9804377836387));
#52118=CARTESIAN_POINT('',(58.,111.869463223246,77.3594446636108));
#52119=CARTESIAN_POINT('Origin',(14.,112.223830067592,78.5799717800933));
#52120=CARTESIAN_POINT('Origin',(14.,111.388532989905,76.2860060453866));
#52121=CARTESIAN_POINT('Origin',(14.,114.435710592521,78.9079726085064));
#52122=CARTESIAN_POINT('Origin',(57.5,105.424288749871,89.8318355365386));
#52123=CARTESIAN_POINT('',(57.5,106.158783788695,89.7304999679884));
#52124=CARTESIAN_POINT('',(58.,105.745225158215,89.4454980381808));
#52125=CARTESIAN_POINT('',(57.5,106.158783788695,89.7304999679884));
#52126=CARTESIAN_POINT('',(57.5,105.424288749871,89.8318355365386));
#52127=CARTESIAN_POINT('',(57.5,105.424288749871,89.8318355365386));
#52128=CARTESIAN_POINT('',(58.,105.745225158215,89.4454980381808));
#52129=CARTESIAN_POINT('Origin',(14.,105.791536269283,89.7811677522635));
#52130=CARTESIAN_POINT('',(14.2512407024475,105.791536269283,89.7811677522635));
#52131=CARTESIAN_POINT('',(14.5,105.424288749871,89.8318355365386));
#52132=CARTESIAN_POINT('',(14.3353834448875,105.667314928647,89.7983061119719));
#52133=CARTESIAN_POINT('',(14.,105.424288749871,89.8318355365386));
#52134=CARTESIAN_POINT('',(14.5,106.158783788695,89.7304999679884));
#52135=CARTESIAN_POINT('',(14.,106.158783788695,89.7304999679884));
#52136=CARTESIAN_POINT('',(14.4305329766294,106.056228458041,89.7446491482965));
#52137=CARTESIAN_POINT('Origin',(57.75,105.197236237204,89.3744230506705));
#52138=CARTESIAN_POINT('',(58.,105.338079563709,89.1678724336801));
#52139=CARTESIAN_POINT('',(57.5,105.0563929107,89.5809736676609));
#52140=CARTESIAN_POINT('Origin',(57.5,106.801571398381,88.9644555248695));
#52141=CARTESIAN_POINT('',(57.5,106.773823726948,88.223522379275));
#52142=CARTESIAN_POINT('',(58.,106.449085585742,88.6066698449906));
#52143=CARTESIAN_POINT('',(57.5,106.773823726948,88.223522379275));
#52144=CARTESIAN_POINT('',(57.5,106.801571398381,88.9644555248695));
#52145=CARTESIAN_POINT('',(57.5,106.801571398381,88.9644555248695));
#52146=CARTESIAN_POINT('',(58.,106.449085585742,88.6066698449906));
#52147=CARTESIAN_POINT('Origin',(14.,106.787697562665,88.5939889520722));
#52148=CARTESIAN_POINT('',(14.2512407024475,106.787697562665,88.5939889520722));
#52149=CARTESIAN_POINT('',(14.5,106.801571398381,88.9644555248695));
#52150=CARTESIAN_POINT('',(14.2590041943422,106.788130549139,88.6055507882064));
#52151=CARTESIAN_POINT('',(14.,106.801571398381,88.9644555248695));
#52152=CARTESIAN_POINT('',(14.5,106.773823726948,88.223522379275));
#52153=CARTESIAN_POINT('',(14.,106.773823726948,88.223522379275));
#52154=CARTESIAN_POINT('',(14.6801520303733,106.76377626461,87.9552296725038));
#52155=CARTESIAN_POINT('Origin',(57.75,106.610060287601,88.8037586224478));
#52156=CARTESIAN_POINT('',(58.,106.418549176822,88.6430617200262));
#52157=CARTESIAN_POINT('',(57.5,106.801571398381,88.9644555248695));
#52158=CARTESIAN_POINT('Origin',(57.75,104.880401745181,86.6405640410765));
#52159=CARTESIAN_POINT('',(57.5,105.059357207198,86.4659933029383));
#52160=CARTESIAN_POINT('',(58.,104.701446283163,86.8151347792147));
#52161=CARTESIAN_POINT('Origin',(14.25,105.197236237204,89.3744230506705));
#52162=CARTESIAN_POINT('',(14.,105.745225158215,89.4454980381808));
#52163=CARTESIAN_POINT('',(14.5,105.837389983851,90.1135221895479));
#52164=CARTESIAN_POINT('',(14.,105.338079563709,89.1678724336801));
#52165=CARTESIAN_POINT('',(14.5,105.0563929107,89.5809736676609));
#52166=CARTESIAN_POINT('Origin',(14.,107.122965203225,88.58143330331));
#52167=CARTESIAN_POINT('',(14.5,106.801571398381,88.9644555248695));
#52168=CARTESIAN_POINT('Origin',(14.25,106.610060287601,88.8037586224478));
#52169=CARTESIAN_POINT('',(14.,106.449085585742,88.6066698449906));
#52170=CARTESIAN_POINT('',(14.,106.449085585742,88.6066698449906));
#52171=CARTESIAN_POINT('',(14.,106.418549176822,88.6430617200262));
#52172=CARTESIAN_POINT('Origin',(14.25,104.880401745181,86.6405640410765));
#52173=CARTESIAN_POINT('',(14.5,105.059357207198,86.4659933029383));
#52174=CARTESIAN_POINT('',(14.,104.701446283163,86.8151347792147));
#52175=CARTESIAN_POINT('Origin',(14.,104.315902474623,85.7038650873162));
#52176=CARTESIAN_POINT('Origin',(14.,105.837389983851,90.1135221895479));
#52177=CARTESIAN_POINT('Origin',(57.5,98.6413959755234,97.9342891943368));
#52178=CARTESIAN_POINT('',(57.5,98.6783304709881,97.1937571541419));
#52179=CARTESIAN_POINT('',(58.,98.3214345544939,97.5471438341797));
#52180=CARTESIAN_POINT('',(57.5,98.6783304709881,97.1937571541419));
#52181=CARTESIAN_POINT('',(57.5,98.6413959755234,97.9342891943368));
#52182=CARTESIAN_POINT('',(57.5,98.6413959755234,97.9342891943368));
#52183=CARTESIAN_POINT('',(58.,98.3214345544939,97.5471438341797));
#52184=CARTESIAN_POINT('Origin',(57.5,97.1937571541419,98.678330470988));
#52185=CARTESIAN_POINT('',(57.5,97.9342891943369,98.6413959755234));
#52186=CARTESIAN_POINT('',(58.,97.5471438341798,98.3214345544939));
#52187=CARTESIAN_POINT('',(57.5,97.9342891943369,98.6413959755234));
#52188=CARTESIAN_POINT('',(57.5,97.1937571541419,98.678330470988));
#52189=CARTESIAN_POINT('',(57.5,97.1937571541419,98.678330470988));
#52190=CARTESIAN_POINT('',(58.,97.5471438341798,98.3214345544939));
#52191=CARTESIAN_POINT('Origin',(14.,98.3214345544939,97.5471438341797));
#52192=CARTESIAN_POINT('',(14.5,98.6783304709881,97.1937571541419));
#52193=CARTESIAN_POINT('',(14.5,98.6413959755234,97.9342891943368));
#52194=CARTESIAN_POINT('',(14.5,98.6783304709881,97.1937571541419));
#52195=CARTESIAN_POINT('',(14.,98.3214345544939,97.5471438341797));
#52196=CARTESIAN_POINT('',(14.,98.3214345544939,97.5471438341797));
#52197=CARTESIAN_POINT('',(14.5,98.6413959755234,97.9342891943368));
#52198=CARTESIAN_POINT('Origin',(14.25,96.9300774412053,95.4517998511728));
#52199=CARTESIAN_POINT('',(14.,96.7365881164045,95.6101092987371));
#52200=CARTESIAN_POINT('',(14.5,97.1235667660061,95.2934904036084));
#52201=CARTESIAN_POINT('Origin',(14.5,97.1937571541419,98.678330470988));
#52202=CARTESIAN_POINT('',(14.,97.5471438341798,98.3214345544939));
#52203=CARTESIAN_POINT('',(14.5,97.9342891943369,98.6413959755234));
#52204=CARTESIAN_POINT('',(14.,97.5471438341798,98.3214345544939));
#52205=CARTESIAN_POINT('',(14.5,97.1937571541419,98.678330470988));
#52206=CARTESIAN_POINT('',(14.5,97.1937571541419,98.678330470988));
#52207=CARTESIAN_POINT('',(14.5,97.9342891943369,98.6413959755234));
#52208=CARTESIAN_POINT('Origin',(14.25,97.0074347697832,98.2028696473411));
#52209=CARTESIAN_POINT('',(14.5,96.8491253222189,98.3963589721419));
#52210=CARTESIAN_POINT('',(14.,97.1657442173475,98.0093803225402));
#52211=CARTESIAN_POINT('Origin',(14.,97.5640231742394,98.6598632232557));
#52212=CARTESIAN_POINT('',(14.,97.9342891943369,98.6413959755234));
#52213=CARTESIAN_POINT('',(14.,97.1937571541419,98.678330470988));
#52214=CARTESIAN_POINT('Origin',(14.25,98.4646192802268,97.7575124990402));
#52215=CARTESIAN_POINT('',(14.5,98.6413959755234,97.9342891943368));
#52216=CARTESIAN_POINT('',(14.,98.2878425849301,97.5807358037436));
#52217=CARTESIAN_POINT('Origin',(14.,98.6598632232557,97.5640231742393));
#52218=CARTESIAN_POINT('',(14.,98.6783304709881,97.1937571541419));
#52219=CARTESIAN_POINT('',(14.,98.6413959755234,97.9342891943368));
#52220=CARTESIAN_POINT('Origin',(57.75,97.0074347697832,98.2028696473411));
#52221=CARTESIAN_POINT('',(58.,97.1657442173475,98.0093803225402));
#52222=CARTESIAN_POINT('',(57.5,96.8491253222189,98.3963589721419));
#52223=CARTESIAN_POINT('Origin',(57.75,98.4646192802268,97.7575124990402));
#52224=CARTESIAN_POINT('',(58.,98.2878425849301,97.5807358037436));
#52225=CARTESIAN_POINT('',(57.5,98.6413959755234,97.9342891943368));
#52226=CARTESIAN_POINT('Origin',(57.75,96.9300774412053,95.4517998511728));
#52227=CARTESIAN_POINT('',(57.5,97.1235667660061,95.2934904036084));
#52228=CARTESIAN_POINT('',(58.,96.7365881164045,95.6101092987371));
#52229=CARTESIAN_POINT('Origin',(14.,96.873629022557,96.873629022557));
#52230=CARTESIAN_POINT('Origin',(14.,96.4493649538451,94.4694659665227));
#52231=CARTESIAN_POINT('Origin',(14.,98.9949493661167,97.5807358037436));
#52232=CARTESIAN_POINT('Origin',(57.5,89.7304999679885,106.158783788695));
#52233=CARTESIAN_POINT('',(57.5,89.8318355365387,105.424288749871));
#52234=CARTESIAN_POINT('',(58.,89.4454980381808,105.745225158215));
#52235=CARTESIAN_POINT('',(57.5,89.8318355365387,105.424288749871));
#52236=CARTESIAN_POINT('',(57.5,89.7304999679885,106.158783788695));
#52237=CARTESIAN_POINT('',(57.5,89.7304999679885,106.158783788695));
#52238=CARTESIAN_POINT('',(58.,89.4454980381808,105.745225158215));
#52239=CARTESIAN_POINT('Origin',(57.5,88.223522379275,106.773823726948));
#52240=CARTESIAN_POINT('',(57.5,88.9644555248695,106.801571398381));
#52241=CARTESIAN_POINT('',(58.,88.6066698449906,106.449085585742));
#52242=CARTESIAN_POINT('',(57.5,88.9644555248695,106.801571398381));
#52243=CARTESIAN_POINT('',(57.5,88.223522379275,106.773823726948));
#52244=CARTESIAN_POINT('',(57.5,88.223522379275,106.773823726948));
#52245=CARTESIAN_POINT('',(58.,88.6066698449906,106.449085585742));
#52246=CARTESIAN_POINT('Origin',(14.,89.4454980381808,105.745225158215));
#52247=CARTESIAN_POINT('',(14.5,89.8318355365387,105.424288749871));
#52248=CARTESIAN_POINT('',(14.5,89.7304999679885,106.158783788695));
#52249=CARTESIAN_POINT('',(14.5,89.8318355365387,105.424288749871));
#52250=CARTESIAN_POINT('',(14.,89.4454980381808,105.745225158215));
#52251=CARTESIAN_POINT('',(14.,89.4454980381808,105.745225158215));
#52252=CARTESIAN_POINT('',(14.5,89.7304999679885,106.158783788695));
#52253=CARTESIAN_POINT('Origin',(14.25,88.2420567199213,103.536589829029));
#52254=CARTESIAN_POINT('',(14.,88.0355061029309,103.677433155534));
#52255=CARTESIAN_POINT('',(14.5,88.4486073369117,103.395746502524));
#52256=CARTESIAN_POINT('Origin',(14.5,88.223522379275,106.773823726948));
#52257=CARTESIAN_POINT('',(14.,88.6066698449906,106.449085585742));
#52258=CARTESIAN_POINT('',(14.5,88.9644555248695,106.801571398381));
#52259=CARTESIAN_POINT('',(14.,88.6066698449906,106.449085585742));
#52260=CARTESIAN_POINT('',(14.5,88.223522379275,106.773823726948));
#52261=CARTESIAN_POINT('',(14.5,88.223522379275,106.773823726948));
#52262=CARTESIAN_POINT('',(14.5,88.9644555248695,106.801571398381));
#52263=CARTESIAN_POINT('Origin',(14.25,88.0793481490734,106.283933109481));
#52264=CARTESIAN_POINT('',(14.5,87.9047774109353,106.462888571499));
#52265=CARTESIAN_POINT('',(14.,88.2539188872116,106.104977647464));
#52266=CARTESIAN_POINT('Origin',(14.,88.5939889520723,106.787697562665));
#52267=CARTESIAN_POINT('',(14.,88.9644555248695,106.801571398381));
#52268=CARTESIAN_POINT('',(14.,88.223522379275,106.773823726948));
#52269=CARTESIAN_POINT('Origin',(14.25,89.5698030655669,105.967272677915));
#52270=CARTESIAN_POINT('',(14.5,89.7304999679885,106.158783788695));
#52271=CARTESIAN_POINT('',(14.,89.4091061631452,105.775761567135));
#52272=CARTESIAN_POINT('Origin',(14.,89.7811677522636,105.791536269283));
#52273=CARTESIAN_POINT('',(14.,89.8318355365387,105.424288749871));
#52274=CARTESIAN_POINT('',(14.,89.7304999679885,106.158783788695));
#52275=CARTESIAN_POINT('Origin',(57.75,88.0793481490734,106.283933109481));
#52276=CARTESIAN_POINT('',(58.,88.2539188872116,106.104977647464));
#52277=CARTESIAN_POINT('',(57.5,87.9047774109353,106.462888571499));
#52278=CARTESIAN_POINT('Origin',(57.75,89.5698030655669,105.967272677915));
#52279=CARTESIAN_POINT('',(58.,89.4091061631452,105.775761567135));
#52280=CARTESIAN_POINT('',(57.5,89.7304999679885,106.158783788695));
#52281=CARTESIAN_POINT('Origin',(57.75,88.2420567199213,103.536589829029));
#52282=CARTESIAN_POINT('',(57.5,88.4486073369117,103.395746502524));
#52283=CARTESIAN_POINT('',(58.,88.0355061029309,103.677433155534));
#52284=CARTESIAN_POINT('Origin',(14.,88.0619025270559,104.9480887073));
#52285=CARTESIAN_POINT('Origin',(14.,87.8487895280494,102.516097167501));
#52286=CARTESIAN_POINT('Origin',(14.,90.113522189548,105.837389983851));
#52287=CARTESIAN_POINT('Origin',(57.75,78.882460664988,110.833403841184));
#52288=CARTESIAN_POINT('',(57.7487592975525,80.2191833833255,113.213911894641));
#52289=CARTESIAN_POINT('',(58.,79.8888272731288,113.138521468083));
#52290=CARTESIAN_POINT('',(58.2319907935076,79.5837828460196,113.068907409893));
#52291=CARTESIAN_POINT('',(58.,78.6644207307221,110.955709143871));
#52292=CARTESIAN_POINT('',(57.5,80.301666091711,112.852477851287));
#52293=CARTESIAN_POINT('',(57.5,79.100500599254,110.711098538497));
#52294=CARTESIAN_POINT('',(50.4896657310026,82.6261273797262,102.666834600827));
#52295=CARTESIAN_POINT('Origin',(58.,78.5799717800934,112.223830067592));
#52296=CARTESIAN_POINT('',(58.,78.9918455961111,113.766594799967));
#52297=CARTESIAN_POINT('',(58.,79.8499124567644,113.16576991585));
#52298=CARTESIAN_POINT('',(58.,78.6704279451708,113.393052024553));
#52299=CARTESIAN_POINT('Origin',(57.75,79.9933065658522,113.370557926922));
#52300=CARTESIAN_POINT('',(57.5,80.13670067494,113.575345937994));
#52301=CARTESIAN_POINT('',(57.5,80.13670067494,113.575345937994));
#52302=CARTESIAN_POINT('',(57.5,79.317548630651,114.148922374345));
#52303=CARTESIAN_POINT('',(57.5,80.13670067494,113.575345937994));
#52304=CARTESIAN_POINT('',(57.5,79.317548630651,114.148922374345));
#52305=CARTESIAN_POINT('Origin',(14.,80.2191833833255,113.213911894641));
#52306=CARTESIAN_POINT('',(14.5,80.301666091711,112.852477851287));
#52307=CARTESIAN_POINT('',(14.,80.301666091711,112.852477851287));
#52308=CARTESIAN_POINT('',(14.5,80.13670067494,113.575345937994));
#52309=CARTESIAN_POINT('',(14.5,80.301666091711,112.852477851287));
#52310=CARTESIAN_POINT('',(14.,80.13670067494,113.575345937994));
#52311=CARTESIAN_POINT('Origin',(57.5,78.5818533282826,114.056703712549));
#52312=CARTESIAN_POINT('',(57.5,78.5818533282826,114.056703712549));
#52313=CARTESIAN_POINT('',(57.5,78.5818533282826,114.056703712549));
#52314=CARTESIAN_POINT('',(58.,78.9918455961111,113.766594799967));
#52315=CARTESIAN_POINT('Origin',(14.,79.8888272731288,113.138521468083));
#52316=CARTESIAN_POINT('',(14.,79.8888272731288,113.138521468083));
#52317=CARTESIAN_POINT('',(14.,79.8888272731288,113.138521468083));
#52318=CARTESIAN_POINT('',(14.5,80.13670067494,113.575345937994));
#52319=CARTESIAN_POINT('Origin',(14.25,78.882460664988,110.833403841184));
#52320=CARTESIAN_POINT('',(14.,78.6644207307221,110.955709143871));
#52321=CARTESIAN_POINT('',(14.5,79.100500599254,110.711098538497));
#52322=CARTESIAN_POINT('Origin',(14.5,78.5818533282826,114.056703712549));
#52323=CARTESIAN_POINT('',(14.,78.9918455961111,113.766594799967));
#52324=CARTESIAN_POINT('',(14.5,79.317548630651,114.148922374345));
#52325=CARTESIAN_POINT('',(14.,78.9918455961111,113.766594799967));
#52326=CARTESIAN_POINT('',(14.5,78.5818533282826,114.056703712549));
#52327=CARTESIAN_POINT('',(14.5,78.5818533282826,114.056703712549));
#52328=CARTESIAN_POINT('',(14.5,79.317548630651,114.148922374345));
#52329=CARTESIAN_POINT('Origin',(14.25,78.4809245051847,113.556111664665));
#52330=CARTESIAN_POINT('',(14.5,78.2914210651986,113.719171304777));
#52331=CARTESIAN_POINT('',(14.,78.6704279451708,113.393052024553));
#52332=CARTESIAN_POINT('Origin',(14.,78.9497009794668,114.102813043447));
#52333=CARTESIAN_POINT('',(14.,79.317548630651,114.148922374345));
#52334=CARTESIAN_POINT('',(14.,78.5818533282826,114.056703712549));
#52335=CARTESIAN_POINT('Origin',(14.25,79.9933065658522,113.370557926922));
#52336=CARTESIAN_POINT('',(14.5,80.13670067494,113.575345937994));
#52337=CARTESIAN_POINT('',(14.,79.8499124567644,113.16576991585));
#52338=CARTESIAN_POINT('Origin',(57.75,78.4809245051847,113.556111664665));
#52339=CARTESIAN_POINT('',(57.5,78.2914210651986,113.719171304777));
#52340=CARTESIAN_POINT('Origin',(14.,78.5796317693959,109.782518968122));
#52341=CARTESIAN_POINT('Origin',(14.,80.5462766970845,113.288557719819));
#52342=CARTESIAN_POINT('Origin',(57.5,69.9330127018923,120.127531126037));
#52343=CARTESIAN_POINT('',(57.5,70.1603524804536,119.421791454066));
#52344=CARTESIAN_POINT('',(58.,69.7241542943355,119.670765314673));
#52345=CARTESIAN_POINT('',(57.5,70.1603524804536,119.421791454066));
#52346=CARTESIAN_POINT('',(57.5,69.9330127018923,120.127531126037));
#52347=CARTESIAN_POINT('',(57.5,69.9330127018923,120.127531126037));
#52348=CARTESIAN_POINT('',(58.,69.7241542943355,119.670765314673));
#52349=CARTESIAN_POINT('Origin',(57.5,68.3421289244415,120.471543313576));
#52350=CARTESIAN_POINT('',(57.5,69.0669872981079,120.627531126037));
#52351=CARTESIAN_POINT('',(58.,68.7758457056646,120.218271533617));
#52352=CARTESIAN_POINT('',(57.5,69.0669872981079,120.627531126037));
#52353=CARTESIAN_POINT('',(57.5,68.3421289244415,120.471543313576));
#52354=CARTESIAN_POINT('',(57.5,68.3421289244415,120.471543313576));
#52355=CARTESIAN_POINT('',(58.,68.7758457056646,120.218271533617));
#52356=CARTESIAN_POINT('Origin',(14.,69.7241542943355,119.670765314673));
#52357=CARTESIAN_POINT('',(14.5,70.1603524804536,119.421791454066));
#52358=CARTESIAN_POINT('',(14.5,69.9330127018923,120.127531126037));
#52359=CARTESIAN_POINT('',(14.5,70.1603524804536,119.421791454066));
#52360=CARTESIAN_POINT('',(14.,69.7241542943355,119.670765314673));
#52361=CARTESIAN_POINT('',(14.,69.7241542943355,119.670765314673));
#52362=CARTESIAN_POINT('',(14.5,69.9330127018923,120.127531126037));
#52363=CARTESIAN_POINT('Origin',(14.25,68.9225214538622,117.286708727069));
#52364=CARTESIAN_POINT('',(14.,68.6946516178765,117.389545188734));
#52365=CARTESIAN_POINT('',(14.5,69.1503912898478,117.183872265403));
#52366=CARTESIAN_POINT('Origin',(14.5,68.3421289244415,120.471543313576));
#52367=CARTESIAN_POINT('',(14.,68.7758457056646,120.218271533617));
#52368=CARTESIAN_POINT('',(14.5,69.0669872981079,120.627531126037));
#52369=CARTESIAN_POINT('',(14.,68.7758457056646,120.218271533617));
#52370=CARTESIAN_POINT('',(14.5,68.3421289244415,120.471543313576));
#52371=CARTESIAN_POINT('',(14.5,68.3421289244415,120.471543313576));
#52372=CARTESIAN_POINT('',(14.5,69.0669872981079,120.627531126037));
#52373=CARTESIAN_POINT('Origin',(14.25,68.2852136377336,119.964059643026));
#52374=CARTESIAN_POINT('',(14.5,68.0822197315032,120.109982478913));
#52375=CARTESIAN_POINT('',(14.,68.488207543964,119.818136807139));
#52376=CARTESIAN_POINT('Origin',(14.,68.7045581112747,120.549537219807));
#52377=CARTESIAN_POINT('',(14.,69.0669872981079,120.627531126037));
#52378=CARTESIAN_POINT('',(14.,68.3421289244415,120.471543313576));
#52379=CARTESIAN_POINT('Origin',(14.25,69.8080127018923,119.911024775091));
#52380=CARTESIAN_POINT('',(14.5,69.9330127018923,120.127531126037));
#52381=CARTESIAN_POINT('',(14.,69.6830127018923,119.694518424145));
#52382=CARTESIAN_POINT('Origin',(14.,70.0466825911729,119.774661290051));
#52383=CARTESIAN_POINT('',(14.,70.1603524804536,119.421791454066));
#52384=CARTESIAN_POINT('',(14.,69.9330127018923,120.127531126037));
#52385=CARTESIAN_POINT('Origin',(57.75,68.2852136377336,119.964059643026));
#52386=CARTESIAN_POINT('',(58.,68.4882075439641,119.818136807139));
#52387=CARTESIAN_POINT('',(57.5,68.0822197315032,120.109982478913));
#52388=CARTESIAN_POINT('Origin',(57.75,69.8080127018923,119.911024775091));
#52389=CARTESIAN_POINT('',(58.,69.6830127018923,119.694518424145));
#52390=CARTESIAN_POINT('',(57.5,69.9330127018923,120.127531126037));
#52391=CARTESIAN_POINT('Origin',(57.75,68.9225214538622,117.286708727069));
#52392=CARTESIAN_POINT('',(57.5,69.1503912898478,117.183872265403));
#52393=CARTESIAN_POINT('',(58.,68.6946516178765,117.389545188734));
#52394=CARTESIAN_POINT('Origin',(14.,68.5000000000001,118.645480318468));
#52395=CARTESIAN_POINT('Origin',(14.,68.7124355652983,116.213429510899));
#52396=CARTESIAN_POINT('Origin',(14.,70.3660254037845,119.877531126037));
#52397=CARTESIAN_POINT('Origin',(57.5,57.5822796533798,125.969521727281));
#52398=CARTESIAN_POINT('',(57.5,58.290784488439,126.188091528965));
#52399=CARTESIAN_POINT('',(58.,58.0364201014071,125.755014631118));
#52400=CARTESIAN_POINT('',(57.5,58.290784488439,126.188091528965));
#52401=CARTESIAN_POINT('',(57.5,57.5822796533798,125.969521727281));
#52402=CARTESIAN_POINT('',(57.5,57.5822796533798,125.969521727281));
#52403=CARTESIAN_POINT('',(58.,58.0364201014071,125.755014631118));
#52404=CARTESIAN_POINT('Origin',(14.,57.9365320709094,126.078806628123));
#52405=CARTESIAN_POINT('',(14.2512407024475,57.9365320709094,126.078806628123));
#52406=CARTESIAN_POINT('',(14.5,57.5822796533798,125.969521727281));
#52407=CARTESIAN_POINT('',(14.3353834448874,57.816706318786,126.041841049933));
#52408=CARTESIAN_POINT('',(14.,57.5822796533798,125.969521727281));
#52409=CARTESIAN_POINT('',(14.5,58.290784488439,126.188091528965));
#52410=CARTESIAN_POINT('',(14.,58.290784488439,126.188091528965));
#52411=CARTESIAN_POINT('',(14.4305329766294,58.1918580916782,126.157573285685));
#52412=CARTESIAN_POINT('Origin',(57.75,57.5698110627601,125.459008691224));
#52413=CARTESIAN_POINT('',(58.,57.7847505290374,125.331333220453));
#52414=CARTESIAN_POINT('',(57.5,57.3548715964829,125.586684161994));
#52415=CARTESIAN_POINT('Origin',(57.5,59.1970922754756,125.765473267224));
#52416=CARTESIAN_POINT('',(57.5,59.4850762228409,125.08223311503));
#52417=CARTESIAN_POINT('',(58.,59.0288384007668,125.292242378034));
#52418=CARTESIAN_POINT('',(57.5,59.4850762228409,125.08223311503));
#52419=CARTESIAN_POINT('',(57.5,59.1970922754756,125.765473267224));
#52420=CARTESIAN_POINT('',(57.5,59.1970922754756,125.765473267224));
#52421=CARTESIAN_POINT('',(58.,59.0288384007668,125.292242378034));
#52422=CARTESIAN_POINT('Origin',(14.,59.3410842491583,125.423853191127));
#52423=CARTESIAN_POINT('',(14.2512407024475,59.3410842491583,125.423853191127));
#52424=CARTESIAN_POINT('',(14.5,59.1970922754756,125.765473267224));
#52425=CARTESIAN_POINT('',(14.2590041943422,59.3365904250818,125.434514761239));
#52426=CARTESIAN_POINT('',(14.,59.1970922754756,125.765473267224));
#52427=CARTESIAN_POINT('',(14.5,59.4850762228409,125.08223311503));
#52428=CARTESIAN_POINT('',(14.,59.4850762228409,125.08223311503));
#52429=CARTESIAN_POINT('',(14.6801520303733,59.5893555268573,124.83483110461));
#52430=CARTESIAN_POINT('Origin',(57.75,59.0914377100405,125.538896320465));
#52431=CARTESIAN_POINT('',(58.,58.9857831446053,125.312319373706));
#52432=CARTESIAN_POINT('',(57.5,59.1970922754756,125.765473267224));
#52433=CARTESIAN_POINT('Origin',(57.75,58.4380402379162,122.84739093989));
#52434=CARTESIAN_POINT('',(57.5,58.6740057485781,122.764805966813));
#52435=CARTESIAN_POINT('',(58.,58.2020747272542,122.929975912966));
#52436=CARTESIAN_POINT('Origin',(14.25,57.5698110627601,125.459008691224));
#52437=CARTESIAN_POINT('',(14.,58.0364201014071,125.755014631118));
#52438=CARTESIAN_POINT('',(14.5,57.8376305949207,126.399400659835));
#52439=CARTESIAN_POINT('',(14.,57.7847505290374,125.331333220453));
#52440=CARTESIAN_POINT('',(14.5,57.3548715964829,125.586684161994));
#52441=CARTESIAN_POINT('Origin',(14.,59.650246168994,125.554164136354));
#52442=CARTESIAN_POINT('',(14.5,59.1970922754756,125.765473267224));
#52443=CARTESIAN_POINT('Origin',(14.25,59.0914377100405,125.538896320465));
#52444=CARTESIAN_POINT('',(14.,59.0288384007668,125.292242378034));
#52445=CARTESIAN_POINT('',(14.,59.0288384007668,125.292242378034));
#52446=CARTESIAN_POINT('',(14.,58.9857831446053,125.312319373706));
#52447=CARTESIAN_POINT('Origin',(14.25,58.4380402379162,122.84739093989));
#52448=CARTESIAN_POINT('',(14.5,58.6740057485781,122.764805966813));
#52449=CARTESIAN_POINT('',(14.,58.2020747272542,122.929975912966));
#52450=CARTESIAN_POINT('Origin',(14.,58.3222962368458,121.759885683511));
#52451=CARTESIAN_POINT('Origin',(14.,57.8376305949207,126.399400659835));
#52452=CARTESIAN_POINT('Origin',(57.5,48.010646232661,130.446264217578));
#52453=CARTESIAN_POINT('',(57.5,48.3570826171014,129.790723455271));
#52454=CARTESIAN_POINT('',(58.,47.8842774043812,129.960169823373));
#52455=CARTESIAN_POINT('',(57.5,48.3570826171014,129.790723455271));
#52456=CARTESIAN_POINT('',(57.5,48.010646232661,130.446264217578));
#52457=CARTESIAN_POINT('',(57.5,48.010646232661,130.446264217578));
#52458=CARTESIAN_POINT('',(58.,47.8842774043812,129.960169823373));
#52459=CARTESIAN_POINT('Origin',(57.5,46.3841944650248,130.508796018163));
#52460=CARTESIAN_POINT('',(57.5,47.0709536118751,130.788284360904));
#52461=CARTESIAN_POINT('',(58.,46.8553022968292,130.334686134323));
#52462=CARTESIAN_POINT('',(57.5,47.0709536118751,130.788284360904));
#52463=CARTESIAN_POINT('',(57.5,46.3841944650248,130.508796018163));
#52464=CARTESIAN_POINT('',(57.5,46.3841944650248,130.508796018163));
#52465=CARTESIAN_POINT('',(58.,46.8553022968292,130.334686134323));
#52466=CARTESIAN_POINT('Origin',(14.,47.8842774043813,129.960169823373));
#52467=CARTESIAN_POINT('',(14.5,48.3570826171014,129.790723455271));
#52468=CARTESIAN_POINT('',(14.5,48.010646232661,130.446264217578));
#52469=CARTESIAN_POINT('',(14.5,48.3570826171014,129.790723455271));
#52470=CARTESIAN_POINT('',(14.,47.8842774043813,129.960169823373));
#52471=CARTESIAN_POINT('',(14.,47.8842774043813,129.960169823373));
#52472=CARTESIAN_POINT('',(14.5,48.010646232661,130.446264217578));
#52473=CARTESIAN_POINT('Origin',(14.25,47.5088102499062,127.473130330375));
#52474=CARTESIAN_POINT('',(14.,47.266544904584,127.534835293351));
#52475=CARTESIAN_POINT('',(14.5,47.7510755952284,127.411425367399));
#52476=CARTESIAN_POINT('Origin',(14.5,46.3841944650248,130.508796018163));
#52477=CARTESIAN_POINT('',(14.,46.8553022968292,130.334686134323));
#52478=CARTESIAN_POINT('',(14.5,47.0709536118751,130.788284360904));
#52479=CARTESIAN_POINT('',(14.,46.8553022968292,130.334686134323));
#52480=CARTESIAN_POINT('',(14.5,46.3841944650248,130.508796018163));
#52481=CARTESIAN_POINT('',(14.5,46.3841944650248,130.508796018163));
#52482=CARTESIAN_POINT('',(14.5,47.0709536118751,130.788284360904));
#52483=CARTESIAN_POINT('Origin',(14.25,46.4162674639967,129.99913892906));
#52484=CARTESIAN_POINT('',(14.5,46.191018256795,130.107595347289));
#52485=CARTESIAN_POINT('',(14.,46.6415166711984,129.890682510832));
#52486=CARTESIAN_POINT('Origin',(14.,46.7275740384499,130.648540189534));
#52487=CARTESIAN_POINT('',(14.,47.0709536118751,130.788284360904));
#52488=CARTESIAN_POINT('',(14.,46.3841944650248,130.508796018163));
#52489=CARTESIAN_POINT('Origin',(14.25,47.9251411968296,130.211341062382));
#52490=CARTESIAN_POINT('',(14.5,48.010646232661,130.446264217578));
#52491=CARTESIAN_POINT('',(14.,47.8396361609982,129.976417907185));
#52492=CARTESIAN_POINT('Origin',(14.,48.1838644248812,130.118493836425));
#52493=CARTESIAN_POINT('',(14.,48.3570826171014,129.790723455271));
#52494=CARTESIAN_POINT('',(14.,48.010646232661,130.446264217578));
#52495=CARTESIAN_POINT('Origin',(57.75,46.4162674639967,129.99913892906));
#52496=CARTESIAN_POINT('',(58.,46.6415166711984,129.890682510832));
#52497=CARTESIAN_POINT('',(57.5,46.191018256795,130.107595347289));
#52498=CARTESIAN_POINT('Origin',(57.75,47.9251411968296,130.211341062382));
#52499=CARTESIAN_POINT('',(58.,47.8396361609982,129.976417907185));
#52500=CARTESIAN_POINT('',(57.5,48.010646232661,130.446264217578));
#52501=CARTESIAN_POINT('Origin',(57.75,47.5088102499062,127.473130330375));
#52502=CARTESIAN_POINT('',(57.5,47.7510755952284,127.411425367399));
#52503=CARTESIAN_POINT('',(58.,47.266544904584,127.534835293351));
#52504=CARTESIAN_POINT('Origin',(14.,46.8567596356167,128.737889047669));
#52505=CARTESIAN_POINT('Origin',(14.,47.4882890180657,126.379675605442));
#52506=CARTESIAN_POINT('Origin',(14.,48.480492543054,130.275254145916));
#52507=CARTESIAN_POINT('Origin',(57.5,36.4588101823949,134.134280331629));
#52508=CARTESIAN_POINT('',(57.5,36.8610624138407,133.511428020236));
#52509=CARTESIAN_POINT('',(58.,36.375288143631,133.639021904261));
#52510=CARTESIAN_POINT('',(57.5,36.8610624138407,133.511428020236));
#52511=CARTESIAN_POINT('',(57.5,36.4588101823949,134.134280331629));
#52512=CARTESIAN_POINT('',(57.5,36.4588101823949,134.134280331629));
#52513=CARTESIAN_POINT('',(58.,36.375288143631,133.639021904261));
#52514=CARTESIAN_POINT('Origin',(57.5,34.8330975492484,134.054819567983));
#52515=CARTESIAN_POINT('',(57.5,35.4928843561058,134.393099376732));
#52516=CARTESIAN_POINT('',(58.,35.3175873497673,133.922431977811));
#52517=CARTESIAN_POINT('',(57.5,35.4928843561058,134.393099376732));
#52518=CARTESIAN_POINT('',(57.5,34.8330975492484,134.054819567983));
#52519=CARTESIAN_POINT('',(57.5,34.8330975492484,134.054819567983));
#52520=CARTESIAN_POINT('',(58.,35.3175873497673,133.922431977811));
#52521=CARTESIAN_POINT('Origin',(14.,36.375288143631,133.639021904261));
#52522=CARTESIAN_POINT('',(14.5,36.8610624138407,133.511428020236));
#52523=CARTESIAN_POINT('',(14.5,36.4588101823949,134.134280331629));
#52524=CARTESIAN_POINT('',(14.5,36.8610624138407,133.511428020236));
#52525=CARTESIAN_POINT('',(14.,36.375288143631,133.639021904261));
#52526=CARTESIAN_POINT('',(14.,36.375288143631,133.639021904261));
#52527=CARTESIAN_POINT('',(14.5,36.4588101823949,134.134280331629));
#52528=CARTESIAN_POINT('Origin',(14.25,36.2180095292903,131.128722228666));
#52529=CARTESIAN_POINT('',(14.,35.9712881348695,131.169077569515));
#52530=CARTESIAN_POINT('',(14.5,36.4647309237111,131.088366887817));
#52531=CARTESIAN_POINT('Origin',(14.5,34.8330975492484,134.054819567983));
#52532=CARTESIAN_POINT('',(14.,35.3175873497673,133.922431977811));
#52533=CARTESIAN_POINT('',(14.5,35.4928843561058,134.393099376732));
#52534=CARTESIAN_POINT('',(14.,35.3175873497673,133.922431977811));
#52535=CARTESIAN_POINT('',(14.5,34.8330975492484,134.054819567983));
#52536=CARTESIAN_POINT('',(14.5,34.8330975492484,134.054819567983));
#52537=CARTESIAN_POINT('',(14.5,35.4928843561058,134.393099376732));
#52538=CARTESIAN_POINT('Origin',(14.25,34.9094680429235,133.549897224021));
#52539=CARTESIAN_POINT('',(14.5,34.6756233772733,133.638309170877));
#52540=CARTESIAN_POINT('',(14.,35.1433127085737,133.461485277164));
#52541=CARTESIAN_POINT('Origin',(14.,35.1629909526771,134.223959472357));
#52542=CARTESIAN_POINT('',(14.,35.4928843561058,134.393099376732));
#52543=CARTESIAN_POINT('',(14.,34.8330975492484,134.054819567983));
#52544=CARTESIAN_POINT('Origin',(14.25,36.3941054211193,133.892798875057));
#52545=CARTESIAN_POINT('',(14.5,36.4588101823949,134.134280331629));
#52546=CARTESIAN_POINT('',(14.,36.3294006598436,133.651317418485));
#52547=CARTESIAN_POINT('Origin',(14.,36.6599362981178,133.822854175933));
#52548=CARTESIAN_POINT('',(14.,36.8610624138407,133.511428020236));
#52549=CARTESIAN_POINT('',(14.,36.4588101823949,134.134280331629));
#52550=CARTESIAN_POINT('Origin',(57.75,34.9094680429235,133.549897224021));
#52551=CARTESIAN_POINT('',(58.,35.1433127085737,133.461485277164));
#52552=CARTESIAN_POINT('',(57.5,34.6756233772733,133.638309170877));
#52553=CARTESIAN_POINT('Origin',(57.75,36.3941054211193,133.892798875057));
#52554=CARTESIAN_POINT('',(58.,36.3294006598436,133.651317418485));
#52555=CARTESIAN_POINT('',(57.5,36.4588101823949,134.134280331629));
#52556=CARTESIAN_POINT('Origin',(57.75,36.2180095292903,131.128722228666));
#52557=CARTESIAN_POINT('',(57.5,36.4647309237111,131.088366887817));
#52558=CARTESIAN_POINT('',(58.,35.9712881348695,131.169077569515));
#52559=CARTESIAN_POINT('Origin',(14.,35.4582091790453,132.331838201602));
#52560=CARTESIAN_POINT('Origin',(14.,36.292867245645,130.037639885881));
#52561=CARTESIAN_POINT('Origin',(14.,36.9417730955394,134.004870809078));
#52562=CARTESIAN_POINT('Origin',(1.88275881709439,0.,-3.89963199725568E-15));
#52563=CARTESIAN_POINT('',(1.46551763418878,127.371647073124,-1.55985279890227E-14));
#52564=CARTESIAN_POINT('',(1.46551763418879,-127.371647073124,-1.55985279890227E-14));
#52565=CARTESIAN_POINT('Origin',(1.46551763418878,0.,-7.79926399451136E-15));
#52566=CARTESIAN_POINT('Origin',(1.46551763418878,0.,-7.79926399451136E-15));
#52567=CARTESIAN_POINT('',(2.3,127.,1.55530143491714E-14));
#52568=CARTESIAN_POINT('',(1.88275881709439,127.185823536562,-1.5575771169097E-14));
#52569=CARTESIAN_POINT('',(2.3,-127.,-1.55530143491714E-14));
#52570=CARTESIAN_POINT('Origin',(2.3,0.,0.));
#52571=CARTESIAN_POINT('Origin',(2.3,0.,0.));
#52572=CARTESIAN_POINT('Origin',(0.9,0.,0.));
#52573=CARTESIAN_POINT('',(0.334482365811226,-128.628352926876,-1.57524300691495E-14));
#52574=CARTESIAN_POINT('',(0.9,-128.,-1.56754790290861E-14));
#52575=CARTESIAN_POINT('',(0.334482365811233,128.628352926876,1.57524300691495E-14));
#52576=CARTESIAN_POINT('Origin',(0.334482365811233,0.,-7.87621503457476E-15));
#52577=CARTESIAN_POINT('Origin',(0.334482365811233,0.,-7.87621503457476E-15));
#52578=CARTESIAN_POINT('Origin',(30.775,0.,0.));
#52579=CARTESIAN_POINT('',(59.75,-127.,-1.55530143491714E-14));
#52580=CARTESIAN_POINT('Origin',(59.75,0.,0.));
#52581=CARTESIAN_POINT('',(30.775,-127.,-1.55530143491714E-14));
#52582=CARTESIAN_POINT('Origin',(57.5,24.6295005722094,136.801453579863));
#52583=CARTESIAN_POINT('',(57.5,25.0845072682929,136.216030001563));
#52584=CARTESIAN_POINT('',(58.,24.5894609761083,136.30080033501));
#52585=CARTESIAN_POINT('',(57.5,25.0845072682929,136.216030001563));
#52586=CARTESIAN_POINT('',(57.5,24.6295005722094,136.801453579863));
#52587=CARTESIAN_POINT('',(57.5,24.6295005722094,136.801453579863));
#52588=CARTESIAN_POINT('',(58.,24.5894609761083,136.30080033501));
#52589=CARTESIAN_POINT('Origin',(57.5,23.016899728323,136.580604996376));
#52590=CARTESIAN_POINT('',(57.5,23.6446928191972,136.97510175753));
#52591=CARTESIAN_POINT('',(58.,23.5110842376315,136.490947249372));
#52592=CARTESIAN_POINT('',(57.5,23.6446928191972,136.97510175753));
#52593=CARTESIAN_POINT('',(57.5,23.016899728323,136.580604996376));
#52594=CARTESIAN_POINT('',(57.5,23.016899728323,136.580604996376));
#52595=CARTESIAN_POINT('',(58.,23.5110842376315,136.490947249372));
#52596=CARTESIAN_POINT('Origin',(14.,24.5894609761083,136.30080033501));
#52597=CARTESIAN_POINT('',(14.5,25.0845072682929,136.216030001563));
#52598=CARTESIAN_POINT('',(14.5,24.6295005722094,136.801453579863));
#52599=CARTESIAN_POINT('',(14.5,25.0845072682929,136.216030001563));
#52600=CARTESIAN_POINT('',(14.,24.5894609761083,136.30080033501));
#52601=CARTESIAN_POINT('',(14.,24.5894609761083,136.30080033501));
#52602=CARTESIAN_POINT('',(14.5,24.6295005722094,136.801453579863));
#52603=CARTESIAN_POINT('Origin',(14.25,24.6515678871246,133.786345373109));
#52604=CARTESIAN_POINT('',(14.,24.4022681423913,133.805043963321));
#52605=CARTESIAN_POINT('',(14.5,24.900867631858,133.767646782898));
#52606=CARTESIAN_POINT('Origin',(14.5,23.016899728323,136.580604996376));
#52607=CARTESIAN_POINT('',(14.,23.5110842376315,136.490947249372));
#52608=CARTESIAN_POINT('',(14.5,23.6446928191972,136.97510175753));
#52609=CARTESIAN_POINT('',(14.,23.5110842376315,136.490947249372));
#52610=CARTESIAN_POINT('',(14.5,23.016899728323,136.580604996376));
#52611=CARTESIAN_POINT('',(14.5,23.016899728323,136.580604996376));
#52612=CARTESIAN_POINT('',(14.5,23.6446928191972,136.97510175753));
#52613=CARTESIAN_POINT('Origin',(14.25,23.1369864911307,136.084260161474));
#52614=CARTESIAN_POINT('',(14.5,22.8963260661369,136.151954768658));
#52615=CARTESIAN_POINT('',(14.,23.3776469161245,136.01656555429));
#52616=CARTESIAN_POINT('Origin',(14.,23.3307962737601,136.777853376953));
#52617=CARTESIAN_POINT('',(14.,23.6446928191972,136.97510175753));
#52618=CARTESIAN_POINT('',(14.,23.016899728323,136.580604996376));
#52619=CARTESIAN_POINT('Origin',(14.25,24.5860885277927,136.55525164161));
#52620=CARTESIAN_POINT('',(14.5,24.6295005722094,136.801453579863));
#52621=CARTESIAN_POINT('',(14.,24.542676483376,136.309049703357));
#52622=CARTESIAN_POINT('Origin',(14.,24.8570039202511,136.508741790713));
#52623=CARTESIAN_POINT('',(14.,25.0845072682929,136.216030001563));
#52624=CARTESIAN_POINT('',(14.,24.6295005722094,136.801453579863));
#52625=CARTESIAN_POINT('Origin',(57.75,23.1369864911307,136.084260161474));
#52626=CARTESIAN_POINT('',(58.,23.3776469161245,136.01656555429));
#52627=CARTESIAN_POINT('',(57.5,22.8963260661369,136.151954768658));
#52628=CARTESIAN_POINT('Origin',(57.75,24.5860885277927,136.55525164161));
#52629=CARTESIAN_POINT('',(58.,24.542676483376,136.309049703357));
#52630=CARTESIAN_POINT('',(57.5,24.6295005722094,136.801453579863));
#52631=CARTESIAN_POINT('Origin',(57.75,24.6515678871246,133.786345373109));
#52632=CARTESIAN_POINT('',(57.5,24.900867631858,133.767646782898));
#52633=CARTESIAN_POINT('',(58.,24.4022681423913,133.805043963321));
#52634=CARTESIAN_POINT('Origin',(14.,23.7898003403695,134.918662162673));
#52635=CARTESIAN_POINT('Origin',(14.,24.8212348392527,132.705939207914));
#52636=CARTESIAN_POINT('Origin',(14.,25.1219044487155,136.71462949103));
#52637=CARTESIAN_POINT('Origin',(57.5,12.6127455909704,138.427485163379));
#52638=CARTESIAN_POINT('',(57.5,13.1170438759937,137.883945745091));
#52639=CARTESIAN_POINT('',(58.,12.6164931630349,137.925247374536));
#52640=CARTESIAN_POINT('',(57.5,13.1170438759937,137.883945745091));
#52641=CARTESIAN_POINT('',(57.5,12.6127455909704,138.427485163379));
#52642=CARTESIAN_POINT('',(57.5,12.6127455909704,138.427485163379));
#52643=CARTESIAN_POINT('',(58.,12.6164931630349,137.925247374536));
#52644=CARTESIAN_POINT('Origin',(57.5,11.025529402481,138.066929551123));
#52645=CARTESIAN_POINT('',(57.5,11.6165508928786,138.514640906126));
#52646=CARTESIAN_POINT('',(58.,11.5256475780665,138.020683996878));
#52647=CARTESIAN_POINT('',(57.5,11.6165508928786,138.514640906126));
#52648=CARTESIAN_POINT('',(57.5,11.0255294024811,138.066929551123));
#52649=CARTESIAN_POINT('',(57.5,11.025529402481,138.066929551123));
#52650=CARTESIAN_POINT('',(58.,11.5256475780665,138.020683996878));
#52651=CARTESIAN_POINT('Origin',(14.,12.6164931630349,137.925247374536));
#52652=CARTESIAN_POINT('',(14.5,13.1170438759937,137.883945745091));
#52653=CARTESIAN_POINT('',(14.5,12.6127455909704,138.427485163379));
#52654=CARTESIAN_POINT('',(14.5,13.1170438759937,137.883945745091));
#52655=CARTESIAN_POINT('',(14.,12.6164931630349,137.925247374536));
#52656=CARTESIAN_POINT('',(14.,12.6164931630349,137.925247374536));
#52657=CARTESIAN_POINT('',(14.5,12.6127455909704,138.427485163379));
#52658=CARTESIAN_POINT('Origin',(14.25,12.8975129283142,135.425773646859));
#52659=CARTESIAN_POINT('',(14.,12.647532154857,135.422673178871));
#52660=CARTESIAN_POINT('',(14.5,13.1474937017714,135.428874114848));
#52661=CARTESIAN_POINT('Origin',(14.5,11.0255294024811,138.066929551123));
#52662=CARTESIAN_POINT('',(14.,11.5256475780664,138.020683996878));
#52663=CARTESIAN_POINT('',(14.5,11.6165508928786,138.514640906126));
#52664=CARTESIAN_POINT('',(14.,11.5256475780664,138.020683996878));
#52665=CARTESIAN_POINT('',(14.5,11.025529402481,138.066929551123));
#52666=CARTESIAN_POINT('',(14.5,11.0255294024811,138.066929551123));
#52667=CARTESIAN_POINT('',(14.5,11.6165508928786,138.514640906126));
#52668=CARTESIAN_POINT('Origin',(14.25,11.188418501646,137.582939709175));
#52669=CARTESIAN_POINT('',(14.5,10.9427738884575,137.629401779851));
#52670=CARTESIAN_POINT('',(14.,11.4340631148345,137.536477638499));
#52671=CARTESIAN_POINT('Origin',(14.,11.3210401476798,138.290785228625));
#52672=CARTESIAN_POINT('',(14.,11.6165508928786,138.514640906126));
#52673=CARTESIAN_POINT('',(14.,11.025529402481,138.066929551123));
#52674=CARTESIAN_POINT('Origin',(14.25,12.5909566552835,138.178436488856));
#52675=CARTESIAN_POINT('',(14.5,12.6127455909704,138.427485163379));
#52676=CARTESIAN_POINT('',(14.,12.5691677195965,137.929387814333));
#52677=CARTESIAN_POINT('Origin',(14.,12.864894733482,138.155715454235));
#52678=CARTESIAN_POINT('',(14.,13.1170438759937,137.883945745091));
#52679=CARTESIAN_POINT('',(14.,12.6127455909704,138.427485163379));
#52680=CARTESIAN_POINT('Origin',(57.75,11.188418501646,137.582939709175));
#52681=CARTESIAN_POINT('',(58.,11.4340631148345,137.536477638499));
#52682=CARTESIAN_POINT('',(57.5,10.9427738884575,137.629401779851));
#52683=CARTESIAN_POINT('Origin',(57.75,12.5909566552835,138.178436488856));
#52684=CARTESIAN_POINT('',(58.,12.5691677195965,137.929387814333));
#52685=CARTESIAN_POINT('',(57.5,12.6127455909704,138.427485163379));
#52686=CARTESIAN_POINT('Origin',(57.75,12.8975129283142,135.425773646859));
#52687=CARTESIAN_POINT('',(57.5,13.1474937017714,135.428874114848));
#52688=CARTESIAN_POINT('',(58.,12.647532154857,135.422673178871));
#52689=CARTESIAN_POINT('Origin',(14.,11.9403367564292,136.478673638569));
#52690=CARTESIAN_POINT('Origin',(14.,13.1606978482623,134.364266202539));
#52691=CARTESIAN_POINT('Origin',(14.,13.1108429400163,138.383907292005));
#52692=CARTESIAN_POINT('Origin',(11.2910997468263,0.,-4.24054782501806E-15));
#52693=CARTESIAN_POINT('',(11.5821994936527,138.506803038084,-1.69621913000722E-14));
#52694=CARTESIAN_POINT('',(11.5821994936527,-138.506803038084,-1.69621913000722E-14));
#52695=CARTESIAN_POINT('Origin',(11.5821994936527,0.,-8.48109565003612E-15));
#52696=CARTESIAN_POINT('Origin',(11.5821994936527,0.,-8.48109565003612E-15));
#52697=CARTESIAN_POINT('',(11.,139.,1.70225905081482E-14));
#52698=CARTESIAN_POINT('',(11.2910997468263,138.753401519042,1.69923909041102E-14));
#52699=CARTESIAN_POINT('',(11.,-139.,-1.70225905081482E-14));
#52700=CARTESIAN_POINT('Origin',(11.,0.,0.));
#52701=CARTESIAN_POINT('Origin',(11.,0.,0.));
#52702=CARTESIAN_POINT('Origin',(5.75,0.,0.));
#52703=CARTESIAN_POINT('',(1.5,-139.,-1.70225905081482E-14));
#52704=CARTESIAN_POINT('',(5.75,-139.,-1.70225905081482E-14));
#52705=CARTESIAN_POINT('',(1.5,139.,-1.70225905081482E-14));
#52706=CARTESIAN_POINT('Origin',(1.5,0.,0.));
#52707=CARTESIAN_POINT('Origin',(1.5,0.,0.));
#52708=CARTESIAN_POINT('Origin',(11.75,0.,0.));
#52709=CARTESIAN_POINT('',(11.75,-137.5,-1.68388934882761E-14));
#52710=CARTESIAN_POINT('Origin',(0.167241182905616,0.,-3.93810751728738E-15));
#52711=CARTESIAN_POINT('',(0.,129.5,-1.58591760489582E-14));
#52712=CARTESIAN_POINT('Origin',(0.,0.,0.));
#52713=CARTESIAN_POINT('',(0.167241182905616,129.064176463438,-1.58058030590539E-14));
#52714=CARTESIAN_POINT('Origin',(0.,139.,0.));
#52715=CARTESIAN_POINT('',(0.,137.5,1.68388934882761E-14));
#52716=CARTESIAN_POINT('Origin',(0.,0.,0.));
#52717=CARTESIAN_POINT('Origin',(1.07322330470336,0.,4.24482317633411E-15));
#52718=CARTESIAN_POINT('',(0.646446609406718,138.646446609407,3.39585854106729E-14));
#52719=CARTESIAN_POINT('Origin',(0.646446609406718,0.,8.48964635266822E-15));
#52720=CARTESIAN_POINT('',(1.07322330470336,138.823223304703,-8.51129525407411E-15));
#52721=CARTESIAN_POINT('Origin',(0.5,0.,0.));
#52722=CARTESIAN_POINT('',(0.353553390593267,138.353553390593,0.));
#52723=CARTESIAN_POINT('',(0.5,138.5,1.69613581681908E-14));
#52724=CARTESIAN_POINT('Origin',(0.353553390593267,0.,8.47171181552262E-15));
#52725=CARTESIAN_POINT('Origin',(0.176776695296634,0.,4.23585590776131E-15));
#52726=CARTESIAN_POINT('',(0.176776695296634,137.926776695297,2.53628703751833E-14));
#52727=CARTESIAN_POINT('Origin',(14.,11.1184535438328,138.5582187775));
#52728=CARTESIAN_POINT('Origin',(58.,11.9403367564292,136.478673638569));
#52729=CARTESIAN_POINT('Origin',(14.,23.1522889426911,137.061925846364));
#52730=CARTESIAN_POINT('Origin',(58.,23.7898003403695,134.918662162673));
#52731=CARTESIAN_POINT('Origin',(14.,35.0099214429613,134.522508899283));
#52732=CARTESIAN_POINT('Origin',(58.,35.4582091790453,132.331838201602));
#52733=CARTESIAN_POINT('Origin',(14.,46.6011073014821,130.959294432567));
#52734=CARTESIAN_POINT('Origin',(58.,46.8567596356167,128.737889047669));
#52735=CARTESIAN_POINT('Origin',(14.,57.8987018584759,124.164166824021));
#52736=CARTESIAN_POINT('Origin',(58.,57.8987018584759,124.164166824021));
#52737=CARTESIAN_POINT('Origin',(14.,68.6339745962156,120.877531126037));
#52738=CARTESIAN_POINT('Origin',(58.,68.5000000000001,118.645480318468));
#52739=CARTESIAN_POINT('Origin',(14.,78.5799717800934,112.223830067592));
#52740=CARTESIAN_POINT('Origin',(14.,78.9079726085065,114.435710592521));
#52741=CARTESIAN_POINT('Origin',(14.,88.58143330331,107.122965203224));
#52742=CARTESIAN_POINT('Origin',(58.,88.0619025270559,104.9480887073));
#52743=CARTESIAN_POINT('Origin',(14.,97.5807358037436,98.9949493661166));
#52744=CARTESIAN_POINT('Origin',(58.,96.873629022557,96.873629022557));
#52745=CARTESIAN_POINT('Origin',(14.,104.9480887073,88.0619025270559));
#52746=CARTESIAN_POINT('Origin',(58.,104.9480887073,88.0619025270559));
#52747=CARTESIAN_POINT('Origin',(14.,113.288557719819,80.5462766970844));
#52748=CARTESIAN_POINT('Origin',(58.,112.223830067592,78.5799717800933));
#52749=CARTESIAN_POINT('Origin',(14.,118.645480318468,68.5));
#52750=CARTESIAN_POINT('Origin',(14.,119.877531126037,70.3660254037845));
#52751=CARTESIAN_POINT('Origin',(14.,125.554164136354,59.6502461689938));
#52752=CARTESIAN_POINT('Origin',(58.,124.164166824021,57.8987018584757));
#52753=CARTESIAN_POINT('Origin',(14.,130.275254145916,48.4804925430538));
#52754=CARTESIAN_POINT('Origin',(58.,128.737889047669,46.8567596356165));
#52755=CARTESIAN_POINT('Origin',(14.,132.331838201602,35.4582091790453));
#52756=CARTESIAN_POINT('Origin',(58.,132.331838201602,35.4582091790453));
#52757=CARTESIAN_POINT('Origin',(14.,136.71462949103,25.1219044487155));
#52758=CARTESIAN_POINT('Origin',(58.,134.918662162673,23.7898003403694));
#52759=CARTESIAN_POINT('Origin',(14.,136.478673638569,11.9403367564291));
#52760=CARTESIAN_POINT('Origin',(14.,138.383907292005,13.1108429400162));
#52761=CARTESIAN_POINT('Origin',(14.,139.,0.999999999999974));
#52762=CARTESIAN_POINT('Origin',(58.,137.,-2.51664917224781E-14));
#52763=CARTESIAN_POINT('Origin',(14.,138.5582187775,-11.1184535438328));
#52764=CARTESIAN_POINT('Origin',(58.,136.478673638569,-11.9403367564292));
#52765=CARTESIAN_POINT('Origin',(14.,134.918662162673,-23.7898003403695));
#52766=CARTESIAN_POINT('Origin',(58.,134.918662162673,-23.7898003403695));
#52767=CARTESIAN_POINT('Origin',(14.,134.522508899283,-35.0099214429613));
#52768=CARTESIAN_POINT('Origin',(58.,132.331838201602,-35.4582091790453));
#52769=CARTESIAN_POINT('Origin',(14.,128.737889047669,-46.8567596356167));
#52770=CARTESIAN_POINT('Origin',(14.,130.959294432567,-46.6011073014821));
#52771=CARTESIAN_POINT('Origin',(14.,126.399400659835,-57.8376305949206));
#52772=CARTESIAN_POINT('Origin',(58.,124.164166824021,-57.8987018584759));
#52773=CARTESIAN_POINT('Origin',(14.,120.877531126037,-68.6339745962156));
#52774=CARTESIAN_POINT('Origin',(58.,118.645480318468,-68.5000000000001));
#52775=CARTESIAN_POINT('Origin',(14.,112.223830067592,-78.5799717800934));
#52776=CARTESIAN_POINT('Origin',(58.,112.223830067592,-78.5799717800934));
#52777=CARTESIAN_POINT('Origin',(14.,107.122965203224,-88.58143330331));
#52778=CARTESIAN_POINT('Origin',(58.,104.9480887073,-88.0619025270559));
#52779=CARTESIAN_POINT('Origin',(14.,96.873629022557,-96.873629022557));
#52780=CARTESIAN_POINT('Origin',(14.,98.9949493661167,-97.5807358037436));
#52781=CARTESIAN_POINT('Origin',(14.,90.113522189548,-105.837389983851));
#52782=CARTESIAN_POINT('Origin',(58.,88.0619025270559,-104.9480887073));
#52783=CARTESIAN_POINT('Origin',(14.,80.5462766970844,-113.288557719819));
#52784=CARTESIAN_POINT('Origin',(58.,78.5799717800933,-112.223830067592));
#52785=CARTESIAN_POINT('Origin',(14.,68.5,-118.645480318468));
#52786=CARTESIAN_POINT('Origin',(58.,68.5,-118.645480318468));
#52787=CARTESIAN_POINT('Origin',(14.,59.6502461689939,-125.554164136354));
#52788=CARTESIAN_POINT('Origin',(58.,57.8987018584758,-124.164166824021));
#52789=CARTESIAN_POINT('Origin',(14.,46.8567596356166,-128.737889047669));
#52790=CARTESIAN_POINT('Origin',(14.,48.4804925430539,-130.275254145916));
#52791=CARTESIAN_POINT('Origin',(14.,36.9417730955395,-134.004870809078));
#52792=CARTESIAN_POINT('Origin',(58.,35.4582091790453,-132.331838201602));
#52793=CARTESIAN_POINT('Origin',(14.,25.1219044487155,-136.71462949103));
#52794=CARTESIAN_POINT('Origin',(58.,23.7898003403694,-134.918662162673));
#52795=CARTESIAN_POINT('Origin',(14.,11.9403367564291,-136.478673638569));
#52796=CARTESIAN_POINT('Origin',(58.,11.9403367564291,-136.478673638569));
#52797=CARTESIAN_POINT('Origin',(14.,0.999999999999983,-139.));
#52798=CARTESIAN_POINT('Origin',(58.,-1.67776611483187E-14,-137.));
#52799=CARTESIAN_POINT('Origin',(14.,-11.9403367564292,-136.478673638569));
#52800=CARTESIAN_POINT('Origin',(14.,-11.1184535438327,-138.5582187775));
#52801=CARTESIAN_POINT('Origin',(14.,-23.1522889426912,-137.061925846364));
#52802=CARTESIAN_POINT('Origin',(58.,-23.7898003403695,-134.918662162672));
#52803=CARTESIAN_POINT('Origin',(14.,-35.0099214429614,-134.522508899283));
#52804=CARTESIAN_POINT('Origin',(58.,-35.4582091790454,-132.331838201602));
#52805=CARTESIAN_POINT('Origin',(14.,-46.8567596356166,-128.737889047669));
#52806=CARTESIAN_POINT('Origin',(58.,-46.8567596356166,-128.737889047669));
#52807=CARTESIAN_POINT('Origin',(14.,-57.8376305949206,-126.399400659835));
#52808=CARTESIAN_POINT('Origin',(58.,-57.8987018584758,-124.164166824021));
#52809=CARTESIAN_POINT('Origin',(14.,-68.5,-118.645480318468));
#52810=CARTESIAN_POINT('Origin',(14.,-68.6339745962156,-120.877531126037));
#52811=CARTESIAN_POINT('Origin',(14.,-78.9079726085065,-114.435710592521));
#52812=CARTESIAN_POINT('Origin',(58.,-78.5799717800934,-112.223830067592));
#52813=CARTESIAN_POINT('Origin',(14.,-88.58143330331,-107.122965203224));
#52814=CARTESIAN_POINT('Origin',(58.,-88.0619025270559,-104.9480887073));
#52815=CARTESIAN_POINT('Origin',(14.,-96.873629022557,-96.873629022557));
#52816=CARTESIAN_POINT('Origin',(58.,-96.873629022557,-96.873629022557));
#52817=CARTESIAN_POINT('Origin',(14.,-105.837389983851,-90.113522189548));
#52818=CARTESIAN_POINT('Origin',(58.,-104.9480887073,-88.0619025270559));
#52819=CARTESIAN_POINT('Origin',(14.,-112.223830067592,-78.5799717800933));
#52820=CARTESIAN_POINT('Origin',(14.,-113.288557719819,-80.5462766970844));
#52821=CARTESIAN_POINT('Origin',(14.,-119.877531126037,-70.3660254037844));
#52822=CARTESIAN_POINT('Origin',(58.,-118.645480318468,-68.5));
#52823=CARTESIAN_POINT('Origin',(14.,-125.554164136354,-59.6502461689939));
#52824=CARTESIAN_POINT('Origin',(58.,-124.164166824021,-57.8987018584758));
#52825=CARTESIAN_POINT('Origin',(14.,-128.737889047669,-46.8567596356166));
#52826=CARTESIAN_POINT('Origin',(58.,-128.737889047669,-46.8567596356166));
#52827=CARTESIAN_POINT('Origin',(14.,-134.004870809078,-36.9417730955394));
#52828=CARTESIAN_POINT('Origin',(58.,-132.331838201602,-35.4582091790453));
#52829=CARTESIAN_POINT('Origin',(14.,-134.918662162673,-23.7898003403695));
#52830=CARTESIAN_POINT('Origin',(14.,-136.71462949103,-25.1219044487155));
#52831=CARTESIAN_POINT('Origin',(14.,-138.383907292005,-13.1108429400162));
#52832=CARTESIAN_POINT('Origin',(58.,-136.478673638569,-11.9403367564291));
#52833=CARTESIAN_POINT('Origin',(14.,-139.,-0.999999999999992));
#52834=CARTESIAN_POINT('Origin',(58.,-137.,8.38883057415937E-15));
#52835=CARTESIAN_POINT('Origin',(14.,-136.478673638569,11.9403367564292));
#52836=CARTESIAN_POINT('Origin',(58.,-136.478673638569,11.9403367564292));
#52837=CARTESIAN_POINT('Origin',(14.,-137.061925846364,23.1522889426911));
#52838=CARTESIAN_POINT('Origin',(58.,-134.918662162673,23.7898003403695));
#52839=CARTESIAN_POINT('Origin',(14.,-132.331838201602,35.4582091790453));
#52840=CARTESIAN_POINT('Origin',(14.,-134.522508899283,35.0099214429613));
#52841=CARTESIAN_POINT('Origin',(14.,-130.959294432567,46.6011073014821));
#52842=CARTESIAN_POINT('Origin',(58.,-128.737889047669,46.8567596356166));
#52843=CARTESIAN_POINT('Origin',(14.,-126.399400659835,57.8376305949206));
#52844=CARTESIAN_POINT('Origin',(58.,-124.164166824021,57.8987018584758));
#52845=CARTESIAN_POINT('Origin',(14.,-118.645480318468,68.5));
#52846=CARTESIAN_POINT('Origin',(58.,-118.645480318468,68.5));
#52847=CARTESIAN_POINT('Origin',(14.,-114.435710592521,78.9079726085064));
#52848=CARTESIAN_POINT('Origin',(58.,-112.223830067592,78.5799717800933));
#52849=CARTESIAN_POINT('Origin',(14.,-104.9480887073,88.0619025270559));
#52850=CARTESIAN_POINT('Origin',(14.,-107.122965203224,88.58143330331));
#52851=CARTESIAN_POINT('Origin',(14.,-98.9949493661167,97.5807358037436));
#52852=CARTESIAN_POINT('Origin',(58.,-96.873629022557,96.873629022557));
#52853=CARTESIAN_POINT('Origin',(14.,-90.113522189548,105.837389983851));
#52854=CARTESIAN_POINT('Origin',(58.,-88.0619025270559,104.9480887073));
#52855=CARTESIAN_POINT('Origin',(14.,-78.5799717800933,112.223830067592));
#52856=CARTESIAN_POINT('Origin',(58.,-78.5799717800933,112.223830067592));
#52857=CARTESIAN_POINT('Origin',(14.,-70.3660254037844,119.877531126037));
#52858=CARTESIAN_POINT('Origin',(58.,-68.5,118.645480318468));
#52859=CARTESIAN_POINT('Origin',(14.,-57.8987018584758,124.164166824021));
#52860=CARTESIAN_POINT('Origin',(14.,-59.6502461689939,125.554164136354));
#52861=CARTESIAN_POINT('Origin',(14.,-48.4804925430539,130.275254145916));
#52862=CARTESIAN_POINT('Origin',(58.,-46.8567596356166,128.737889047669));
#52863=CARTESIAN_POINT('Origin',(14.,-36.9417730955394,134.004870809078));
#52864=CARTESIAN_POINT('Origin',(58.,-35.4582091790453,132.331838201602));
#52865=CARTESIAN_POINT('Origin',(14.,-23.7898003403695,134.918662162673));
#52866=CARTESIAN_POINT('Origin',(58.,-23.7898003403695,134.918662162673));
#52867=CARTESIAN_POINT('Origin',(14.,-13.1108429400162,138.383907292005));
#52868=CARTESIAN_POINT('Origin',(58.,-11.9403367564292,136.478673638569));
#52869=CARTESIAN_POINT('Origin',(14.,0.,137.));
#52870=CARTESIAN_POINT('Origin',(14.,-1.,139.));
#52871=CARTESIAN_POINT('Origin',(80.,33.5919271685148,-46.2353212285282));
#52872=CARTESIAN_POINT('',(62.,33.5919271685148,-39.0553212285282));
#52873=CARTESIAN_POINT('',(80.,33.5919271685148,-39.0553212285282));
#52874=CARTESIAN_POINT('Origin',(62.,33.5919271685148,-46.2353212285282));
#52875=CARTESIAN_POINT('Origin',(80.,-33.5919271685148,-46.2353212285282));
#52876=CARTESIAN_POINT('',(62.,-33.5919271685148,-39.0553212285282));
#52877=CARTESIAN_POINT('',(80.,-33.5919271685148,-39.0553212285282));
#52878=CARTESIAN_POINT('Origin',(62.,-33.5919271685148,-46.2353212285282));
#52879=CARTESIAN_POINT('Origin',(80.,-54.352879906268,17.6603212285283));
#52880=CARTESIAN_POINT('',(62.,-54.352879906268,24.8403212285282));
#52881=CARTESIAN_POINT('',(80.,-54.352879906268,24.8403212285282));
#52882=CARTESIAN_POINT('Origin',(62.,-54.352879906268,17.6603212285283));
#52883=CARTESIAN_POINT('Origin',(80.,3.49942822856356E-15,57.15));
#52884=CARTESIAN_POINT('',(62.,2.62013182677576E-15,64.33));
#52885=CARTESIAN_POINT('',(80.,4.37872463035136E-15,64.33));
#52886=CARTESIAN_POINT('Origin',(62.,3.49942822856356E-15,57.15));
#52887=CARTESIAN_POINT('Origin',(80.,54.352879906268,17.6603212285282));
#52888=CARTESIAN_POINT('',(62.,54.352879906268,24.8403212285282));
#52889=CARTESIAN_POINT('',(80.,54.352879906268,24.8403212285282));
#52890=CARTESIAN_POINT('Origin',(62.,54.352879906268,17.6603212285282));
#52891=CARTESIAN_POINT('Origin',(76.,0.,0.));
#52892=CARTESIAN_POINT('',(75.,-27.,-3.30654635769785E-15));
#52893=CARTESIAN_POINT('Origin',(75.,0.,0.));
#52894=CARTESIAN_POINT('',(77.,-23.,-2.81668763803891E-15));
#52895=CARTESIAN_POINT('',(76.,-25.,-3.06161699786838E-15));
#52896=CARTESIAN_POINT('Origin',(77.,0.,0.));
#52897=CARTESIAN_POINT('Origin',(78.5,0.,0.));
#52898=CARTESIAN_POINT('',(80.,-23.,-2.81668763803891E-15));
#52899=CARTESIAN_POINT('',(78.5,-23.,-2.81668763803891E-15));
#52900=CARTESIAN_POINT('Origin',(80.,0.,0.));
#52901=CARTESIAN_POINT('Origin',(72.,-54.352879906268,17.6603212285283));
#52902=CARTESIAN_POINT('',(72.,-43.6855709521459,28.205866244188));
#52903=CARTESIAN_POINT('',(72.,-43.6855709521459,28.205866244188));
#52904=CARTESIAN_POINT('Origin',(72.,-54.352879906268,17.6603212285283));
#52905=CARTESIAN_POINT('Origin',(72.,0.,0.));
#52906=CARTESIAN_POINT('',(72.,-13.3257890560989,50.2635389326334));
#52907=CARTESIAN_POINT('',(72.,-13.3257890560989,50.2635389326334));
#52908=CARTESIAN_POINT('Origin',(72.,0.,0.));
#52909=CARTESIAN_POINT('Origin',(72.,3.49942822856356E-15,57.15));
#52910=CARTESIAN_POINT('',(72.,13.3257890560989,50.2635389326334));
#52911=CARTESIAN_POINT('',(72.,13.3257890560989,50.2635389326334));
#52912=CARTESIAN_POINT('Origin',(72.,3.49942822856356E-15,57.15));
#52913=CARTESIAN_POINT('Origin',(72.,0.,0.));
#52914=CARTESIAN_POINT('Origin',(72.,0.,0.));
#52915=CARTESIAN_POINT('Origin',(72.,50.,0.));
#52916=CARTESIAN_POINT('Origin',(92.5,0.,0.));
#52917=CARTESIAN_POINT('',(80.,-25.16,-3.08121134665474E-15));
#52918=CARTESIAN_POINT('',(92.5,-25.16,-3.08121134665474E-15));
#52919=CARTESIAN_POINT('Origin',(80.,0.,0.));
#52920=CARTESIAN_POINT('Origin',(80.,23.,0.));
#52921=CARTESIAN_POINT('Origin',(54.5,0.,0.));
#52922=CARTESIAN_POINT('',(34.,-27.,-3.30654635769785E-15));
#52923=CARTESIAN_POINT('',(54.5,-27.,-3.30654635769785E-15));
#52924=CARTESIAN_POINT('Origin',(34.,0.,0.));
#52925=CARTESIAN_POINT('Origin',(34.,26.,0.));
#52926=CARTESIAN_POINT('Origin',(23.47,0.,0.));
#52927=CARTESIAN_POINT('',(15.,-29.58,-3.62250523187787E-15));
#52928=CARTESIAN_POINT('',(23.47,-29.58,-3.62250523187787E-15));
#52929=CARTESIAN_POINT('Origin',(15.,0.,0.));
#52930=CARTESIAN_POINT('Origin',(15.,32.6,0.));
#52931=CARTESIAN_POINT('',(15.,-32.6,-3.99234856522037E-15));
#52932=CARTESIAN_POINT('Origin',(15.,0.,0.));
#52933=CARTESIAN_POINT('Origin',(10.3,0.,0.));
#52934=CARTESIAN_POINT('',(5.6,-32.6,-3.99234856522037E-15));
#52935=CARTESIAN_POINT('',(10.3,-32.6,-3.99234856522037E-15));
#52936=CARTESIAN_POINT('Origin',(5.6,0.,0.));
#52937=CARTESIAN_POINT('Origin',(5.3,0.,0.));
#52938=CARTESIAN_POINT('',(5.3,-32.9,-4.02908796919479E-15));
#52939=CARTESIAN_POINT('Origin',(59.,0.,0.));
#52940=CARTESIAN_POINT('',(62.,-46.,-5.63337527607782E-15));
#52941=CARTESIAN_POINT('Origin',(62.,0.,0.));
#52942=CARTESIAN_POINT('',(59.,-43.,-5.26598123633362E-15));
#52943=CARTESIAN_POINT('Origin',(62.,123.,0.));
#52944=CARTESIAN_POINT('',(62.,-123.,-1.50631556295124E-14));
#52945=CARTESIAN_POINT('Origin',(62.,0.,0.));
#52946=CARTESIAN_POINT('Origin',(61.,0.,0.));
#52947=CARTESIAN_POINT('',(60.,-126.5,-1.5491782009214E-14));
#52948=CARTESIAN_POINT('',(61.,-124.75,-1.52774688193632E-14));
#52949=CARTESIAN_POINT('Origin',(60.,0.,0.));
#52950=CARTESIAN_POINT('Origin',(59.875,0.,0.));
#52951=CARTESIAN_POINT('',(59.875,-126.75,-1.55223981791927E-14));
#52952=CARTESIAN_POINT('',(0.,0.,0.));
#52953=CARTESIAN_POINT('Origin',(93.0806848796603,0.,0.));
#52954=CARTESIAN_POINT('',(106.687827736803,-11.5967315487946,7.87168637228455E-6));
#52955=CARTESIAN_POINT('',(107.068507977483,-11.5985329378162,-8.63915123328063E-5));
#52956=CARTESIAN_POINT('',(93.0806848796603,-11.59764,-5.19855242766535E-13));
#52957=CARTESIAN_POINT('',(108.008153428708,1.61683638546944,11.4839173606684));
#52958=CARTESIAN_POINT('Ctrl Pts',(106.687827736803,-11.5967315487946,7.87168637238211E-6));
#52959=CARTESIAN_POINT('Ctrl Pts',(106.711594970266,-11.596708823616,-0.954793789917175));
#52960=CARTESIAN_POINT('Ctrl Pts',(106.782454004811,-11.2488354439901,-3.80143203778901));
#52961=CARTESIAN_POINT('Ctrl Pts',(106.90040484044,-8.94469671038593,-8.10505773452174));
#52962=CARTESIAN_POINT('Ctrl Pts',(107.041680243689,-4.08614924745149,-11.3579434776441));
#52963=CARTESIAN_POINT('Ctrl Pts',(107.182955646938,1.73118676492076,-11.9458275473958));
#52964=CARTESIAN_POINT('Ctrl Pts',(107.324231050188,7.14228240914768,-9.73071187083892));
#52965=CARTESIAN_POINT('Ctrl Pts',(107.465506453437,10.8775923704873,-5.2324691939163));
#52966=CARTESIAN_POINT('Ctrl Pts',(107.606781856686,12.0604357325722,0.493684347847536));
#52967=CARTESIAN_POINT('Ctrl Pts',(107.748057259935,10.4137508886283,6.10364517469624));
#52968=CARTESIAN_POINT('Ctrl Pts',(107.881847783942,6.53964630458162,10.0607723786066));
#52969=CARTESIAN_POINT('Ctrl Pts',(107.968546506866,3.1919014918455,11.2608399260662));
#52970=CARTESIAN_POINT('Ctrl Pts',(108.008153428708,1.61683638546944,11.4839173606684));
#52971=CARTESIAN_POINT('',(108.381837686686,1.89465380507476,11.4418329182223));
#52972=CARTESIAN_POINT('Ctrl Pts',(108.381837686686,1.89465380507475,11.4418329182223));
#52973=CARTESIAN_POINT('Ctrl Pts',(108.245634554207,1.81427119940562,11.4551434787576));
#52974=CARTESIAN_POINT('Ctrl Pts',(108.119678552464,1.71980777108499,11.4698872225825));
#52975=CARTESIAN_POINT('Ctrl Pts',(108.008153428707,1.61690871966318,11.4843745916736));
#52976=CARTESIAN_POINT('',(107.547344722949,1.0134778581722,-11.5532729648613));
#52977=CARTESIAN_POINT('Ctrl Pts',(107.547344722949,1.01347785817195,-11.5532729648613));
#52978=CARTESIAN_POINT('Ctrl Pts',(107.609159016559,3.48672851139089,-11.3363141184487));
#52979=CARTESIAN_POINT('Ctrl Pts',(107.701880456974,7.0775262685878,-9.77461236926229));
#52980=CARTESIAN_POINT('Ctrl Pts',(107.825509044195,10.2343745743181,-5.85997992529276));
#52981=CARTESIAN_POINT('Ctrl Pts',(107.949137631415,12.0158490350764,-1.15276339618737));
#52982=CARTESIAN_POINT('Ctrl Pts',(108.072766218635,11.3809885644172,4.02471057714319));
#52983=CARTESIAN_POINT('Ctrl Pts',(108.227301952661,7.79854554867288,9.20330948728365));
#52984=CARTESIAN_POINT('Ctrl Pts',(108.320023393076,4.34404808711794,11.0362375708885));
#52985=CARTESIAN_POINT('Ctrl Pts',(108.381837686686,1.89465380507476,11.4418329182223));
#52986=CARTESIAN_POINT('',(107.3,-5.24483772964977E-16,-11.59764));
#52987=CARTESIAN_POINT('Ctrl Pts',(107.3,-1.2490009027033E-15,-11.59764));
#52988=CARTESIAN_POINT('Ctrl Pts',(107.3,0.276953548632659,-11.59764));
#52989=CARTESIAN_POINT('Ctrl Pts',(107.355486366965,0.571913365577543,-11.5867146442773));
#52990=CARTESIAN_POINT('Ctrl Pts',(107.491919613987,0.900866393499067,-11.5627453043894));
#52991=CARTESIAN_POINT('Ctrl Pts',(107.518478464707,0.957861594797325,-11.5581517426463));
#52992=CARTESIAN_POINT('Ctrl Pts',(107.547344722949,1.01347785817219,-11.5532729648613));
#52993=CARTESIAN_POINT('',(107.499276121999,-0.914933857717795,-11.5614942635285));
#52994=CARTESIAN_POINT('Ctrl Pts',(107.499276121999,-0.914933857717795,
-11.5614942635285));
#52995=CARTESIAN_POINT('Ctrl Pts',(107.488376247984,-0.891098650368292,
-11.563380493605));
#52996=CARTESIAN_POINT('Ctrl Pts',(107.4778971503,-0.867056951964309,-11.565208847591));
#52997=CARTESIAN_POINT('Ctrl Pts',(107.355486366965,-0.571913365577543,
-11.5867146442773));
#52998=CARTESIAN_POINT('Ctrl Pts',(107.3,-0.27695354863266,-11.59764));
#52999=CARTESIAN_POINT('Ctrl Pts',(107.3,4.85722573273506E-16,-11.59764));
#53000=CARTESIAN_POINT('Ctrl Pts',(107.068507977483,-11.5985329378162,-8.63915123330145E-5));
#53001=CARTESIAN_POINT('Ctrl Pts',(107.070148102946,-11.5985543598099,-0.0659446921696183));
#53002=CARTESIAN_POINT('Ctrl Pts',(107.119104647089,-11.5821690115654,-2.03175412121691));
#53003=CARTESIAN_POINT('Ctrl Pts',(107.215377609914,-10.5467853781223,-5.88028127277808));
#53004=CARTESIAN_POINT('Ctrl Pts',(107.357326865957,-6.5216081564048,-10.1627828959428));
#53005=CARTESIAN_POINT('Ctrl Pts',(107.451959703319,-2.80945746568101,-11.4115686783349));
#53006=CARTESIAN_POINT('Ctrl Pts',(107.499276121999,-0.914933857717795,
-11.5614942635285));
#53007=CARTESIAN_POINT('Origin',(93.0806848796603,0.,0.));
#53008=CARTESIAN_POINT('',(104.873542022517,-11.5970620128151,-0.000217152463837714));
#53009=CARTESIAN_POINT('',(105.254222263197,-11.5979149765058,0.000262464412231905));
#53010=CARTESIAN_POINT('',(93.0806848796603,-11.59764,-5.19855242766535E-13));
#53011=CARTESIAN_POINT('Ctrl Pts',(104.873542022517,-11.5970620128151,-0.000217152463837314));
#53012=CARTESIAN_POINT('Ctrl Pts',(104.889877746662,-11.5975244094225,-0.656419016915337));
#53013=CARTESIAN_POINT('Ctrl Pts',(104.95330527189,-11.3847135734158,-3.20398978174987));
#53014=CARTESIAN_POINT('Ctrl Pts',(105.063824598201,-9.54321881653396,-7.39097662401987));
#53015=CARTESIAN_POINT('Ctrl Pts',(105.20510000145,-4.95004576133935,-11.0089330909609));
#53016=CARTESIAN_POINT('Ctrl Pts',(105.346375404699,0.80460272604254,-12.0437608442455));
#53017=CARTESIAN_POINT('Ctrl Pts',(105.487650807948,6.3704597694178,-10.2526485946914));
#53018=CARTESIAN_POINT('Ctrl Pts',(105.628926211197,10.4415563792162,-6.05586171641488));
#53019=CARTESIAN_POINT('Ctrl Pts',(105.770201614447,12.062653180839,-0.438131499218847));
#53020=CARTESIAN_POINT('Ctrl Pts',(105.911477017696,10.8533770682464,5.28240162572942));
#53021=CARTESIAN_POINT('Ctrl Pts',(106.052752420945,7.09747185328678,9.76347550654746));
#53022=CARTESIAN_POINT('Ctrl Pts',(106.194027824194,1.67622047878578,11.9536541207404));
#53023=CARTESIAN_POINT('Ctrl Pts',(106.335303227443,-4.13833793915172,11.3390350829177));
#53024=CARTESIAN_POINT('Ctrl Pts',(106.476578630693,-8.98187994449148,8.0638328962862));
#53025=CARTESIAN_POINT('Ctrl Pts',(106.594086800479,-11.2576257684445,3.76584875965195));
#53026=CARTESIAN_POINT('Ctrl Pts',(106.664503169183,-11.5967538507156,0.937026307393627));
#53027=CARTESIAN_POINT('Ctrl Pts',(106.687827736803,-11.5967315487946,7.87168637238211E-6));
#53028=CARTESIAN_POINT('Ctrl Pts',(105.254222263197,-11.5979149765058,0.000262464412231628));
#53029=CARTESIAN_POINT('Ctrl Pts',(105.292827269251,-11.596406322082,-1.55016204041523));
#53030=CARTESIAN_POINT('Ctrl Pts',(105.378748693986,-10.8995437237543,-5.00218789188436));
#53031=CARTESIAN_POINT('Ctrl Pts',(105.511986537402,-7.57509950853803,-9.40367293367282));
#53032=CARTESIAN_POINT('Ctrl Pts',(105.653935793445,-2.23922610928576,-11.8657938991006));
#53033=CARTESIAN_POINT('Ctrl Pts',(105.795885049488,3.6269801590525,-11.5176477156709));
#53034=CARTESIAN_POINT('Ctrl Pts',(105.93783430553,8.63418136051829,-8.44168924241129));
#53035=CARTESIAN_POINT('Ctrl Pts',(106.079783561573,11.5964822941979,-3.36641977915706));
#53036=CARTESIAN_POINT('Ctrl Pts',(106.221732817616,11.8123013659403,2.50614254258396));
#53037=CARTESIAN_POINT('Ctrl Pts',(106.363682073658,9.23051857694247,7.78516037256956));
#53038=CARTESIAN_POINT('Ctrl Pts',(106.505631329701,4.46260964811663,11.2203497277713));
#53039=CARTESIAN_POINT('Ctrl Pts',(106.647580585744,-1.36223065258046,11.9981569780826));
#53040=CARTESIAN_POINT('Ctrl Pts',(106.789529841786,-6.86440734641473,9.9343085302927));
#53041=CARTESIAN_POINT('Ctrl Pts',(106.929838972366,-10.6961186798297,5.56875601983415));
#53042=CARTESIAN_POINT('Ctrl Pts',(107.022831684265,-11.597936350978,1.83401905935505));
#53043=CARTESIAN_POINT('Ctrl Pts',(107.068507977483,-11.5985329378162,-8.63915123330145E-5));
#53044=CARTESIAN_POINT('Origin',(93.0806848796603,0.,0.));
#53045=CARTESIAN_POINT('',(103.059256308232,-11.5978818050668,-0.000259090622128178));
#53046=CARTESIAN_POINT('',(103.439936548911,-11.5968529998687,0.000153614214355446));
#53047=CARTESIAN_POINT('',(93.0806848796603,-11.59764,-5.19855242766535E-13));
#53048=CARTESIAN_POINT('Ctrl Pts',(103.059256308232,-11.5978818050668,-0.000259090622127499));
#53049=CARTESIAN_POINT('Ctrl Pts',(103.068160523058,-11.5982264103411,-0.357866351962969));
#53050=CARTESIAN_POINT('Ctrl Pts',(103.124156538968,-11.4961896948955,-2.60655846572717));
#53051=CARTESIAN_POINT('Ctrl Pts',(103.227244355961,-10.0848767600063,-6.63285923053644));
#53052=CARTESIAN_POINT('Ctrl Pts',(103.36851975921,-5.7844519333586,-10.5943228508145));
#53053=CARTESIAN_POINT('Ctrl Pts',(103.50979516246,-0.126767166023071,-12.0699416287838));
#53054=CARTESIAN_POINT('Ctrl Pts',(103.651070565709,5.56066216453452,-10.7134773593142));
#53055=CARTESIAN_POINT('Ctrl Pts',(103.792345968958,9.94334143638835,-6.84320991319397));
#53056=CARTESIAN_POINT('Ctrl Pts',(103.933621372207,11.992921710502,-1.36725626068703));
#53057=CARTESIAN_POINT('Ctrl Pts',(104.074896775456,11.2284908393957,4.42950948822145));
#53058=CARTESIAN_POINT('Ctrl Pts',(104.216172178705,7.82941437242525,9.18693808738774));
#53059=CARTESIAN_POINT('Ctrl Pts',(104.357447581955,2.59324934302537,11.7887496657387));
#53060=CARTESIAN_POINT('Ctrl Pts',(104.498722985204,-3.25139398131772,11.6244568911889));
#53061=CARTESIAN_POINT('Ctrl Pts',(104.639998388453,-8.33313239206491,8.73260931064738));
#53062=CARTESIAN_POINT('Ctrl Pts',(104.764938067557,-11.0980767761605,4.36306161391605));
#53063=CARTESIAN_POINT('Ctrl Pts',(104.842785945579,-11.5961914358203,1.23524659872623));
#53064=CARTESIAN_POINT('Ctrl Pts',(104.873542022517,-11.5970620128151,-0.000217152463837314));
#53065=CARTESIAN_POINT('Ctrl Pts',(103.439936548911,-11.5968529998687,0.000153614214355169));
#53066=CARTESIAN_POINT('Ctrl Pts',(103.468190016876,-11.5963058546535,-1.1348392538219));
#53067=CARTESIAN_POINT('Ctrl Pts',(103.543759903522,-11.1534213600585,-4.17103610100268));
#53068=CARTESIAN_POINT('Ctrl Pts',(103.666646208848,-8.54072618632016,-8.53622829798181));
#53069=CARTESIAN_POINT('Ctrl Pts',(103.808595464891,-3.49996651231003,-11.5568781146813));
#53070=CARTESIAN_POINT('Ctrl Pts',(103.950544720934,2.36971705558015,-11.8404239122457));
#53071=CARTESIAN_POINT('Ctrl Pts',(104.092493976976,7.67816237096933,-9.3197113662083));
#53072=CARTESIAN_POINT('Ctrl Pts',(104.234443233019,11.168129644454,-4.59174014842598));
#53073=CARTESIAN_POINT('Ctrl Pts',(104.376392489061,12.0130631783326,1.22372808128535));
#53074=CARTESIAN_POINT('Ctrl Pts',(104.518341745104,10.0128508883889,6.74937141017876));
#53075=CARTESIAN_POINT('Ctrl Pts',(104.660291001147,5.64121838056578,10.6765093795372));
#53076=CARTESIAN_POINT('Ctrl Pts',(104.802240257189,-0.0664671110029323,
12.0750478032933));
#53077=CARTESIAN_POINT('Ctrl Pts',(104.944189513232,-5.75841068985474,10.6137601120454));
#53078=CARTESIAN_POINT('Ctrl Pts',(105.086138769275,-10.0865457254805,6.63873426049027));
#53079=CARTESIAN_POINT('Ctrl Pts',(105.189483019263,-11.4983987440124,2.60007647808839));
#53080=CARTESIAN_POINT('Ctrl Pts',(105.24551085057,-11.5982554119192,0.35012350546277));
#53081=CARTESIAN_POINT('Ctrl Pts',(105.254222263197,-11.5979149765058,0.000262464412231628));
#53082=CARTESIAN_POINT('Origin',(93.0806848796603,0.,0.));
#53083=CARTESIAN_POINT('',(101.244970593946,-11.5985409258756,-5.7588822467809E-5));
#53084=CARTESIAN_POINT('',(101.625650834626,-11.5969301646075,-0.000186353423677899));
#53085=CARTESIAN_POINT('',(93.0806848796603,-11.59764,-5.19855242766535E-13));
#53086=CARTESIAN_POINT('Ctrl Pts',(101.244970593946,-11.5985409258756,-5.75888224674682E-5));
#53087=CARTESIAN_POINT('Ctrl Pts',(101.246443299455,-11.5985577555476,-0.0591940151317032));
#53088=CARTESIAN_POINT('Ctrl Pts',(101.295007806047,-11.5839431479448,-2.00929134158216));
#53089=CARTESIAN_POINT('Ctrl Pts',(101.390664113722,-10.5664450398852,-5.83522065184453));
#53090=CARTESIAN_POINT('Ctrl Pts',(101.531939516971,-6.58439206452233,-10.1165874669912));
#53091=CARTESIAN_POINT('Ctrl Pts',(101.67321492022,-1.05738173003248,-12.0242049514145));
#53092=CARTESIAN_POINT('Ctrl Pts',(101.814490323469,4.71773194782029,-11.1104710118493));
#53093=CARTESIAN_POINT('Ctrl Pts',(101.955765726718,9.38588015038702,-7.58978356998396));
#53094=CARTESIAN_POINT('Ctrl Pts',(102.097041129968,11.8517316992723,-2.28823437722007));
#53095=CARTESIAN_POINT('Ctrl Pts',(102.238316533217,11.5367008329307,3.55022460248401));
#53096=CARTESIAN_POINT('Ctrl Pts',(102.379591936466,8.51470618356667,8.55566125113419));
#53097=CARTESIAN_POINT('Ctrl Pts',(102.520867339715,3.49482655861225,11.5536032544763));
#53098=CARTESIAN_POINT('Ctrl Pts',(102.662142742964,-2.34507683735861,11.8406155018864));
#53099=CARTESIAN_POINT('Ctrl Pts',(102.803418146214,-7.63473296948303,9.34935363120446));
#53100=CARTESIAN_POINT('Ctrl Pts',(102.935789334636,-10.912495171678,4.95964805911867));
#53101=CARTESIAN_POINT('Ctrl Pts',(103.021068721975,-11.5964038933259,1.53341438918833));
#53102=CARTESIAN_POINT('Ctrl Pts',(103.059256308232,-11.5978818050668,-0.000259090622127499));
#53103=CARTESIAN_POINT('Ctrl Pts',(101.625650834626,-11.5969301646075,-0.000186353423678731));
#53104=CARTESIAN_POINT('Ctrl Pts',(101.643552764501,-11.5973545849506,-0.719325510492189));
#53105=CARTESIAN_POINT('Ctrl Pts',(101.708771113057,-11.3573577041451,-3.33893460572594));
#53106=CARTESIAN_POINT('Ctrl Pts',(101.821305880294,-9.40766205636401,-7.57014477921035));
#53107=CARTESIAN_POINT('Ctrl Pts',(101.963255136337,-4.72026363022087,-11.1144189504522));
#53108=CARTESIAN_POINT('Ctrl Pts',(102.105204392379,1.08507100893144,-12.0263800975411));
#53109=CARTESIAN_POINT('Ctrl Pts',(102.247153648422,6.63341996474086,-10.0900414724784));
#53110=CARTESIAN_POINT('Ctrl Pts',(102.389102904465,10.610725229854,-5.76400099249621));
#53111=CARTESIAN_POINT('Ctrl Pts',(102.531052160507,12.0750111151176,-0.0728279804925511));
#53112=CARTESIAN_POINT('Ctrl Pts',(102.67300141655,10.6794795716148,5.63559344030584));
#53113=CARTESIAN_POINT('Ctrl Pts',(102.814950672592,6.75464503055027,10.0092940738206));
#53114=CARTESIAN_POINT('Ctrl Pts',(102.956899928635,1.23005613734974,12.0124168777114));
#53115=CARTESIAN_POINT('Ctrl Pts',(103.098849184678,-4.58585637836471,11.1705469258209));
#53116=CARTESIAN_POINT('Ctrl Pts',(103.24079844072,-9.31566538066349,7.68307073119021));
#53117=CARTESIAN_POINT('Ctrl Pts',(103.354494228798,-11.3368967970257,3.4322783363807));
#53118=CARTESIAN_POINT('Ctrl Pts',(103.420873598195,-11.59722216525,0.765946795195559));
#53119=CARTESIAN_POINT('Ctrl Pts',(103.439936548911,-11.5968529998687,0.000153614214355169));
#53120=CARTESIAN_POINT('Origin',(93.0806848796603,0.,0.));
#53121=CARTESIAN_POINT('',(99.4306848796602,-11.5982123705775,0.000204477995816285));
#53122=CARTESIAN_POINT('',(99.8113651203399,-11.5980517843054,-0.000244059920104789));
#53123=CARTESIAN_POINT('',(93.0806848796603,-11.59764,-5.19855242766535E-13));
#53124=CARTESIAN_POINT('Ctrl Pts',(99.4306848796602,-11.5982123705775,0.000204477995815917));
#53125=CARTESIAN_POINT('Ctrl Pts',(99.4718178769342,-11.5968382129007,-1.6516251690263));
#53126=CARTESIAN_POINT('Ctrl Pts',(99.5600426752913,-10.8315259674307,-5.19581284549921));
#53127=CARTESIAN_POINT('Ctrl Pts',(99.6953592747313,-7.34509979707817,-9.57857347461386));
#53128=CARTESIAN_POINT('Ctrl Pts',(99.8366346779806,-1.98169599765362,-11.9068233298798));
#53129=CARTESIAN_POINT('Ctrl Pts',(99.9779100812298,3.84669162792076,-11.4412641065812));
#53130=CARTESIAN_POINT('Ctrl Pts',(100.119185484479,8.77249409748291,-8.29113430998339));
#53131=CARTESIAN_POINT('Ctrl Pts',(100.260460887728,11.6399244073961,-3.19557829300717));
#53132=CARTESIAN_POINT('Ctrl Pts',(100.401736290977,11.7761706236747,2.64978608169418));
#53133=CARTESIAN_POINT('Ctrl Pts',(100.543011694227,9.14926402506894,7.8734064188378));
#53134=CARTESIAN_POINT('Ctrl Pts',(100.684287097476,4.37558022249231,11.2496159291403));
#53135=CARTESIAN_POINT('Ctrl Pts',(100.825562500725,-1.42478680291599,11.9862230666236));
#53136=CARTESIAN_POINT('Ctrl Pts',(100.966837903974,-6.89084280389226,9.91039082421449));
#53137=CARTESIAN_POINT('Ctrl Pts',(101.106640601714,-10.699910676898,5.55507077934471));
#53138=CARTESIAN_POINT('Ctrl Pts',(101.199351498372,-11.5980196034472,1.83177523010779));
#53139=CARTESIAN_POINT('Ctrl Pts',(101.244970593946,-11.5985409258756,-5.75888224674682E-5));
#53140=CARTESIAN_POINT('Ctrl Pts',(99.8113651203399,-11.5980517843054,-0.000244059920105136));
#53141=CARTESIAN_POINT('Ctrl Pts',(99.8189155121257,-11.5983353502102,-0.303466742622632));
#53142=CARTESIAN_POINT('Ctrl Pts',(99.8737823225923,-11.5136117348972,-2.50675216138025));
#53143=CARTESIAN_POINT('Ctrl Pts',(99.9759655517397,-10.1658893729505,-6.51658580867914));
#53144=CARTESIAN_POINT('Ctrl Pts',(100.117914807782,-5.88601658741872,-10.5435291092497));
#53145=CARTESIAN_POINT('Ctrl Pts',(100.259864063825,-0.212113381356825,
-12.0733676022228));
#53146=CARTESIAN_POINT('Ctrl Pts',(100.401813319868,5.51202626250981,-10.7437779121853));
#53147=CARTESIAN_POINT('Ctrl Pts',(100.54376257591,9.93071048086492,-6.8696569557873));
#53148=CARTESIAN_POINT('Ctrl Pts',(100.685711831953,11.997428424203,-1.36854249151505));
#53149=CARTESIAN_POINT('Ctrl Pts',(100.827661087996,11.2227034420802,4.45669437992771));
#53150=CARTESIAN_POINT('Ctrl Pts',(100.969610344038,7.7900195897285,9.22641816397909));
#53151=CARTESIAN_POINT('Ctrl Pts',(101.111559600081,2.51236569298111,11.8109786203214));
#53152=CARTESIAN_POINT('Ctrl Pts',(101.253508856124,-3.3603110263314,11.5982544872611));
#53153=CARTESIAN_POINT('Ctrl Pts',(101.395458112166,-8.43713953088349,8.63862685161016));
#53154=CARTESIAN_POINT('Ctrl Pts',(101.519505438333,-11.1274784823704,4.26432569210168));
#53155=CARTESIAN_POINT('Ctrl Pts',(101.59623634582,-11.5962328036236,1.18142427920913));
#53156=CARTESIAN_POINT('Ctrl Pts',(101.625650834626,-11.5969301646075,-0.000186353423678731));
#53157=CARTESIAN_POINT('Origin',(93.0806848796603,0.,0.));
#53158=CARTESIAN_POINT('',(97.6163991653745,-11.5973549676912,0.000264155725229257));
#53159=CARTESIAN_POINT('',(97.9970794060541,-11.5984942842416,0.000109136483176162));
#53160=CARTESIAN_POINT('',(93.0806848796603,-11.59764,-5.19855242766535E-13));
#53161=CARTESIAN_POINT('Ctrl Pts',(97.6163991653745,-11.5973549676912,0.00026415572522899));
#53162=CARTESIAN_POINT('Ctrl Pts',(97.6501006533306,-11.5961500955102,-1.35341785052988));
#53163=CARTESIAN_POINT('Ctrl Pts',(97.7308939423697,-11.0276899039031,-4.59961573681585));
#53164=CARTESIAN_POINT('Ctrl Pts',(97.8587790324919,-8.06204243838756,-8.9834859317315));
#53165=CARTESIAN_POINT('Ctrl Pts',(98.0000544357412,-2.89420258720722,-11.7184964778204));
#53166=CARTESIAN_POINT('Ctrl Pts',(98.1413298389903,2.95273122806244,-11.7038855003407));
#53167=CARTESIAN_POINT('Ctrl Pts',(98.2826052422396,8.10683806242452,-8.94308328046984));
#53168=CARTESIAN_POINT('Ctrl Pts',(98.4238806454887,11.3587618711925,-4.08388166193566));
#53169=CARTESIAN_POINT('Ctrl Pts',(98.5651560487379,11.9454733539258,1.73355907649387));
#53170=CARTESIAN_POINT('Ctrl Pts',(98.706431451987,9.7293069528249,7.14423874107845));
#53171=CARTESIAN_POINT('Ctrl Pts',(98.8477068552363,5.23026245722293,10.8785989620564));
#53172=CARTESIAN_POINT('Ctrl Pts',(98.9889822584854,-0.496007327832227,
12.0604120000411));
#53173=CARTESIAN_POINT('Ctrl Pts',(99.1302576617347,-6.10589428573641,10.4123780084834));
#53174=CARTESIAN_POINT('Ctrl Pts',(99.2715330649838,-10.2830982833774,6.32119059473821));
#53175=CARTESIAN_POINT('Ctrl Pts',(99.371675470959,-11.5337740761537,2.36981230115211));
#53176=CARTESIAN_POINT('Ctrl Pts',(99.4247260758512,-11.59841144034,0.23949967759091));
#53177=CARTESIAN_POINT('Ctrl Pts',(99.4306848796602,-11.5982123705775,0.000204477995815917));
#53178=CARTESIAN_POINT('Ctrl Pts',(97.9970794060541,-11.5984942842416,0.000109136483176196));
#53179=CARTESIAN_POINT('Ctrl Pts',(98.0415946784313,-11.5976002818738,-1.7874203035197));
#53180=CARTESIAN_POINT('Ctrl Pts',(98.1334263694893,-10.7312077943355,-5.47579749744129));
#53181=CARTESIAN_POINT('Ctrl Pts',(98.2725744792281,-6.98375473307958,-9.85080540269698));
#53182=CARTESIAN_POINT('Ctrl Pts',(98.4145237352708,-1.50684673412838,-11.9808434723489));
#53183=CARTESIAN_POINT('Ctrl Pts',(98.5564729913134,4.32693932863066,-11.2733665501931));
#53184=CARTESIAN_POINT('Ctrl Pts',(98.6984222473561,9.13594318590594,-7.89593182926991));
#53185=CARTESIAN_POINT('Ctrl Pts',(98.8403715033986,11.781211598614,-2.64844305476444));
#53186=CARTESIAN_POINT('Ctrl Pts',(98.9823207594414,11.6362453734974,3.22629678599122));
#53187=CARTESIAN_POINT('Ctrl Pts',(99.124270015484,8.73537797318143,8.33692803205455));
#53188=CARTESIAN_POINT('Ctrl Pts',(99.2662192715265,3.76564405694391,11.4730607154675));
#53189=CARTESIAN_POINT('Ctrl Pts',(99.4081685275693,-2.0959362022484,11.8919404968782));
#53190=CARTESIAN_POINT('Ctrl Pts',(99.5501177836118,-7.46111982681854,9.49436086710135));
#53191=CARTESIAN_POINT('Ctrl Pts',(99.6845166478687,-10.8678430079567,5.09529409224268));
#53192=CARTESIAN_POINT('Ctrl Pts',(99.7715990934448,-11.59655831354,1.59675404265655));
#53193=CARTESIAN_POINT('Ctrl Pts',(99.8113651203399,-11.5980517843054,-0.000244059920105136));
#53194=CARTESIAN_POINT('Origin',(93.0806848796603,0.,0.));
#53195=CARTESIAN_POINT('',(115.759256308232,-11.5966977159097,-2.20020729888378E-5));
#53196=CARTESIAN_POINT('',(116.139936548911,-11.5978562621874,0.000265160474589299));
#53197=CARTESIAN_POINT('',(93.0806848796603,-11.59764,-5.19855242766535E-13));
#53198=CARTESIAN_POINT('',(117.38636,-9.24570028839849,7.00280438584369));
#53199=CARTESIAN_POINT('Ctrl Pts',(115.759256308232,-11.5966977159097,-2.20020729886639E-5));
#53200=CARTESIAN_POINT('Ctrl Pts',(115.782472788843,-11.5967602494871,-0.932708015072538));
#53201=CARTESIAN_POINT('Ctrl Pts',(115.853334649975,-11.2572698648965,-3.77942835970487));
#53202=CARTESIAN_POINT('Ctrl Pts',(115.971841891627,-8.95294307109407,-8.11300498914965));
#53203=CARTESIAN_POINT('Ctrl Pts',(116.11477803319,-4.0242321603504,-11.3921725585846));
#53204=CARTESIAN_POINT('Ctrl Pts',(116.257714174752,1.87059427966267,-11.9363694039364));
#53205=CARTESIAN_POINT('Ctrl Pts',(116.400650316314,7.31633898196617,-9.61494819743955));
#53206=CARTESIAN_POINT('Ctrl Pts',(116.543586457876,11.005616292,-4.98522204048877));
#53207=CARTESIAN_POINT('Ctrl Pts',(116.686522599438,12.0527268155209,0.841327506667632));
#53208=CARTESIAN_POINT('Ctrl Pts',(116.829458741,10.2062813712173,6.46589893037503));
#53209=CARTESIAN_POINT('Ctrl Pts',(116.972394882562,5.9095743448429,10.5381658364625));
#53210=CARTESIAN_POINT('Ctrl Pts',(117.115331024124,0.194114641227306,12.0805020392623));
#53211=CARTESIAN_POINT('Ctrl Pts',(117.253319396603,-5.36846226369204,10.7695908115406));
#53212=CARTESIAN_POINT('Ctrl Pts',(117.343662388562,-8.20939703265164,8.36879965219385));
#53213=CARTESIAN_POINT('Ctrl Pts',(117.38636,-9.24570028839849,7.00280438584369));
#53214=CARTESIAN_POINT('',(117.38636,4.47152467205382,10.7009682121205));
#53215=CARTESIAN_POINT('Origin',(117.38636,0.,0.));
#53216=CARTESIAN_POINT('Ctrl Pts',(116.139936548911,-11.5978562621874,0.000265160474589889));
#53217=CARTESIAN_POINT('Ctrl Pts',(116.177899585767,-11.5963703069285,-1.52440435616002));
#53218=CARTESIAN_POINT('Ctrl Pts',(116.263051553478,-10.917763149328,-4.94555756957596));
#53219=CARTESIAN_POINT('Ctrl Pts',(116.395392452043,-7.64837610766902,-9.34078625853751));
#53220=CARTESIAN_POINT('Ctrl Pts',(116.536959244609,-2.34918804318456,-11.8418520279979));
#53221=CARTESIAN_POINT('Ctrl Pts',(116.678526037174,3.50341987815323,-11.5530757135873));
#53222=CARTESIAN_POINT('Ctrl Pts',(116.820092829739,8.53070918247288,-8.54259995247553));
#53223=CARTESIAN_POINT('Ctrl Pts',(116.961659622304,11.5481555073598,-3.51942696985816));
#53224=CARTESIAN_POINT('Ctrl Pts',(117.103226414869,11.8451994508802,2.33252276799301));
#53225=CARTESIAN_POINT('Ctrl Pts',(117.244793207435,9.35114240419514,7.63559939886844));
#53226=CARTESIAN_POINT('Ctrl Pts',(117.339171069145,6.22031361682587,9.97021630652136));
#53227=CARTESIAN_POINT('Ctrl Pts',(117.38636,4.47152467205382,10.7009682121205));
#53228=CARTESIAN_POINT('Origin',(93.0806848796603,0.,0.));
#53229=CARTESIAN_POINT('',(113.944970593946,-11.5979544128403,-0.000269279950390758));
#53230=CARTESIAN_POINT('',(114.325650834626,-11.5969419105478,0.000182072225077823));
#53231=CARTESIAN_POINT('',(93.0806848796603,-11.59764,-5.19855242766535E-13));
#53232=CARTESIAN_POINT('Ctrl Pts',(113.944970593946,-11.5979544128403,-0.000269279950390472));
#53233=CARTESIAN_POINT('Ctrl Pts',(113.95355903255,-11.5982957222328,-0.345189041569635));
#53234=CARTESIAN_POINT('Ctrl Pts',(114.009792851675,-11.4995210665118,-2.60339725427472));
#53235=CARTESIAN_POINT('Ctrl Pts',(114.11367205132,-10.078006847733,-6.66406913873543));
#53236=CARTESIAN_POINT('Ctrl Pts',(114.256608192883,-5.7025528495123,-10.6516163368671));
#53237=CARTESIAN_POINT('Ctrl Pts',(114.399544334445,0.0419388972008348,
-12.0819816539827));
#53238=CARTESIAN_POINT('Ctrl Pts',(114.542480476007,5.77636218068765,-10.6117708005521));
#53239=CARTESIAN_POINT('Ctrl Pts',(114.685416617569,10.1240279793146,-6.59394396708397));
#53240=CARTESIAN_POINT('Ctrl Pts',(114.828352759131,12.0411724308134,-0.993079077887869));
#53241=CARTESIAN_POINT('Ctrl Pts',(114.971288900693,11.0675379662367,4.84619881277042));
#53242=CARTESIAN_POINT('Ctrl Pts',(115.114225042255,7.43686942972829,9.52202775941664));
#53243=CARTESIAN_POINT('Ctrl Pts',(115.257161183817,2.02079789647468,11.9118602837624));
#53244=CARTESIAN_POINT('Ctrl Pts',(115.400097325379,-3.88041576111888,11.4419584473181));
#53245=CARTESIAN_POINT('Ctrl Pts',(115.543033466941,-8.85004039162967,8.22513371169866));
#53246=CARTESIAN_POINT('Ctrl Pts',(115.662753127892,-11.23290225591,3.87689112845648));
#53247=CARTESIAN_POINT('Ctrl Pts',(115.734827408322,-11.5966319166816,0.981371071238124));
#53248=CARTESIAN_POINT('Ctrl Pts',(115.759256308232,-11.5966977159097,-2.20020729886639E-5));
#53249=CARTESIAN_POINT('Ctrl Pts',(114.325650834626,-11.5969419105478,0.000182072225077753));
#53250=CARTESIAN_POINT('Ctrl Pts',(114.354919675127,-11.5962607053732,-1.17557795589793));
#53251=CARTESIAN_POINT('Ctrl Pts',(114.431377446484,-11.1315096647659,-4.24749348564229));
#53252=CARTESIAN_POINT('Ctrl Pts',(114.555024148696,-8.45978526537628,-8.6127818545234));
#53253=CARTESIAN_POINT('Ctrl Pts',(114.696590941261,-3.40781807628825,-11.581655924795));
#53254=CARTESIAN_POINT('Ctrl Pts',(114.838157733826,2.44699275634759,-11.8220220132816));
#53255=CARTESIAN_POINT('Ctrl Pts',(114.979724526391,7.72531959196485,-9.2772525651793));
#53256=CARTESIAN_POINT('Ctrl Pts',(115.121291318956,11.1836479525214,-4.54686667674157));
#53257=CARTESIAN_POINT('Ctrl Pts',(115.262858111522,12.0072345239343,1.25470992130988));
#53258=CARTESIAN_POINT('Ctrl Pts',(115.404424904087,10.0020516002354,6.76069092494371));
#53259=CARTESIAN_POINT('Ctrl Pts',(115.545991696652,5.64049766960815,10.6739292014239));
#53260=CARTESIAN_POINT('Ctrl Pts',(115.687558489217,-0.0498940161182073,
12.0725095394857));
#53261=CARTESIAN_POINT('Ctrl Pts',(115.829125281783,-5.72853146574744,10.6269426623712));
#53262=CARTESIAN_POINT('Ctrl Pts',(115.970692074348,-10.0575907787097,6.67778673879954));
#53263=CARTESIAN_POINT('Ctrl Pts',(116.074295830057,-11.4917013921148,2.63631752302503));
#53264=CARTESIAN_POINT('Ctrl Pts',(116.130710654912,-11.5982173836055,0.370795036632186));
#53265=CARTESIAN_POINT('Ctrl Pts',(116.139936548911,-11.5978562621874,0.000265160474589889));
#53266=CARTESIAN_POINT('Origin',(93.0806848796603,0.,0.));
#53267=CARTESIAN_POINT('',(112.13068487966,-11.5982247539793,0.000228379848985116));
#53268=CARTESIAN_POINT('',(112.51136512034,-11.5967929078458,-0.000103121459272826));
#53269=CARTESIAN_POINT('',(93.0806848796603,-11.59764,-5.19855242766535E-13));
#53270=CARTESIAN_POINT('Ctrl Pts',(112.13068487966,-11.5982247539793,0.000228379848985077));
#53271=CARTESIAN_POINT('Ctrl Pts',(112.172290656778,-11.596775601192,-1.67056794358247));
#53272=CARTESIAN_POINT('Ctrl Pts',(112.261541814416,-10.8135367102492,-5.25606952472166));
#53273=CARTESIAN_POINT('Ctrl Pts',(112.398438352575,-7.24939531411746,-9.66549613681094));
#53274=CARTESIAN_POINT('Ctrl Pts',(112.541374494138,-1.78769147784434,-11.9490739890003));
#53275=CARTESIAN_POINT('Ctrl Pts',(112.6843106357,4.1032269254419,-11.363957802295));
#53276=CARTESIAN_POINT('Ctrl Pts',(112.827246777262,9.00904847698782,-8.05065674001605));
#53277=CARTESIAN_POINT('Ctrl Pts',(112.970182918824,11.7520346070574,-2.80459235140811));
#53278=CARTESIAN_POINT('Ctrl Pts',(113.113119060386,11.6736528323709,3.11478061972093));
#53279=CARTESIAN_POINT('Ctrl Pts',(113.256055201948,8.79272593142687,8.28637530125792));
#53280=CARTESIAN_POINT('Ctrl Pts',(113.39899134351,3.80088861740511,11.4686216793657));
#53281=CARTESIAN_POINT('Ctrl Pts',(113.541927485072,-2.10344490785294,11.897544267814));
#53282=CARTESIAN_POINT('Ctrl Pts',(113.684863626634,-7.50279504034574,9.47016927888733));
#53283=CARTESIAN_POINT('Ctrl Pts',(113.819211329592,-10.8847189596875,5.05170665773232));
#53284=CARTESIAN_POINT('Ctrl Pts',(113.905913652029,-11.5964022679471,1.56829419431985));
#53285=CARTESIAN_POINT('Ctrl Pts',(113.944970593946,-11.5979544128403,-0.000269279950390472));
#53286=CARTESIAN_POINT('Ctrl Pts',(112.51136512034,-11.5967929078458,-0.000103121459272826));
#53287=CARTESIAN_POINT('Ctrl Pts',(112.531939764487,-11.5970590783192,-0.826638577717111));
#53288=CARTESIAN_POINT('Ctrl Pts',(112.59970333949,-11.3098683964611,-3.54869026150752));
#53289=CARTESIAN_POINT('Ctrl Pts',(112.714655845348,-9.20221848328371,-7.81454784931888));
#53290=CARTESIAN_POINT('Ctrl Pts',(112.856222637913,-4.43865660418402,-11.2270344946451));
#53291=CARTESIAN_POINT('Ctrl Pts',(112.997789430478,1.37060254033464,-11.9945582342283));
#53292=CARTESIAN_POINT('Ctrl Pts',(113.139356223043,6.85696329237368,-9.9362987275659));
#53293=CARTESIAN_POINT('Ctrl Pts',(113.280923015609,10.7279004735232,-5.53715895830823));
#53294=CARTESIAN_POINT('Ctrl Pts',(113.422489808174,12.0714648968156,0.166473261964394));
#53295=CARTESIAN_POINT('Ctrl Pts',(113.564056600739,10.5711278304476,5.83088624039759));
#53296=CARTESIAN_POINT('Ctrl Pts',(113.705623393304,6.58035185125043,10.1216079525872));
#53297=CARTESIAN_POINT('Ctrl Pts',(113.847190185869,1.03931892093069,12.0277925731204));
#53298=CARTESIAN_POINT('Ctrl Pts',(113.988756978435,-4.74656586578709,11.1003644305775));
#53299=CARTESIAN_POINT('Ctrl Pts',(114.130323771,-9.41421307630654,7.55781517133264));
#53300=CARTESIAN_POINT('Ctrl Pts',(114.242621723064,-11.3574903143052,3.33527400553394));
#53301=CARTESIAN_POINT('Ctrl Pts',(114.307730744272,-11.5973589840659,0.720050901223368));
#53302=CARTESIAN_POINT('Ctrl Pts',(114.325650834626,-11.5969419105478,0.000182072225077753));
#53303=CARTESIAN_POINT('Origin',(117.798242418585,0.,-8.05687251955465E-17));
#53304=CARTESIAN_POINT('',(118.,-3.4268292682927,-4.19665549463912E-16));
#53305=CARTESIAN_POINT('Origin',(118.,0.,0.));
#53306=CARTESIAN_POINT('',(117.596484837171,-2.63157427110059,0.));
#53307=CARTESIAN_POINT('',(117.798242418585,-3.02920176969664,-5.32107675514142E-16));
#53308=CARTESIAN_POINT('Origin',(117.596484837171,0.,-1.61137450391093E-16));
#53309=CARTESIAN_POINT('Origin',(116.05,0.,0.));
#53310=CARTESIAN_POINT('',(114.,0.,0.));
#53311=CARTESIAN_POINT('',(116.05,-1.5,-1.83697019872103E-16));
#53312=CARTESIAN_POINT('Origin',(118.,0.,0.));
#53313=CARTESIAN_POINT('',(118.,-12.,-1.46957615897682E-15));
#53314=CARTESIAN_POINT('Origin',(118.,0.,0.));
#53315=CARTESIAN_POINT('Origin',(94.75,4.6,-12.25));
#53316=CARTESIAN_POINT('',(95.,-2.7,-12.));
#53317=CARTESIAN_POINT('',(94.5,-2.7,-12.5));
#53318=CARTESIAN_POINT('',(99.7500000000001,-2.7,-7.24999999999999));
#53319=CARTESIAN_POINT('',(94.5,2.7,-12.5));
#53320=CARTESIAN_POINT('',(94.5,4.6,-12.5));
#53321=CARTESIAN_POINT('',(95.,2.7,-12.));
#53322=CARTESIAN_POINT('',(100.625,2.7,-6.375));
#53323=CARTESIAN_POINT('',(95.,4.6,-12.));
#53324=CARTESIAN_POINT('Origin',(118.5,-2.7,-12.5));
#53325=CARTESIAN_POINT('',(86.,-2.7,-12.5));
#53326=CARTESIAN_POINT('',(118.5,-2.7,-12.5));
#53327=CARTESIAN_POINT('',(86.,2.7,-12.5));
#53328=CARTESIAN_POINT('',(86.,-2.7,-12.5));
#53329=CARTESIAN_POINT('',(118.5,2.7,-12.5));
#53330=CARTESIAN_POINT('Origin',(-22.,-41.9267766952966,53.8232233047034));
#53331=CARTESIAN_POINT('',(-14.3232233047034,-41.9267766952966,53.8232233047034));
#53332=CARTESIAN_POINT('',(-14.5,-41.5,54.));
#53333=CARTESIAN_POINT('',(-24.5071980214169,-17.3404868153423,64.0071980214168));
#53334=CARTESIAN_POINT('',(-21.5,-41.5,54.));
#53335=CARTESIAN_POINT('',(-22.,-41.5,54.));
#53336=CARTESIAN_POINT('',(-21.6767766952966,-41.9267766952966,53.8232233047034));
#53337=CARTESIAN_POINT('',(-12.0037603021723,-18.5740493299586,63.4962396978277));
#53338=CARTESIAN_POINT('',(-21.5,-42.3535533905933,53.6464466094067));
#53339=CARTESIAN_POINT('',(-21.0638697904486,-43.4064648574528,53.2103163998554));
#53340=CARTESIAN_POINT('',(-14.5,-42.3535533905933,53.6464466094067));
#53341=CARTESIAN_POINT('',(-22.,-42.3535533905933,53.6464466094067));
#53342=CARTESIAN_POINT('',(-15.4470885331405,-44.6400273720691,52.6993580762662));
#53343=CARTESIAN_POINT('Origin',(-22.,-42.,54.));
#53344=CARTESIAN_POINT('',(-21.5,-53.6464466094067,42.3535533905933));
#53345=CARTESIAN_POINT('',(-21.5,-45.,51.));
#53346=CARTESIAN_POINT('',(-14.5,-53.6464466094067,42.3535533905933));
#53347=CARTESIAN_POINT('',(-22.,-53.6464466094067,42.3535533905933));
#53348=CARTESIAN_POINT('',(-14.5,-45.,51.));
#53349=CARTESIAN_POINT('Origin',(-21.75,-44.8232233047034,50.8232233047034));
#53350=CARTESIAN_POINT('',(-22.,-41.7928932188134,53.5));
#53351=CARTESIAN_POINT('',(-22.,-41.7928932188134,53.5));
#53352=CARTESIAN_POINT('',(-22.,-53.5,41.7928932188135));
#53353=CARTESIAN_POINT('',(-22.,-44.6464466094067,50.6464466094067));
#53354=CARTESIAN_POINT('',(-22.,-53.5,41.7928932188135));
#53355=CARTESIAN_POINT('Origin',(-21.75,21.,53.75));
#53356=CARTESIAN_POINT('',(-21.5,41.5,54.));
#53357=CARTESIAN_POINT('',(-21.5,21.,54.));
#53358=CARTESIAN_POINT('',(-21.6767766952966,41.9267766952966,53.8232233047034));
#53359=CARTESIAN_POINT('',(-18.4799635039079,34.2089869322727,57.0200364960921));
#53360=CARTESIAN_POINT('',(-22.,41.7928932188135,53.5));
#53361=CARTESIAN_POINT('',(-22.,41.7928932188135,53.5));
#53362=CARTESIAN_POINT('',(-22.,21.,53.5));
#53363=CARTESIAN_POINT('Origin',(-14.5,41.5,54.));
#53364=CARTESIAN_POINT('',(-14.5,42.3535533905933,53.6464466094067));
#53365=CARTESIAN_POINT('',(-14.,41.7928932188134,53.5));
#53366=CARTESIAN_POINT('',(-14.5,42.3535533905933,53.6464466094067));
#53367=CARTESIAN_POINT('',(-14.5,41.5,54.));
#53368=CARTESIAN_POINT('',(-14.5,41.5,54.));
#53369=CARTESIAN_POINT('',(-14.,41.7928932188134,53.5));
#53370=CARTESIAN_POINT('Origin',(-22.,41.9267766952966,53.8232233047034));
#53371=CARTESIAN_POINT('',(-22.,41.5,54.));
#53372=CARTESIAN_POINT('',(-21.5,42.3535533905933,53.6464466094067));
#53373=CARTESIAN_POINT('',(-22.,42.3535533905933,53.6464466094067));
#53374=CARTESIAN_POINT('',(-19.7554791617946,46.5651992580313,51.9019257712013));
#53375=CARTESIAN_POINT('Origin',(-14.25,21.,53.75));
#53376=CARTESIAN_POINT('',(-14.,-41.7928932188134,53.5));
#53377=CARTESIAN_POINT('',(-7.85670147864286,-39.2482556535607,47.3567014786429));
#53378=CARTESIAN_POINT('',(-14.,21.,53.5));
#53379=CARTESIAN_POINT('',(-14.5,21.,54.));
#53380=CARTESIAN_POINT('Origin',(-14.5,53.6464466094067,42.3535533905933));
#53381=CARTESIAN_POINT('',(-14.5,54.,41.5));
#53382=CARTESIAN_POINT('',(-14.,53.5,41.7928932188135));
#53383=CARTESIAN_POINT('',(-14.5,54.,41.5));
#53384=CARTESIAN_POINT('',(-14.5,53.6464466094067,42.3535533905933));
#53385=CARTESIAN_POINT('',(-14.5,53.6464466094067,42.3535533905933));
#53386=CARTESIAN_POINT('',(-14.,53.5,41.7928932188134));
#53387=CARTESIAN_POINT('Origin',(-22.,53.8232233047034,41.9267766952966));
#53388=CARTESIAN_POINT('',(-21.6767766952966,53.8232233047034,41.9267766952966));
#53389=CARTESIAN_POINT('',(-21.5,53.6464466094067,42.3535533905933));
#53390=CARTESIAN_POINT('',(-21.0638697904486,53.2103163998554,43.4064648574528));
#53391=CARTESIAN_POINT('',(-22.,53.6464466094067,42.3535533905933));
#53392=CARTESIAN_POINT('',(-21.5,54.,41.5));
#53393=CARTESIAN_POINT('',(-22.,54.,41.5));
#53394=CARTESIAN_POINT('',(-12.0037603021723,63.4962396978277,18.5740493299586));
#53395=CARTESIAN_POINT('Origin',(-14.25,50.8232233047034,44.8232233047034));
#53396=CARTESIAN_POINT('',(-14.,50.6464466094067,44.6464466094067));
#53397=CARTESIAN_POINT('',(-14.5,51.,45.));
#53398=CARTESIAN_POINT('Origin',(-14.5,54.,-41.5));
#53399=CARTESIAN_POINT('',(-14.5,53.6464466094067,-42.3535533905933));
#53400=CARTESIAN_POINT('',(-14.,53.5,-41.7928932188134));
#53401=CARTESIAN_POINT('',(-14.5,53.6464466094067,-42.3535533905933));
#53402=CARTESIAN_POINT('',(-14.5,54.,-41.5));
#53403=CARTESIAN_POINT('',(-14.5,54.,-41.5));
#53404=CARTESIAN_POINT('',(-14.,53.5,-41.7928932188134));
#53405=CARTESIAN_POINT('Origin',(-22.,53.8232233047034,-41.9267766952966));
#53406=CARTESIAN_POINT('',(-21.6767766952966,53.8232233047034,-41.9267766952966));
#53407=CARTESIAN_POINT('',(-21.5,54.,-41.5));
#53408=CARTESIAN_POINT('',(-18.4799635039079,57.0200364960921,-34.2089869322727));
#53409=CARTESIAN_POINT('',(-22.,54.,-41.5));
#53410=CARTESIAN_POINT('',(-21.5,53.6464466094067,-42.3535533905933));
#53411=CARTESIAN_POINT('',(-22.,53.6464466094067,-42.3535533905933));
#53412=CARTESIAN_POINT('',(-19.7554791617946,51.9019257712013,-46.5651992580313));
#53413=CARTESIAN_POINT('Origin',(-14.25,53.75,-21.));
#53414=CARTESIAN_POINT('',(-14.,53.5,-21.));
#53415=CARTESIAN_POINT('',(-14.5,54.,-21.));
#53416=CARTESIAN_POINT('Origin',(-14.5,42.3535533905933,-53.6464466094067));
#53417=CARTESIAN_POINT('',(-14.5,41.5,-54.));
#53418=CARTESIAN_POINT('',(-14.,41.7928932188135,-53.5));
#53419=CARTESIAN_POINT('',(-14.5,41.5,-54.));
#53420=CARTESIAN_POINT('',(-14.5,42.3535533905933,-53.6464466094067));
#53421=CARTESIAN_POINT('',(-14.5,42.3535533905933,-53.6464466094067));
#53422=CARTESIAN_POINT('',(-14.,41.7928932188134,-53.5));
#53423=CARTESIAN_POINT('Origin',(-22.,41.9267766952966,-53.8232233047034));
#53424=CARTESIAN_POINT('',(-21.6767766952966,41.9267766952966,-53.8232233047034));
#53425=CARTESIAN_POINT('',(-21.5,42.3535533905933,-53.6464466094067));
#53426=CARTESIAN_POINT('',(-21.0638697904486,43.4064648574528,-53.2103163998554));
#53427=CARTESIAN_POINT('',(-22.,42.3535533905933,-53.6464466094067));
#53428=CARTESIAN_POINT('',(-21.5,41.5,-54.));
#53429=CARTESIAN_POINT('',(-22.,41.5,-54.));
#53430=CARTESIAN_POINT('',(-12.0037603021723,18.5740493299586,-63.4962396978277));
#53431=CARTESIAN_POINT('Origin',(-14.25,44.8232233047034,-50.8232233047034));
#53432=CARTESIAN_POINT('',(-14.,44.6464466094067,-50.6464466094067));
#53433=CARTESIAN_POINT('',(-14.5,45.,-51.));
#53434=CARTESIAN_POINT('Origin',(-14.5,-41.5,-54.));
#53435=CARTESIAN_POINT('',(-14.5,-42.3535533905933,-53.6464466094067));
#53436=CARTESIAN_POINT('',(-14.,-41.7928932188134,-53.5));
#53437=CARTESIAN_POINT('',(-14.5,-42.3535533905933,-53.6464466094067));
#53438=CARTESIAN_POINT('',(-14.5,-41.5,-54.));
#53439=CARTESIAN_POINT('',(-14.5,-41.5,-54.));
#53440=CARTESIAN_POINT('',(-14.,-41.7928932188134,-53.5));
#53441=CARTESIAN_POINT('Origin',(-22.,-41.9267766952966,-53.8232233047034));
#53442=CARTESIAN_POINT('',(-21.6767766952966,-41.9267766952966,-53.8232233047034));
#53443=CARTESIAN_POINT('',(-21.5,-41.5,-54.));
#53444=CARTESIAN_POINT('',(-18.4799635039079,-34.2089869322727,-57.0200364960921));
#53445=CARTESIAN_POINT('',(-22.,-41.5,-54.));
#53446=CARTESIAN_POINT('',(-21.5,-42.3535533905933,-53.6464466094067));
#53447=CARTESIAN_POINT('',(-22.,-42.3535533905933,-53.6464466094067));
#53448=CARTESIAN_POINT('',(-19.7554791617946,-46.5651992580313,-51.9019257712013));
#53449=CARTESIAN_POINT('Origin',(-14.25,-21.,-53.75));
#53450=CARTESIAN_POINT('',(-14.,-21.,-53.5));
#53451=CARTESIAN_POINT('',(-14.5,-21.,-54.));
#53452=CARTESIAN_POINT('Origin',(-14.5,-53.6464466094067,-42.3535533905933));
#53453=CARTESIAN_POINT('',(-14.5,-54.,-41.5));
#53454=CARTESIAN_POINT('',(-14.,-53.5,-41.7928932188135));
#53455=CARTESIAN_POINT('',(-14.5,-54.,-41.5));
#53456=CARTESIAN_POINT('',(-14.5,-53.6464466094067,-42.3535533905933));
#53457=CARTESIAN_POINT('',(-14.5,-53.6464466094067,-42.3535533905933));
#53458=CARTESIAN_POINT('',(-14.,-53.5,-41.7928932188134));
#53459=CARTESIAN_POINT('Origin',(-22.,-53.8232233047034,-41.9267766952966));
#53460=CARTESIAN_POINT('',(-21.6767766952966,-53.8232233047034,-41.9267766952966));
#53461=CARTESIAN_POINT('',(-21.5,-53.6464466094067,-42.3535533905933));
#53462=CARTESIAN_POINT('',(-21.0638697904486,-53.2103163998554,-43.4064648574528));
#53463=CARTESIAN_POINT('',(-22.,-53.6464466094067,-42.3535533905933));
#53464=CARTESIAN_POINT('',(-21.5,-54.,-41.5));
#53465=CARTESIAN_POINT('',(-22.,-54.,-41.5));
#53466=CARTESIAN_POINT('',(-12.0037603021723,-63.4962396978277,-18.5740493299586));
#53467=CARTESIAN_POINT('Origin',(-14.25,-50.8232233047034,-44.8232233047034));
#53468=CARTESIAN_POINT('',(-14.,-50.6464466094067,-44.6464466094067));
#53469=CARTESIAN_POINT('',(-14.5,-51.,-45.));
#53470=CARTESIAN_POINT('Origin',(-14.25,-53.75,21.));
#53471=CARTESIAN_POINT('',(-14.3232233047034,-53.8232233047034,41.9267766952966));
#53472=CARTESIAN_POINT('',(-14.5,-54.,41.5));
#53473=CARTESIAN_POINT('',(-18.0309948196813,-57.5309948196812,32.9754244176564));
#53474=CARTESIAN_POINT('',(-14.5,-54.,21.));
#53475=CARTESIAN_POINT('',(-14.,-53.5,41.7928932188134));
#53476=CARTESIAN_POINT('',(-14.,-53.5,21.));
#53477=CARTESIAN_POINT('',(-11.0530600149149,-50.5530600149149,40.5722307094916));
#53478=CARTESIAN_POINT('Origin',(-21.75,53.75,-21.));
#53479=CARTESIAN_POINT('',(-22.,53.5,-41.7928932188135));
#53480=CARTESIAN_POINT('',(-22.,53.5,-41.7928932188135));
#53481=CARTESIAN_POINT('',(-22.,53.5,41.7928932188134));
#53482=CARTESIAN_POINT('',(-22.,53.5,-21.));
#53483=CARTESIAN_POINT('',(-22.,53.5,41.7928932188134));
#53484=CARTESIAN_POINT('',(-21.5,54.,-21.));
#53485=CARTESIAN_POINT('Origin',(-22.,42.,-54.));
#53486=CARTESIAN_POINT('',(-21.5,45.,-51.));
#53487=CARTESIAN_POINT('Origin',(-21.75,44.8232233047034,-50.8232233047034));
#53488=CARTESIAN_POINT('',(-22.,41.7928932188134,-53.5));
#53489=CARTESIAN_POINT('',(-22.,41.7928932188134,-53.5));
#53490=CARTESIAN_POINT('',(-22.,44.6464466094067,-50.6464466094067));
#53491=CARTESIAN_POINT('Origin',(-22.,-42.,-54.));
#53492=CARTESIAN_POINT('',(-21.5,-21.,-54.));
#53493=CARTESIAN_POINT('Origin',(-21.75,-21.,-53.75));
#53494=CARTESIAN_POINT('',(-22.,-41.7928932188135,-53.5));
#53495=CARTESIAN_POINT('',(-22.,-41.7928932188135,-53.5));
#53496=CARTESIAN_POINT('',(-22.,-21.,-53.5));
#53497=CARTESIAN_POINT('Origin',(-22.,-54.,-42.));
#53498=CARTESIAN_POINT('',(-21.5,-51.,-45.));
#53499=CARTESIAN_POINT('Origin',(-21.75,-50.8232233047034,-44.8232233047034));
#53500=CARTESIAN_POINT('',(-22.,-53.5,-41.7928932188134));
#53501=CARTESIAN_POINT('',(-22.,-53.5,-41.7928932188134));
#53502=CARTESIAN_POINT('',(-22.,-50.6464466094067,-44.6464466094067));
#53503=CARTESIAN_POINT('Origin',(-21.75,-53.75,21.));
#53504=CARTESIAN_POINT('',(-21.5,-54.,41.5));
#53505=CARTESIAN_POINT('',(-21.5,-54.,21.));
#53506=CARTESIAN_POINT('',(-21.5,-54.,41.5));
#53507=CARTESIAN_POINT('',(-22.,-53.5,21.));
#53508=CARTESIAN_POINT('Origin',(-22.,-54.,42.));
#53509=CARTESIAN_POINT('',(-22.,-54.,41.5));
#53510=CARTESIAN_POINT('Origin',(-22.,-53.8232233047034,41.9267766952966));
#53511=CARTESIAN_POINT('',(-14.1464466094067,-54.,41.5));
#53512=CARTESIAN_POINT('',(-21.5,-53.6464466094067,42.3535533905933));
#53513=CARTESIAN_POINT('Origin',(-14.25,34.7896536343781,-34.7896536343781));
#53514=CARTESIAN_POINT('',(-14.,34.7896536343781,-27.5396536343781));
#53515=CARTESIAN_POINT('Origin',(-14.,34.7896536343781,-34.7896536343781));
#53516=CARTESIAN_POINT('',(-14.5,34.7896536343781,-28.0396536343781));
#53517=CARTESIAN_POINT('',(-14.25,34.7896536343781,-27.7896536343781));
#53518=CARTESIAN_POINT('Origin',(-14.5,34.7896536343781,-34.7896536343781));
#53519=CARTESIAN_POINT('Origin',(-14.,0.,0.));
#53520=CARTESIAN_POINT('',(-14.,-44.6464466094067,50.6464466094067));
#53521=CARTESIAN_POINT('',(-14.,34.7896536343781,42.0396536343781));
#53522=CARTESIAN_POINT('Origin',(-14.,34.7896536343781,34.7896536343781));
#53523=CARTESIAN_POINT('',(-14.,-34.7896536343781,-27.5396536343781));
#53524=CARTESIAN_POINT('Origin',(-14.,-34.7896536343781,-34.7896536343781));
#53525=CARTESIAN_POINT('',(-14.,-25.4,-3.11060286983428E-15));
#53526=CARTESIAN_POINT('Origin',(-14.,0.,0.));
#53527=CARTESIAN_POINT('',(-14.,-34.7896536343781,42.0396536343781));
#53528=CARTESIAN_POINT('Origin',(-14.,-34.7896536343781,34.7896536343781));
#53529=CARTESIAN_POINT('Origin',(-22.,34.7896536343781,-34.7896536343781));
#53530=CARTESIAN_POINT('',(-21.5,34.7896536343781,-28.0396536343781));
#53531=CARTESIAN_POINT('Origin',(-21.5,34.7896536343781,-34.7896536343781));
#53532=CARTESIAN_POINT('',(-22.,34.7896536343781,-28.0396536343781));
#53533=CARTESIAN_POINT('Origin',(-14.25,34.7896536343781,34.7896536343781));
#53534=CARTESIAN_POINT('',(-14.5,34.7896536343781,41.5396536343781));
#53535=CARTESIAN_POINT('',(-14.25,34.7896536343781,41.7896536343781));
#53536=CARTESIAN_POINT('Origin',(-14.5,34.7896536343781,34.7896536343781));
#53537=CARTESIAN_POINT('Origin',(-22.,34.7896536343781,34.7896536343781));
#53538=CARTESIAN_POINT('',(-21.5,34.7896536343781,41.5396536343781));
#53539=CARTESIAN_POINT('Origin',(-21.5,34.7896536343781,34.7896536343781));
#53540=CARTESIAN_POINT('',(-22.,34.7896536343781,41.5396536343781));
#53541=CARTESIAN_POINT('Origin',(-14.25,-34.7896536343781,34.7896536343781));
#53542=CARTESIAN_POINT('',(-14.5,-34.7896536343781,41.5396536343781));
#53543=CARTESIAN_POINT('',(-14.25,-34.7896536343781,41.7896536343781));
#53544=CARTESIAN_POINT('Origin',(-14.5,-34.7896536343781,34.7896536343781));
#53545=CARTESIAN_POINT('Origin',(-22.,-34.7896536343781,34.7896536343781));
#53546=CARTESIAN_POINT('',(-21.5,-34.7896536343781,41.5396536343781));
#53547=CARTESIAN_POINT('Origin',(-21.5,-34.7896536343781,34.7896536343781));
#53548=CARTESIAN_POINT('',(-22.,-34.7896536343781,41.5396536343781));
#53549=CARTESIAN_POINT('Origin',(-14.25,-34.7896536343781,-34.7896536343781));
#53550=CARTESIAN_POINT('',(-14.5,-34.7896536343781,-28.0396536343781));
#53551=CARTESIAN_POINT('',(-14.25,-34.7896536343781,-27.7896536343781));
#53552=CARTESIAN_POINT('Origin',(-14.5,-34.7896536343781,-34.7896536343781));
#53553=CARTESIAN_POINT('Origin',(-22.,-34.7896536343781,-34.7896536343781));
#53554=CARTESIAN_POINT('',(-21.5,-34.7896536343781,-28.0396536343781));
#53555=CARTESIAN_POINT('Origin',(-21.5,-34.7896536343781,-34.7896536343781));
#53556=CARTESIAN_POINT('',(-22.,-34.7896536343781,-28.0396536343781));
#53557=CARTESIAN_POINT('Origin',(-21.75,-34.7896536343781,-34.7896536343781));
#53558=CARTESIAN_POINT('',(-22.,-34.7896536343781,-27.5396536343781));
#53559=CARTESIAN_POINT('Origin',(-22.,-34.7896536343781,-34.7896536343781));
#53560=CARTESIAN_POINT('',(-21.75,-34.7896536343781,-27.7896536343781));
#53561=CARTESIAN_POINT('Origin',(-22.,0.,0.));
#53562=CARTESIAN_POINT('',(-22.,50.6464466094067,44.6464466094067));
#53563=CARTESIAN_POINT('',(-22.,-34.7896536343781,42.0396536343781));
#53564=CARTESIAN_POINT('Origin',(-22.,-34.7896536343781,34.7896536343781));
#53565=CARTESIAN_POINT('',(-22.,34.7896536343781,-27.5396536343781));
#53566=CARTESIAN_POINT('Origin',(-22.,34.7896536343781,-34.7896536343781));
#53567=CARTESIAN_POINT('',(-22.,-25.4,3.11060286983428E-15));
#53568=CARTESIAN_POINT('Origin',(-22.,0.,0.));
#53569=CARTESIAN_POINT('',(-22.,34.7896536343781,42.0396536343781));
#53570=CARTESIAN_POINT('Origin',(-22.,34.7896536343781,34.7896536343781));
#53571=CARTESIAN_POINT('Origin',(-21.75,-34.7896536343781,34.7896536343781));
#53572=CARTESIAN_POINT('',(-21.75,-34.7896536343781,41.7896536343781));
#53573=CARTESIAN_POINT('Origin',(-21.75,34.7896536343781,34.7896536343781));
#53574=CARTESIAN_POINT('',(-21.75,34.7896536343781,41.7896536343781));
#53575=CARTESIAN_POINT('Origin',(-21.75,34.7896536343781,-34.7896536343781));
#53576=CARTESIAN_POINT('',(-21.75,34.7896536343781,-27.7896536343781));
#53577=CARTESIAN_POINT('Origin',(-21.75,50.8232233047034,44.8232233047034));
#53578=CARTESIAN_POINT('',(-21.5,51.,45.));
#53579=CARTESIAN_POINT('Origin',(-21.5,-54.,41.5));
#53580=CARTESIAN_POINT('Origin',(-14.25,-44.8232233047034,50.8232233047034));
#53581=CARTESIAN_POINT('Origin',(-22.,54.,-42.));
#53582=CARTESIAN_POINT('Origin',(-22.,54.,42.));
#53583=CARTESIAN_POINT('Origin',(-22.,42.,54.));
#53584=CARTESIAN_POINT('Origin',(-44.1267766952966,0.,-7.66826266755626E-16));
#53585=CARTESIAN_POINT('',(-43.7,25.4,-3.11060286983428E-15));
#53586=CARTESIAN_POINT('',(-43.7,-25.4,-3.11060286983428E-15));
#53587=CARTESIAN_POINT('Origin',(-43.7,0.,0.));
#53588=CARTESIAN_POINT('Origin',(-43.7,0.,0.));
#53589=CARTESIAN_POINT('',(-44.5535533905933,25.0464466094067,3.0673050670225E-15));
#53590=CARTESIAN_POINT('',(-44.1267766952966,25.2232233047034,3.08895396842839E-15));
#53591=CARTESIAN_POINT('',(-44.5535533905933,-25.0464466094067,-3.0673050670225E-15));
#53592=CARTESIAN_POINT('Origin',(-44.5535533905933,0.,-1.53365253351125E-15));
#53593=CARTESIAN_POINT('Origin',(-44.5535533905933,0.,-1.53365253351125E-15));
#53594=CARTESIAN_POINT('Origin',(-44.6,0.,0.));
#53595=CARTESIAN_POINT('',(-44.6464466094067,-24.9535533905933,-3.05592892871426E-15));
#53596=CARTESIAN_POINT('',(-44.6,-25.,-3.06161699786838E-15));
#53597=CARTESIAN_POINT('',(-44.6464466094067,24.9535533905933,-3.05592892871426E-15));
#53598=CARTESIAN_POINT('Origin',(-44.6464466094067,0.,-1.52796446435713E-15));
#53599=CARTESIAN_POINT('Origin',(-44.6464466094067,0.,-1.52796446435713E-15));
#53600=CARTESIAN_POINT('Origin',(-29.1,0.,0.));
#53601=CARTESIAN_POINT('',(-29.1,-25.4,-3.11060286983428E-15));
#53602=CARTESIAN_POINT('Origin',(-44.8232233047034,0.,-7.63982232178566E-16));
#53603=CARTESIAN_POINT('',(-45.,24.1,2.95139878594512E-15));
#53604=CARTESIAN_POINT('',(-44.8232233047034,24.5267766952966,3.00366385732969E-15));
#53605=CARTESIAN_POINT('Origin',(-45.,0.,0.));
#53606=CARTESIAN_POINT('Origin',(-45.,24.6,0.));
#53607=CARTESIAN_POINT('Ctrl Pts',(110.283043754069,-1.58298314962059,11.4890999611639));
#53608=CARTESIAN_POINT('Ctrl Pts',(110.314848605759,-2.84845815047358,11.3147411681003));
#53609=CARTESIAN_POINT('Ctrl Pts',(110.410263160827,-6.56679889300614,10.166830914177));
#53610=CARTESIAN_POINT('Ctrl Pts',(110.537482567584,-10.3238350595526,6.31146214230268));
#53611=CARTESIAN_POINT('Ctrl Pts',(110.696506826031,-12.0956797652182,0.0747112542218324));
#53612=CARTESIAN_POINT('Ctrl Pts',(110.855531084478,-10.6569271560527,-6.51026421705393));
#53613=CARTESIAN_POINT('Ctrl Pts',(111.014555342924,-5.44549032378077,-10.8066656409731));
#53614=CARTESIAN_POINT('Ctrl Pts',(111.109969897992,-1.63327529727618,-11.552899780549));
#53615=CARTESIAN_POINT('Ctrl Pts',(111.141774749681,-0.356448559383722,
-11.5921610579785));
#53616=CARTESIAN_POINT('Ctrl Pts',(110.478573045235,-1.62920838395028,11.8245971128989));
#53617=CARTESIAN_POINT('Ctrl Pts',(110.510377896924,-2.93163695469239,11.6451468088683));
#53618=CARTESIAN_POINT('Ctrl Pts',(110.605792451992,-6.75855824161194,10.4637160335864));
#53619=CARTESIAN_POINT('Ctrl Pts',(110.73301185875,-10.6253049109047,6.49576531480387));
#53620=CARTESIAN_POINT('Ctrl Pts',(110.892036117196,-12.448889862027,0.0768929232018998));
#53621=CARTESIAN_POINT('Ctrl Pts',(111.051060375643,-10.9681237440525,-6.70037267718105));
#53622=CARTESIAN_POINT('Ctrl Pts',(111.21008463409,-5.60450595595427,-11.1222347938706));
#53623=CARTESIAN_POINT('Ctrl Pts',(111.305499189158,-1.68096912987296,-11.8902599727099));
#53624=CARTESIAN_POINT('Ctrl Pts',(111.337304040847,-0.366857336121472,
-11.9306677321785));
#53625=CARTESIAN_POINT('Ctrl Pts',(110.674102336401,-1.67543361827996,12.1600942646339));
#53626=CARTESIAN_POINT('Ctrl Pts',(110.70590718809,-3.0148157589112,11.9755524496363));
#53627=CARTESIAN_POINT('Ctrl Pts',(110.801321743158,-6.95031759021774,10.7606011529959));
#53628=CARTESIAN_POINT('Ctrl Pts',(110.928541149915,-10.9267747622568,6.68006848730506));
#53629=CARTESIAN_POINT('Ctrl Pts',(111.087565408362,-12.8020999588358,0.0790745921819644));
#53630=CARTESIAN_POINT('Ctrl Pts',(111.246589666809,-11.2793203320523,-6.89048113730818));
#53631=CARTESIAN_POINT('Ctrl Pts',(111.405613925255,-5.76352158812776,-11.437803946768));
#53632=CARTESIAN_POINT('Ctrl Pts',(111.501028480323,-1.72866296246974,-12.2276201648708));
#53633=CARTESIAN_POINT('Ctrl Pts',(111.532833332013,-0.377266112859221,
-12.2691744063785));
#53634=CARTESIAN_POINT('Ctrl Pts',(110.869631627566,-1.72165885260965,12.4955914163688));
#53635=CARTESIAN_POINT('Ctrl Pts',(110.901436479255,-3.09799456313001,12.3059580904043));
#53636=CARTESIAN_POINT('Ctrl Pts',(110.996851034323,-7.14207693882354,11.0574862724054));
#53637=CARTESIAN_POINT('Ctrl Pts',(111.124070441081,-11.2282446136089,6.86437165980624));
#53638=CARTESIAN_POINT('Ctrl Pts',(111.283094699527,-13.1553100556447,0.0812562611620312));
#53639=CARTESIAN_POINT('Ctrl Pts',(111.442118957974,-11.5905169200521,-7.0805895974353));
#53640=CARTESIAN_POINT('Ctrl Pts',(111.601143216421,-5.92253722030125,-11.7533730996655));
#53641=CARTESIAN_POINT('Ctrl Pts',(111.696557771489,-1.77635679506652,-12.5649803570316));
#53642=CARTESIAN_POINT('Ctrl Pts',(111.728362623178,-0.387674889596971,
-12.6076810805785));
#53643=CARTESIAN_POINT('',(110.294852708433,-2.05149138653157,11.4148109645546));
#53644=CARTESIAN_POINT('',(110.869631627566,-1.72165885261005,12.4955914163688));
#53645=CARTESIAN_POINT('Ctrl Pts',(110.294852708433,-2.05151014872391,11.4148181175828));
#53646=CARTESIAN_POINT('Ctrl Pts',(110.295777713638,-2.05115143980387,11.4165390179275));
#53647=CARTESIAN_POINT('Ctrl Pts',(110.296702621574,-2.05079204924444,11.4182598296616));
#53648=CARTESIAN_POINT('Ctrl Pts',(110.297627431306,-2.05043197673464,11.4199805509081));
#53649=CARTESIAN_POINT('Ctrl Pts',(110.362289477104,-2.02525596017536,11.5402921698508));
#53650=CARTESIAN_POINT('Ctrl Pts',(110.426669089208,-1.99667407529724,11.6605286357912));
#53651=CARTESIAN_POINT('Ctrl Pts',(110.490401576393,-1.96452355069117,11.7799729158333));
#53652=CARTESIAN_POINT('Ctrl Pts',(110.52225910097,-1.94845268678713,11.8396787151069));
#53653=CARTESIAN_POINT('Ctrl Pts',(110.553954932835,-1.93149088670665,11.8991863079254));
#53654=CARTESIAN_POINT('Ctrl Pts',(110.585443522995,-1.91362250664267,11.9584045796434));
#53655=CARTESIAN_POINT('Ctrl Pts',(110.642821112822,-1.88106326607426,12.0663103857662));
#53656=CARTESIAN_POINT('Ctrl Pts',(110.69991007705,-1.8452663989536,12.1740075423432));
#53657=CARTESIAN_POINT('Ctrl Pts',(110.756284866846,-1.80604384761692,12.2806792435686));
#53658=CARTESIAN_POINT('Ctrl Pts',(110.794438206198,-1.77949880298167,12.3528725347709));
#53659=CARTESIAN_POINT('Ctrl Pts',(110.832264431244,-1.75138558612517,12.4245957776382));
#53660=CARTESIAN_POINT('Ctrl Pts',(110.869631627566,-1.72165885260991,12.4955914163688));
#53661=CARTESIAN_POINT('',(111.113306560609,-1.49574126823376,-11.5007830876033));
#53662=CARTESIAN_POINT('Ctrl Pts',(110.294852708433,-2.05151014872383,11.4148181175829));
#53663=CARTESIAN_POINT('Ctrl Pts',(110.322721242001,-3.15372498702172,11.2170597406403));
#53664=CARTESIAN_POINT('Ctrl Pts',(110.414199478948,-6.68304601222112,10.047541268463));
#53665=CARTESIAN_POINT('Ctrl Pts',(110.537482567584,-10.3238350595526,6.31146214230268));
#53666=CARTESIAN_POINT('Ctrl Pts',(110.696506826031,-12.0956797652182,0.0747112542218324));
#53667=CARTESIAN_POINT('Ctrl Pts',(110.855531084478,-10.6569271560527,-6.51026421705393));
#53668=CARTESIAN_POINT('Ctrl Pts',(111.005065946567,-5.75647048603604,-10.5502880516584));
#53669=CARTESIAN_POINT('Ctrl Pts',(111.090991105277,-2.3847793900036,-11.3863505147081));
#53670=CARTESIAN_POINT('Ctrl Pts',(111.113306560609,-1.49583592206305,-11.5012322968872));
#53671=CARTESIAN_POINT('',(111.666163538309,-0.384363792912494,-12.5));
#53672=CARTESIAN_POINT('Ctrl Pts',(111.666163538309,-0.384363792912482,
-12.5));
#53673=CARTESIAN_POINT('Ctrl Pts',(111.665943629296,-0.385603136713582,
-12.4996308352661));
#53674=CARTESIAN_POINT('Ctrl Pts',(111.665722752094,-0.3868417540112,-12.4992598048037));
#53675=CARTESIAN_POINT('Ctrl Pts',(111.646927229217,-0.491721570729726,
-12.4676667904319));
#53676=CARTESIAN_POINT('Ctrl Pts',(111.621715678588,-0.589568826402512,
-12.4236261787122));
#53677=CARTESIAN_POINT('Ctrl Pts',(111.547301296044,-0.818118357277709,
-12.2914776069231));
#53678=CARTESIAN_POINT('Ctrl Pts',(111.492284046241,-0.941416122263338,
-12.192147571922));
#53679=CARTESIAN_POINT('Ctrl Pts',(111.337452105661,-1.22626137196524,-11.9109461347845));
#53680=CARTESIAN_POINT('Ctrl Pts',(111.226277414691,-1.37389090285344,-11.7075353508788));
#53681=CARTESIAN_POINT('Ctrl Pts',(111.113306560609,-1.49574126823374,-11.5007830876033));
#53682=CARTESIAN_POINT('',(111.698449331144,-1.68935314531931,-12.5));
#53683=CARTESIAN_POINT('Ctrl Pts',(111.698449331144,-1.68946588589014,-12.5005399240113));
#53684=CARTESIAN_POINT('Ctrl Pts',(111.697947425979,-1.68027860774559,-12.5005322965039));
#53685=CARTESIAN_POINT('Ctrl Pts',(111.697451254675,-1.67109103740135,-12.5005247411879));
#53686=CARTESIAN_POINT('Ctrl Pts',(111.696960821607,-1.66190315994946,-12.5005172591199));
#53687=CARTESIAN_POINT('Ctrl Pts',(111.683767253214,-1.41473204240369,-12.5003159774741));
#53688=CARTESIAN_POINT('Ctrl Pts',(111.67474429422,-1.16766800271047,-12.5001701868406));
#53689=CARTESIAN_POINT('Ctrl Pts',(111.669942717737,-0.920412235438467,
-12.5000872409516));
#53690=CARTESIAN_POINT('Ctrl Pts',(111.667814925534,-0.810842202392649,
-12.5000504839372));
#53691=CARTESIAN_POINT('Ctrl Pts',(111.666516115962,-0.701233850372462,
-12.5000258236701));
#53692=CARTESIAN_POINT('Ctrl Pts',(111.666050707469,-0.591558293419319,
-12.5000124326105));
#53693=CARTESIAN_POINT('Ctrl Pts',(111.665757586238,-0.522482986818619,
-12.5000039987208));
#53694=CARTESIAN_POINT('Ctrl Pts',(111.665795205982,-0.45342049399712,-12.4999999999378));
#53695=CARTESIAN_POINT('Ctrl Pts',(111.666163538309,-0.384363792912482,
-12.5));
#53696=CARTESIAN_POINT('Ctrl Pts',(110.869631627566,-1.72165885260965,12.4955914163688));
#53697=CARTESIAN_POINT('Ctrl Pts',(110.901436479255,-3.09799456313,12.3059580904043));
#53698=CARTESIAN_POINT('Ctrl Pts',(110.933241330945,-4.44602202169452,11.889800817738));
#53699=CARTESIAN_POINT('Ctrl Pts',(110.965046182634,-5.68522096696964,11.2629364182439));
#53700=CARTESIAN_POINT('Ctrl Pts',(111.028655886013,-8.16361885751988,10.0092076192556));
#53701=CARTESIAN_POINT('Ctrl Pts',(111.092265589392,-10.2067026949125,7.91265031295602));
#53702=CARTESIAN_POINT('Ctrl Pts',(111.15587529277,-11.4016147585863,5.40496710455104));
#53703=CARTESIAN_POINT('Ctrl Pts',(111.18768014446,-11.9990707904232,4.15112550034857));
#53704=CARTESIAN_POINT('Ctrl Pts',(111.219484996149,-12.3844838788303,2.79450242061976));
#53705=CARTESIAN_POINT('Ctrl Pts',(111.251289847838,-12.5371063953956,1.41263064356073));
#53706=CARTESIAN_POINT('Ctrl Pts',(111.314899551217,-12.8423514285262,-1.35111291055738));
#53707=CARTESIAN_POINT('Ctrl Pts',(111.378509254595,-12.2164341742891,-4.21585125399633));
#53708=CARTESIAN_POINT('Ctrl Pts',(111.442118957974,-10.7698796072204,-6.58277712616185));
#53709=CARTESIAN_POINT('Ctrl Pts',(111.505728661353,-9.32332504015176,-8.94970299832736));
#53710=CARTESIAN_POINT('Ctrl Pts',(111.569338364732,-7.05613316025142,-10.8188163992194));
#53711=CARTESIAN_POINT('Ctrl Pts',(111.63294806811,-4.45765567795809,-11.802568536124));
#53712=CARTESIAN_POINT('Ctrl Pts',(111.654781822455,-3.5657395707398,-12.1402371833971));
#53713=CARTESIAN_POINT('Ctrl Pts',(111.6766155768,-2.63479219550788,-12.3735947089856));
#53714=CARTESIAN_POINT('Ctrl Pts',(111.698449331144,-1.68946588589041,-12.5005399240113));
#53715=CARTESIAN_POINT('Ctrl Pts',(111.15742112713,0.271901404433829,-11.5944522594156));
#53716=CARTESIAN_POINT('Ctrl Pts',(111.204610057985,2.16670657813642,-11.5500171988943));
#53717=CARTESIAN_POINT('Ctrl Pts',(111.298987919696,5.93235416102211,-10.5144384800968));
#53718=CARTESIAN_POINT('Ctrl Pts',(111.440554712261,10.1848431574681,-6.48215877251662));
#53719=CARTESIAN_POINT('Ctrl Pts',(111.582121504826,12.0371931123728,-0.923170511755194));
#53720=CARTESIAN_POINT('Ctrl Pts',(111.723688297391,11.0540455303336,4.85356472268307));
#53721=CARTESIAN_POINT('Ctrl Pts',(111.865255089956,7.46653539266892,9.48674646633624));
#53722=CARTESIAN_POINT('Ctrl Pts',(112.006821882522,2.12006530550471,11.8850101815537));
#53723=CARTESIAN_POINT('Ctrl Pts',(112.148388675087,-3.72590191992946,11.4832747896718));
#53724=CARTESIAN_POINT('Ctrl Pts',(112.289955467652,-8.69407282986275,8.37622032266638));
#53725=CARTESIAN_POINT('Ctrl Pts',(112.431522260217,-11.6140252170778,3.29581715585153));
#53726=CARTESIAN_POINT('Ctrl Pts',(112.573089052782,-11.7978403519213,-2.56104100542157));
#53727=CARTESIAN_POINT('Ctrl Pts',(112.714655845348,-9.20221848328371,-7.81454784931888));
#53728=CARTESIAN_POINT('Ctrl Pts',(112.856222637913,-4.43865660418402,-11.2270344946451));
#53729=CARTESIAN_POINT('Ctrl Pts',(112.997789430478,1.37060254033464,-11.9945582342283));
#53730=CARTESIAN_POINT('Ctrl Pts',(113.139356223043,6.85696329237368,-9.9362987275659));
#53731=CARTESIAN_POINT('Ctrl Pts',(113.280923015609,10.7279004735232,-5.53715895830823));
#53732=CARTESIAN_POINT('Ctrl Pts',(113.422489808174,12.0714648968156,0.166473261964394));
#53733=CARTESIAN_POINT('Ctrl Pts',(113.564056600739,10.5711278304476,5.83088624039759));
#53734=CARTESIAN_POINT('Ctrl Pts',(113.705623393304,6.58035185125043,10.1216079525872));
#53735=CARTESIAN_POINT('Ctrl Pts',(113.847190185869,1.03931892093069,12.0277925731204));
#53736=CARTESIAN_POINT('Ctrl Pts',(113.988756978435,-4.74656586578709,11.1003644305775));
#53737=CARTESIAN_POINT('Ctrl Pts',(114.130323771,-9.41421307630654,7.55781517133264));
#53738=CARTESIAN_POINT('Ctrl Pts',(114.271890563565,-11.8639774806702,2.23472959112623));
#53739=CARTESIAN_POINT('Ctrl Pts',(114.41345735613,-11.5187221158893,-3.61483316724977));
#53740=CARTESIAN_POINT('Ctrl Pts',(114.555024148696,-8.45978526537628,-8.6127818545234));
#53741=CARTESIAN_POINT('Ctrl Pts',(114.696590941261,-3.40781807628825,-11.581655924795));
#53742=CARTESIAN_POINT('Ctrl Pts',(114.838157733826,2.44699275634759,-11.8220220132816));
#53743=CARTESIAN_POINT('Ctrl Pts',(114.979724526391,7.72531959196485,-9.2772525651793));
#53744=CARTESIAN_POINT('Ctrl Pts',(115.121291318956,11.1836479525214,-4.54686667674157));
#53745=CARTESIAN_POINT('Ctrl Pts',(115.262858111522,12.0072345239343,1.25470992130988));
#53746=CARTESIAN_POINT('Ctrl Pts',(115.404424904087,10.0020516002354,6.76069092494371));
#53747=CARTESIAN_POINT('Ctrl Pts',(115.545991696652,5.64049766960815,10.6739292014239));
#53748=CARTESIAN_POINT('Ctrl Pts',(115.687558489217,-0.0498940161182073,
12.0725095394857));
#53749=CARTESIAN_POINT('Ctrl Pts',(115.829125281783,-5.72853146574744,10.6269426623712));
#53750=CARTESIAN_POINT('Ctrl Pts',(115.970692074348,-10.0575907787097,6.67778673879954));
#53751=CARTESIAN_POINT('Ctrl Pts',(116.112258866913,-12.0171957981701,1.15542096924257));
#53752=CARTESIAN_POINT('Ctrl Pts',(116.253825659478,-11.1456822477808,-4.63915256230159));
#53753=CARTESIAN_POINT('Ctrl Pts',(116.395392452043,-7.64837610766902,-9.34078625853751));
#53754=CARTESIAN_POINT('Ctrl Pts',(116.536959244609,-2.34918804318456,-11.8418520279979));
#53755=CARTESIAN_POINT('Ctrl Pts',(116.678526037174,3.50341987815323,-11.5530757135873));
#53756=CARTESIAN_POINT('Ctrl Pts',(116.820092829739,8.53070918247288,-8.54259995247553));
#53757=CARTESIAN_POINT('Ctrl Pts',(116.961659622304,11.5481555073598,-3.51942696985816));
#53758=CARTESIAN_POINT('Ctrl Pts',(117.103226414869,11.8451994508802,2.33252276799301));
#53759=CARTESIAN_POINT('Ctrl Pts',(117.244793207435,9.35114240419514,7.63559939886844));
#53760=CARTESIAN_POINT('Ctrl Pts',(117.339171069145,6.22031361682587,9.97021630652136));
#53761=CARTESIAN_POINT('Ctrl Pts',(117.38636,4.47152467205382,10.7009682121205));
#53762=CARTESIAN_POINT('Ctrl Pts',(111.352950418296,0.279841290678049,-11.9330258397752));
#53763=CARTESIAN_POINT('Ctrl Pts',(111.400139349151,2.22997732067215,-11.8872932157988));
#53764=CARTESIAN_POINT('Ctrl Pts',(111.494517210861,6.10558687122862,-10.8214742073591));
#53765=CARTESIAN_POINT('Ctrl Pts',(111.636084003426,10.4822542585768,-6.67144651591031));
#53766=CARTESIAN_POINT('Ctrl Pts',(111.777650795992,12.3886953203557,-0.950128330758139));
#53767=CARTESIAN_POINT('Ctrl Pts',(111.919217588557,11.3768385082963,4.99529533219344));
#53768=CARTESIAN_POINT('Ctrl Pts',(112.060784381122,7.68456825564656,9.76377220633729));
#53769=CARTESIAN_POINT('Ctrl Pts',(112.202351173687,2.18197406022818,12.2320684435351));
#53770=CARTESIAN_POINT('Ctrl Pts',(112.343917966252,-3.83470326085307,11.8186018385745));
#53771=CARTESIAN_POINT('Ctrl Pts',(112.485484758818,-8.94795143491056,8.62081720754495));
#53772=CARTESIAN_POINT('Ctrl Pts',(112.627051551383,-11.9531703540927,3.39205944394766));
#53773=CARTESIAN_POINT('Ctrl Pts',(112.768618343948,-12.1423531377856,-2.6358268429284));
#53774=CARTESIAN_POINT('Ctrl Pts',(112.910185136513,-9.47093562398407,-8.04274314350251));
#53775=CARTESIAN_POINT('Ctrl Pts',(113.051751929078,-4.56827133930403,-11.5548789827352));
#53776=CARTESIAN_POINT('Ctrl Pts',(113.193318721644,1.41062597559042,-12.3448154464995));
#53777=CARTESIAN_POINT('Ctrl Pts',(113.334885514209,7.05719583120776,-10.2264519974613));
#53778=CARTESIAN_POINT('Ctrl Pts',(113.476452306774,11.0411695777288,-5.69885143774489));
#53779=CARTESIAN_POINT('Ctrl Pts',(113.618019099339,12.4239678869401,0.171334504830907));
#53780=CARTESIAN_POINT('Ctrl Pts',(113.759585891905,10.8798189628888,6.00115595102388));
#53781=CARTESIAN_POINT('Ctrl Pts',(113.90115268447,6.77250696444217,10.417172500772));
#53782=CARTESIAN_POINT('Ctrl Pts',(114.042719477035,1.06966842949927,12.3790202727297));
#53783=CARTESIAN_POINT('Ctrl Pts',(114.1842862696,-4.88517196494861,11.4245099826457));
#53784=CARTESIAN_POINT('Ctrl Pts',(114.325853062165,-9.6891207438874,7.7785135264599));
#53785=CARTESIAN_POINT('Ctrl Pts',(114.467419854731,-12.2104215595334,2.299986697014));
#53786=CARTESIAN_POINT('Ctrl Pts',(114.608986647296,-11.8550842743326,-3.72039115140071));
#53787=CARTESIAN_POINT('Ctrl Pts',(114.750553439861,-8.70682235883157,-8.86428665389625));
#53788=CARTESIAN_POINT('Ctrl Pts',(114.892120232426,-3.50733094170769,-11.9198558349948));
#53789=CARTESIAN_POINT('Ctrl Pts',(115.033687024992,2.51844823178479,-12.1672409361399));
#53790=CARTESIAN_POINT('Ctrl Pts',(115.175253817557,7.95090930117684,-9.54816080186144));
#53791=CARTESIAN_POINT('Ctrl Pts',(115.316820610122,11.510225495302,-4.67964129133471));
#53792=CARTESIAN_POINT('Ctrl Pts',(115.458387402687,12.3578619008925,1.29134913641601));
#53793=CARTESIAN_POINT('Ctrl Pts',(115.599954195252,10.294124942336,6.95811218132984));
#53794=CARTESIAN_POINT('Ctrl Pts',(115.741520987818,5.80520777822571,10.9856222719867));
#53795=CARTESIAN_POINT('Ctrl Pts',(115.883087780383,-0.0513509884095631,
12.4250430345795));
#53796=CARTESIAN_POINT('Ctrl Pts',(116.024654572948,-5.89581227946469,10.9372636628784));
#53797=CARTESIAN_POINT('Ctrl Pts',(116.166221365513,-10.3512859394254,6.87278708158827));
#53798=CARTESIAN_POINT('Ctrl Pts',(116.307788158079,-12.3681140577166,1.1891608135773));
#53799=CARTESIAN_POINT('Ctrl Pts',(116.449354950644,-11.4711511409851,-4.77462204871715));
#53800=CARTESIAN_POINT('Ctrl Pts',(116.590921743209,-7.87171896378435,-9.61354976440806));
#53801=CARTESIAN_POINT('Ctrl Pts',(116.732488535774,-2.4177874896201,-12.1876500139228));
#53802=CARTESIAN_POINT('Ctrl Pts',(116.874055328339,3.60572444460535,-11.8904410432293));
#53803=CARTESIAN_POINT('Ctrl Pts',(117.015622120905,8.77981734957677,-8.79205534603593));
#53804=CARTESIAN_POINT('Ctrl Pts',(117.15718891347,11.8853771603708,-3.6221989648898));
#53805=CARTESIAN_POINT('Ctrl Pts',(117.298755706035,12.1910951860497,2.40063556600711));
#53806=CARTESIAN_POINT('Ctrl Pts',(117.4403224986,9.62420832342993,7.8585691579243));
#53807=CARTESIAN_POINT('Ctrl Pts',(117.53470036031,6.4019551299468,10.2613600152824));
#53808=CARTESIAN_POINT('Ctrl Pts',(117.581889291165,4.60209919890604,11.0134508581162));
#53809=CARTESIAN_POINT('Ctrl Pts',(111.548479709461,0.287781176922269,-12.2715994201348));
#53810=CARTESIAN_POINT('Ctrl Pts',(111.595668640316,2.29324806320787,-12.2245692327033));
#53811=CARTESIAN_POINT('Ctrl Pts',(111.690046502027,6.27881958143513,-11.1285099346214));
#53812=CARTESIAN_POINT('Ctrl Pts',(111.831613294592,10.7796653596855,-6.86073425930401));
#53813=CARTESIAN_POINT('Ctrl Pts',(111.973180087157,12.7401975283385,-0.977086149761075));
#53814=CARTESIAN_POINT('Ctrl Pts',(112.114746879722,11.6996314862591,5.13702594170381));
#53815=CARTESIAN_POINT('Ctrl Pts',(112.256313672287,7.9026011186242,10.0407979463383));
#53816=CARTESIAN_POINT('Ctrl Pts',(112.397880464853,2.24388281495165,12.5791267055165));
#53817=CARTESIAN_POINT('Ctrl Pts',(112.539447257418,-3.94350460177667,12.1539288874771));
#53818=CARTESIAN_POINT('Ctrl Pts',(112.681014049983,-9.20183003995837,8.86541409242353));
#53819=CARTESIAN_POINT('Ctrl Pts',(112.822580842548,-12.2923154911077,3.4883017320438));
#53820=CARTESIAN_POINT('Ctrl Pts',(112.964147635114,-12.4868659236498,-2.71061268043522));
#53821=CARTESIAN_POINT('Ctrl Pts',(113.105714427679,-9.73965276468443,-8.27093843768614));
#53822=CARTESIAN_POINT('Ctrl Pts',(113.247281220244,-4.69788607442404,-11.8827234708253));
#53823=CARTESIAN_POINT('Ctrl Pts',(113.388848012809,1.4506494108462,-12.6950726587707));
#53824=CARTESIAN_POINT('Ctrl Pts',(113.530414805374,7.25742837004184,-10.5166052673566));
#53825=CARTESIAN_POINT('Ctrl Pts',(113.67198159794,11.3544386819345,-5.86054391718156));
#53826=CARTESIAN_POINT('Ctrl Pts',(113.813548390505,12.7764708770647,0.176195747697426));
#53827=CARTESIAN_POINT('Ctrl Pts',(113.95511518307,11.1885100953299,6.17142566165016));
#53828=CARTESIAN_POINT('Ctrl Pts',(114.096681975635,6.96466207763389,10.7127370489567));
#53829=CARTESIAN_POINT('Ctrl Pts',(114.238248768201,1.10001793806786,12.730247972339));
#53830=CARTESIAN_POINT('Ctrl Pts',(114.379815560766,-5.02377806411015,11.748655534714));
#53831=CARTESIAN_POINT('Ctrl Pts',(114.521382353331,-9.96402841146824,7.99921188158716));
#53832=CARTESIAN_POINT('Ctrl Pts',(114.662949145896,-12.5568656383966,2.36524380290177));
#53833=CARTESIAN_POINT('Ctrl Pts',(114.804515938461,-12.1914464327759,-3.82594913555166));
#53834=CARTESIAN_POINT('Ctrl Pts',(114.946082731027,-8.95385945228687,-9.11579145326909));
#53835=CARTESIAN_POINT('Ctrl Pts',(115.087649523592,-3.60684380712713,-12.2580557451947));
#53836=CARTESIAN_POINT('Ctrl Pts',(115.229216316157,2.589903707222,-12.5124598589981));
#53837=CARTESIAN_POINT('Ctrl Pts',(115.370783108722,8.17649901038882,-9.81906903854357));
#53838=CARTESIAN_POINT('Ctrl Pts',(115.512349901287,11.8368030380826,-4.81241590592785));
#53839=CARTESIAN_POINT('Ctrl Pts',(115.653916693853,12.7084892778507,1.32798835152213));
#53840=CARTESIAN_POINT('Ctrl Pts',(115.795483486418,10.5861982844366,7.15553343771598));
#53841=CARTESIAN_POINT('Ctrl Pts',(115.937050278983,5.96991788684329,11.2973153425495));
#53842=CARTESIAN_POINT('Ctrl Pts',(116.078617071548,-0.0528079607009308,
12.7775765296732));
#53843=CARTESIAN_POINT('Ctrl Pts',(116.220183864114,-6.06309309318193,11.2475846633857));
#53844=CARTESIAN_POINT('Ctrl Pts',(116.361750656679,-10.6449811001411,7.06778742437699));
#53845=CARTESIAN_POINT('Ctrl Pts',(116.503317449244,-12.7190323172631,1.22290065791204));
#53846=CARTESIAN_POINT('Ctrl Pts',(116.644884241809,-11.7966200341894,-4.91009153513272));
#53847=CARTESIAN_POINT('Ctrl Pts',(116.786451034374,-8.09506181989969,-9.88631327027862));
#53848=CARTESIAN_POINT('Ctrl Pts',(116.92801782694,-2.48638693605563,-12.5334479998476));
#53849=CARTESIAN_POINT('Ctrl Pts',(117.069584619505,3.70802901105746,-12.2278063728712));
#53850=CARTESIAN_POINT('Ctrl Pts',(117.21115141207,9.02892551668066,-9.04151073959632));
#53851=CARTESIAN_POINT('Ctrl Pts',(117.352718204635,12.2225988133817,-3.72497095992145));
#53852=CARTESIAN_POINT('Ctrl Pts',(117.494284997201,12.5369909212193,2.46874836402119));
#53853=CARTESIAN_POINT('Ctrl Pts',(117.635851789766,9.89727424266471,8.08153891698017));
#53854=CARTESIAN_POINT('Ctrl Pts',(117.730229651476,6.58359664306774,10.5525037240434));
#53855=CARTESIAN_POINT('Ctrl Pts',(117.777418582331,4.73267372575826,11.3259335041118));
#53856=CARTESIAN_POINT('Ctrl Pts',(111.744009000627,0.295721063166489,-12.6101730004945));
#53857=CARTESIAN_POINT('Ctrl Pts',(111.791197931482,2.3565188057436,-12.5618452496078));
#53858=CARTESIAN_POINT('Ctrl Pts',(111.885575793192,6.45205229164162,-11.4355456618837));
#53859=CARTESIAN_POINT('Ctrl Pts',(112.027142585757,11.0770764607942,-7.05002200269771));
#53860=CARTESIAN_POINT('Ctrl Pts',(112.168709378323,13.0916997363214,-1.00404396876402));
#53861=CARTESIAN_POINT('Ctrl Pts',(112.310276170888,12.0224244642218,5.27875655121417));
#53862=CARTESIAN_POINT('Ctrl Pts',(112.451842963453,8.12063398160184,10.3178236863394));
#53863=CARTESIAN_POINT('Ctrl Pts',(112.593409756018,2.30579156967512,12.9261849674979));
#53864=CARTESIAN_POINT('Ctrl Pts',(112.734976548583,-4.05230594270028,12.4892559363798));
#53865=CARTESIAN_POINT('Ctrl Pts',(112.876543341149,-9.45570864500619,9.1100109773021));
#53866=CARTESIAN_POINT('Ctrl Pts',(113.018110133714,-12.6314606281227,3.58454402013992));
#53867=CARTESIAN_POINT('Ctrl Pts',(113.159676926279,-12.8313787095141,-2.78539851794204));
#53868=CARTESIAN_POINT('Ctrl Pts',(113.301243718844,-10.0083699053848,-8.49913373186977));
#53869=CARTESIAN_POINT('Ctrl Pts',(113.44281051141,-4.82750080954404,-12.2105679589154));
#53870=CARTESIAN_POINT('Ctrl Pts',(113.584377303975,1.49067284610198,-13.045329871042));
#53871=CARTESIAN_POINT('Ctrl Pts',(113.72594409654,7.45766090887593,-10.8067585372519));
#53872=CARTESIAN_POINT('Ctrl Pts',(113.867510889105,11.6677077861402,-6.02223639661823));
#53873=CARTESIAN_POINT('Ctrl Pts',(114.00907768167,13.1289738671892,0.18105699056394));
#53874=CARTESIAN_POINT('Ctrl Pts',(114.150644474236,11.4972012277711,6.34169537227645));
#53875=CARTESIAN_POINT('Ctrl Pts',(114.292211266801,7.15681719082563,11.0083015971415));
#53876=CARTESIAN_POINT('Ctrl Pts',(114.433778059366,1.13036744663645,13.0814756719483));
#53877=CARTESIAN_POINT('Ctrl Pts',(114.575344851931,-5.16238416327168,12.0728010867823));
#53878=CARTESIAN_POINT('Ctrl Pts',(114.716911644497,-10.2389360790491,8.21991023671442));
#53879=CARTESIAN_POINT('Ctrl Pts',(114.858478437062,-12.9033097172598,2.43050090878955));
#53880=CARTESIAN_POINT('Ctrl Pts',(115.000045229627,-12.5278085912191,-3.93150711970261));
#53881=CARTESIAN_POINT('Ctrl Pts',(115.141612022192,-9.20089654574217,-9.36729625264193));
#53882=CARTESIAN_POINT('Ctrl Pts',(115.283178814757,-3.70635667254657,-12.5962556553946));
#53883=CARTESIAN_POINT('Ctrl Pts',(115.424745607323,2.6613591826592,-12.8576787818564));
#53884=CARTESIAN_POINT('Ctrl Pts',(115.566312399888,8.4020887196008,-10.0899772752257));
#53885=CARTESIAN_POINT('Ctrl Pts',(115.707879192453,12.1633805808632,-4.94519052052099));
#53886=CARTESIAN_POINT('Ctrl Pts',(115.849445985018,13.0591166548089,1.36462756662826));
#53887=CARTESIAN_POINT('Ctrl Pts',(115.991012777583,10.8782716265372,7.35295469410212));
#53888=CARTESIAN_POINT('Ctrl Pts',(116.132579570149,6.13462799546086,11.6090084131123));
#53889=CARTESIAN_POINT('Ctrl Pts',(116.274146362714,-0.0542649329922895,
13.130110024767));
#53890=CARTESIAN_POINT('Ctrl Pts',(116.415713155279,-6.23037390689917,11.557905663893));
#53891=CARTESIAN_POINT('Ctrl Pts',(116.557279947844,-10.9386762608569,7.26278776716572));
#53892=CARTESIAN_POINT('Ctrl Pts',(116.69884674041,-13.0699505768096,1.25664050224678));
#53893=CARTESIAN_POINT('Ctrl Pts',(116.840413532975,-12.1220889273937,-5.04556102154829));
#53894=CARTESIAN_POINT('Ctrl Pts',(116.98198032554,-8.31840467601501,-10.1590767761492));
#53895=CARTESIAN_POINT('Ctrl Pts',(117.123547118105,-2.55498638249118,-12.8792459857725));
#53896=CARTESIAN_POINT('Ctrl Pts',(117.26511391067,3.81033357750957,-12.5651717025131));
#53897=CARTESIAN_POINT('Ctrl Pts',(117.406680703236,9.27803368378454,-9.29096613315673));
#53898=CARTESIAN_POINT('Ctrl Pts',(117.548247495801,12.5598204663927,-3.82774295495309));
#53899=CARTESIAN_POINT('Ctrl Pts',(117.689814288366,12.8828866563888,2.53686116203528));
#53900=CARTESIAN_POINT('Ctrl Pts',(117.831381080931,10.1703401618995,8.30450867603603));
#53901=CARTESIAN_POINT('Ctrl Pts',(117.925758942641,6.76523815618867,10.8436474328044));
#53902=CARTESIAN_POINT('Ctrl Pts',(117.972947873497,4.86324825261048,11.6384161501074));
#53903=CARTESIAN_POINT('',(117.141306474002,-1.68935314531914,-12.5));
#53904=CARTESIAN_POINT('',(117.218885227957,1.68935314531925,-12.5));
#53905=CARTESIAN_POINT('Ctrl Pts',(117.141306474002,-1.68966005362616,-12.500608264671));
#53906=CARTESIAN_POINT('Ctrl Pts',(117.140804568838,-1.68047463572448,-12.5006004763374));
#53907=CARTESIAN_POINT('Ctrl Pts',(117.140308397533,-1.67128889071667,-12.5005926219721));
#53908=CARTESIAN_POINT('Ctrl Pts',(117.139817964464,-1.66210280379621,-12.5005847053769));
#53909=CARTESIAN_POINT('Ctrl Pts',(117.126559275382,-1.41376010819252,-12.5003706829534));
#53910=CARTESIAN_POINT('Ctrl Pts',(117.117512467812,-1.16550008733763,-12.5001134860496));
#53911=CARTESIAN_POINT('Ctrl Pts',(117.112729070399,-0.917020752225694,
-12.4998770325662));
#53912=CARTESIAN_POINT('Ctrl Pts',(117.110643239224,-0.808669741663733,
-12.4997739255056));
#53913=CARTESIAN_POINT('Ctrl Pts',(117.10936807505,-0.700276366307754,-12.4996745527923));
#53914=CARTESIAN_POINT('Ctrl Pts',(117.108907850327,-0.591812800653879,
-12.4995829446679));
#53915=CARTESIAN_POINT('Ctrl Pts',(117.10815486932,-0.414353831801932,-12.4994330631552));
#53916=CARTESIAN_POINT('Ctrl Pts',(117.109584424463,-0.236967696978893,
-12.4993044175444));
#53917=CARTESIAN_POINT('Ctrl Pts',(117.113196032071,-0.0595349787923405,
-12.4992090581988));
#53918=CARTESIAN_POINT('Ctrl Pts',(117.113465330855,-0.0463047443763591,
-12.4992019477487));
#53919=CARTESIAN_POINT('Ctrl Pts',(117.113746751044,-0.0330747720332224,
-12.4991950195628));
#53920=CARTESIAN_POINT('Ctrl Pts',(117.114040289568,-0.0198450123812237,
-12.4991882770983));
#53921=CARTESIAN_POINT('Ctrl Pts',(117.114120941615,-0.0162100305813574,
-12.4991864245525));
#53922=CARTESIAN_POINT('Ctrl Pts',(117.114202508421,-0.0125750683061462,
-12.4991845860277));
#53923=CARTESIAN_POINT('Ctrl Pts',(117.114284989917,-0.00894012455784924,
-12.4991827615927));
#53924=CARTESIAN_POINT('Ctrl Pts',(117.114333443178,-0.00680479866143413,
-12.4991816898394));
#53925=CARTESIAN_POINT('Ctrl Pts',(117.11438221208,-0.00466947955864029,
-12.4991806229485));
#53926=CARTESIAN_POINT('Ctrl Pts',(117.114431296611,-0.00253416694871591,
-12.4991795609337));
#53927=CARTESIAN_POINT('Ctrl Pts',(117.114473674849,-0.000690596637058661,
-12.4991786440194));
#53928=CARTESIAN_POINT('Ctrl Pts',(117.114516288354,0.00115296855477631,
-12.4991777307399));
#53929=CARTESIAN_POINT('Ctrl Pts',(117.114559137117,0.00299652874669277,
-12.499176821104));
#53930=CARTESIAN_POINT('Ctrl Pts',(117.114611320797,0.00524172200240544,
-12.4991757132974));
#53931=CARTESIAN_POINT('Ctrl Pts',(117.114663853399,0.00748690754199927,
-12.4991746108951));
#53932=CARTESIAN_POINT('Ctrl Pts',(117.114716734904,0.00973208555912489,
-12.4991735139129));
#53933=CARTESIAN_POINT('Ctrl Pts',(117.11481650341,0.0139679342504296,-12.4991714442994));
#53934=CARTESIAN_POINT('Ctrl Pts',(117.114917513772,0.0182037545289113,
-12.499169393979));
#53935=CARTESIAN_POINT('Ctrl Pts',(117.115019765873,0.0224395480908287,
-12.4991673630552));
#53936=CARTESIAN_POINT('Ctrl Pts',(117.115602197855,0.0465667943806478,
-12.4991557948337));
#53937=CARTESIAN_POINT('Ctrl Pts',(117.116224911658,0.070692915173029,-12.4991448562447));
#53938=CARTESIAN_POINT('Ctrl Pts',(117.116887882688,0.0948182088186656,
-12.4991345650034));
#53939=CARTESIAN_POINT('Ctrl Pts',(117.117735535906,0.125664025393719,-12.4991214069566));
#53940=CARTESIAN_POINT('Ctrl Pts',(117.118648976774,0.15650768043098,-12.4991093076991));
#53941=CARTESIAN_POINT('Ctrl Pts',(117.119628143454,0.187349795104028,-12.4990982985367));
#53942=CARTESIAN_POINT('Ctrl Pts',(117.124449939474,0.339228314825474,-12.4990440851568));
#53943=CARTESIAN_POINT('Ctrl Pts',(117.130863523257,0.491005283256536,-12.4990166205082));
#53944=CARTESIAN_POINT('Ctrl Pts',(117.13885739767,0.642753325474625,-12.4990173756166));
#53945=CARTESIAN_POINT('Ctrl Pts',(117.151510948311,0.882956190529511,-12.4990185708822));
#53946=CARTESIAN_POINT('Ctrl Pts',(117.168102434924,1.12266909663543,-12.4990921998159));
#53947=CARTESIAN_POINT('Ctrl Pts',(117.188543046603,1.36216112185186,-12.4992236134943));
#53948=CARTESIAN_POINT('Ctrl Pts',(117.197860187627,1.47132522163686,-12.4992835138434));
#53949=CARTESIAN_POINT('Ctrl Pts',(117.207977051648,1.58044277825126,-12.4993551794546));
#53950=CARTESIAN_POINT('Ctrl Pts',(117.218885227957,1.68953572661318,-12.499436378717));
#53951=CARTESIAN_POINT('',(115.404599513671,1.68935314531934,-12.5));
#53952=CARTESIAN_POINT('Ctrl Pts',(115.404599513671,1.6896686969101,-12.5005137686862));
#53953=CARTESIAN_POINT('Ctrl Pts',(115.411314878222,1.98036881708519,-12.4614884428392));
#53954=CARTESIAN_POINT('Ctrl Pts',(115.418030242772,2.26967326198219,-12.4122686062437));
#53955=CARTESIAN_POINT('Ctrl Pts',(115.424745607323,2.55686146294845,-12.352824676341));
#53956=CARTESIAN_POINT('Ctrl Pts',(115.471934538178,4.57493569497303,-11.9351116129795));
#53957=CARTESIAN_POINT('Ctrl Pts',(115.519123469033,6.48851220728691,-11.0125444441026));
#53958=CARTESIAN_POINT('Ctrl Pts',(115.566312399888,8.07218244032092,-9.69379640054671));
#53959=CARTESIAN_POINT('Ctrl Pts',(115.613501330743,9.65585267335493,-8.3750483569908));
#53960=CARTESIAN_POINT('Ctrl Pts',(115.660690261598,10.9096166271091,-6.66011943875589));
#53961=CARTESIAN_POINT('Ctrl Pts',(115.707879192453,11.6857879496437,-4.75101863178023));
#53962=CARTESIAN_POINT('Ctrl Pts',(115.755068123308,12.4619592721784,-2.84191782480457));
#53963=CARTESIAN_POINT('Ctrl Pts',(115.802257054163,12.7605379634937,-0.738645129088155));
#53964=CARTESIAN_POINT('Ctrl Pts',(115.849445985018,12.5463531377727,1.31104574001571));
#53965=CARTESIAN_POINT('Ctrl Pts',(115.896634915873,12.3321683120517,3.36073660911957));
#53966=CARTESIAN_POINT('Ctrl Pts',(115.943823846728,11.6052199692944,5.35684565161087));
#53967=CARTESIAN_POINT('Ctrl Pts',(115.991012777583,10.4511385260698,7.06424245935823));
#53968=CARTESIAN_POINT('Ctrl Pts',(116.038201708439,9.2970570828451,8.77163926710553));
#53969=CARTESIAN_POINT('Ctrl Pts',(116.085390639294,7.715842539153,10.1903238401089));
#53970=CARTESIAN_POINT('Ctrl Pts',(116.132579570149,5.89375311256478,11.1531830618864));
#53971=CARTESIAN_POINT('Ctrl Pts',(116.179768501004,4.07166368597657,12.1160422836638));
#53972=CARTESIAN_POINT('Ctrl Pts',(116.226957431859,2.00869937649223,12.6230761542154));
#53973=CARTESIAN_POINT('Ctrl Pts',(116.274146362714,-0.0521342739010579,
12.6145590293455));
#53974=CARTESIAN_POINT('Ctrl Pts',(116.321335293569,-2.11296792429447,12.6060419044757));
#53975=CARTESIAN_POINT('Ctrl Pts',(116.368524224424,-4.17167091559683,12.0819737841843));
#53976=CARTESIAN_POINT('Ctrl Pts',(116.415713155279,-5.98573947024097,11.1040867412508));
#53977=CARTESIAN_POINT('Ctrl Pts',(116.462902086134,-7.79980802488507,10.1261996983172));
#53978=CARTESIAN_POINT('Ctrl Pts',(116.510091016989,-9.36924214287096,8.69449373274147));
#53979=CARTESIAN_POINT('Ctrl Pts',(116.557279947844,-10.509171587856,6.97761620580043));
#53980=CARTESIAN_POINT('Ctrl Pts',(116.604468878699,-11.6491010328411,5.26073867885939));
#53981=CARTESIAN_POINT('Ctrl Pts',(116.651657809554,-12.3595258048254,3.25868959055305));
#53982=CARTESIAN_POINT('Ctrl Pts',(116.69884674041,-12.5567612492482,1.20729812576737));
#53983=CARTESIAN_POINT('Ctrl Pts',(116.746035671265,-12.753996693671,-0.844093339018264));
#53984=CARTESIAN_POINT('Ctrl Pts',(116.79322460212,-12.4380428105324,-2.94482718028324));
#53985=CARTESIAN_POINT('Ctrl Pts',(116.840413532975,-11.6461184937333,-4.84744672668254));
#53986=CARTESIAN_POINT('Ctrl Pts',(116.88760246383,-10.8541941769342,-6.75006627308188));
#53987=CARTESIAN_POINT('Ctrl Pts',(116.934791394685,-9.58629942647459,-8.45457152461553));
#53988=CARTESIAN_POINT('Ctrl Pts',(116.98198032554,-7.9917823356575,-9.76018568531958));
#53989=CARTESIAN_POINT('Ctrl Pts',(117.029169256395,-6.3972652448404,-11.0657998460236));
#53990=CARTESIAN_POINT('Ctrl Pts',(117.07635818725,-4.47612581366579,-11.9725229158981));
#53991=CARTESIAN_POINT('Ctrl Pts',(117.123547118105,-2.45466943807836,-12.3735387369587));
#53992=CARTESIAN_POINT('Ctrl Pts',(117.129466903404,-2.20108056633454,-12.4238456101826));
#53993=CARTESIAN_POINT('Ctrl Pts',(117.135386688703,-1.94591297160764,-12.4661939908398));
#53994=CARTESIAN_POINT('Ctrl Pts',(117.141306474002,-1.68966005362669,-12.5006082646709));
#53995=CARTESIAN_POINT('',(115.327020759716,-1.68935314531923,-12.5));
#53996=CARTESIAN_POINT('Ctrl Pts',(115.327020759716,-1.68956493984068,-12.4995253250381));
#53997=CARTESIAN_POINT('Ctrl Pts',(115.326518854553,-1.68037728524638,-12.4995179807198));
#53998=CARTESIAN_POINT('Ctrl Pts',(115.326022683248,-1.67118932027433,-12.4995106941419));
#53999=CARTESIAN_POINT('Ctrl Pts',(115.325532250178,-1.66200103015941,-12.4995034672907));
#54000=CARTESIAN_POINT('Ctrl Pts',(115.312311851236,-1.41431613999935,-12.4993086560875));
#54001=CARTESIAN_POINT('Ctrl Pts',(115.303279041712,-1.16672568500685,-12.4991596530256));
#54002=CARTESIAN_POINT('Ctrl Pts',(115.298484905107,-0.918930641817005,
-12.4990826397731));
#54003=CARTESIAN_POINT('Ctrl Pts',(115.296374451076,-0.809847382263608,
-12.499048737333));
#54004=CARTESIAN_POINT('Ctrl Pts',(115.295085408755,-0.70072381008354,-12.4990285536869));
#54005=CARTESIAN_POINT('Ctrl Pts',(115.294622136041,-0.591531575591215,
-12.4990229307716));
#54006=CARTESIAN_POINT('Ctrl Pts',(115.293869155035,-0.414055812104477,
-12.4990137915577));
#54007=CARTESIAN_POINT('Ctrl Pts',(115.295298710178,-0.236659403045372,
-12.4990433559505));
#54008=CARTESIAN_POINT('Ctrl Pts',(115.298910317785,-0.0592230017119202,
-12.4991092977448));
#54009=CARTESIAN_POINT('Ctrl Pts',(115.299179616569,-0.0459924926625598,
-12.4991142146813));
#54010=CARTESIAN_POINT('Ctrl Pts',(115.299461036758,-0.0327622823487279,
-12.4991193305549));
#54011=CARTESIAN_POINT('Ctrl Pts',(115.299754575282,-0.0195323214148313,
-12.4991246428424));
#54012=CARTESIAN_POINT('Ctrl Pts',(115.299835227329,-0.0158972842946123,
-12.4991261024357));
#54013=CARTESIAN_POINT('Ctrl Pts',(115.299916794136,-0.0122622694687753,
-12.4991275768541));
#54014=CARTESIAN_POINT('Ctrl Pts',(115.299999275632,-0.00862727598571485,
-12.4991290660423));
#54015=CARTESIAN_POINT('Ctrl Pts',(115.300047728892,-0.00649192084135235,
-12.499129940857));
#54016=CARTESIAN_POINT('Ctrl Pts',(115.300096497795,-0.0043565734465251,
-12.4991308207685));
#54017=CARTESIAN_POINT('Ctrl Pts',(115.300145582325,-0.00222123354126288,
-12.4991317057653));
#54018=CARTESIAN_POINT('Ctrl Pts',(115.300187960563,-0.000377639640268286,
-12.4991324698473));
#54019=CARTESIAN_POINT('Ctrl Pts',(115.300230574068,0.00146594842845679,
-12.4991332377199));
#54020=CARTESIAN_POINT('Ctrl Pts',(115.300273422832,0.00330953078475597,
-12.4991340093757));
#54021=CARTESIAN_POINT('Ctrl Pts',(115.300325606511,0.0055547510331301,
-12.4991349491423));
#54022=CARTESIAN_POINT('Ctrl Pts',(115.300378139113,0.00779996250852122,
-12.49913589452));
#54023=CARTESIAN_POINT('Ctrl Pts',(115.300431020618,0.0100451654044689,
-12.4991368454951));
#54024=CARTESIAN_POINT('Ctrl Pts',(115.300530789124,0.0142810610559831,
-12.4991386396453));
#54025=CARTESIAN_POINT('Ctrl Pts',(115.300631799487,0.0185169245314509,
-12.4991404537185));
#54026=CARTESIAN_POINT('Ctrl Pts',(115.300734051588,0.0227527574583523,
-12.4991422876221));
#54027=CARTESIAN_POINT('Ctrl Pts',(115.301316483569,0.0468802282284872,
-12.4991527336089));
#54028=CARTESIAN_POINT('Ctrl Pts',(115.301939197372,0.0710064513896376,
-12.4991638230625));
#54029=CARTESIAN_POINT('Ctrl Pts',(115.302602168403,0.0951317251787609,
-12.4991755374429));
#54030=CARTESIAN_POINT('Ctrl Pts',(115.303449821618,0.125977516261023,-12.499190515069));
#54031=CARTESIAN_POINT('Ctrl Pts',(115.304363262483,0.156820945974577,-12.4992065140888));
#54032=CARTESIAN_POINT('Ctrl Pts',(115.305342429159,0.18766263524768,-12.4992234901137));
#54033=CARTESIAN_POINT('Ctrl Pts',(115.310164225167,0.339539060211866,-12.4993070866366));
#54034=CARTESIAN_POINT('Ctrl Pts',(115.31657780893,0.491309083351229,-12.4994146211685));
#54035=CARTESIAN_POINT('Ctrl Pts',(115.324571683316,0.643045308941025,-12.4995385978385));
#54036=CARTESIAN_POINT('Ctrl Pts',(115.337251836494,0.883734427911741,-12.4997352538142));
#54037=CARTESIAN_POINT('Ctrl Pts',(115.353886501112,1.12391931965973,-12.4999745588541));
#54038=CARTESIAN_POINT('Ctrl Pts',(115.374386304944,1.36387073326171,-12.500207396726));
#54039=CARTESIAN_POINT('Ctrl Pts',(115.383667815097,1.47251135732339,-12.5003128166164));
#54040=CARTESIAN_POINT('Ctrl Pts',(115.393741649628,1.58110346898439,-12.5004166949864));
#54041=CARTESIAN_POINT('Ctrl Pts',(115.404599513671,1.68966869690974,-12.5005137686862));
#54042=CARTESIAN_POINT('',(113.590313799386,1.68935314531925,-12.5));
#54043=CARTESIAN_POINT('Ctrl Pts',(113.590313799386,1.68940030131958,-12.5009781087056));
#54044=CARTESIAN_POINT('Ctrl Pts',(113.635523898437,3.64596800314944,-12.2358114053962));
#54045=CARTESIAN_POINT('Ctrl Pts',(113.680733997489,5.53979258690265,-11.5038643043075));
#54046=CARTESIAN_POINT('Ctrl Pts',(113.72594409654,7.16483737795765,-10.382433402778));
#54047=CARTESIAN_POINT('Ctrl Pts',(113.773133027395,8.86100986796402,-9.21191782370736));
#54048=CARTESIAN_POINT('Ctrl Pts',(113.82032195825,10.2643588270521,-7.61707711016277));
#54049=CARTESIAN_POINT('Ctrl Pts',(113.867510889105,11.2095776534377,-5.78577452219343));
#54050=CARTESIAN_POINT('Ctrl Pts',(113.91469981996,12.1547964798232,-3.95447193422415));
#54051=CARTESIAN_POINT('Ctrl Pts',(113.961888750815,12.6418851735062,-1.88670747183014));
#54052=CARTESIAN_POINT('Ctrl Pts',(114.00907768167,12.613467413778,0.173947822985603));
#54053=CARTESIAN_POINT('Ctrl Pts',(114.056266612526,12.5850496540499,2.23460311780141));
#54054=CARTESIAN_POINT('Ctrl Pts',(114.103455543381,12.0411254409105,4.28814924503892));
#54055=CARTESIAN_POINT('Ctrl Pts',(114.150644474236,11.0457659948499,6.09269001280186));
#54056=CARTESIAN_POINT('Ctrl Pts',(114.197833405091,10.0504065487893,7.8972307805648));
#54057=CARTESIAN_POINT('Ctrl Pts',(114.245022335946,8.60361186980746,9.45276618885315));
#54058=CARTESIAN_POINT('Ctrl Pts',(114.292211266801,6.87580623961835,10.5760629054651));
#54059=CARTESIAN_POINT('Ctrl Pts',(114.339400197656,5.14800060942926,11.6993596220771));
#54060=CARTESIAN_POINT('Ctrl Pts',(114.386589128511,3.13918402803281,12.3904176470127));
#54061=CARTESIAN_POINT('Ctrl Pts',(114.433778059366,1.08598380234995,12.5678342286195));
#54062=CARTESIAN_POINT('Ctrl Pts',(114.480966990221,-0.967216423332948,
12.7452508102263));
#54063=CARTESIAN_POINT('Ctrl Pts',(114.528155921076,-3.06480029330234,12.4090259485043));
#54064=CARTESIAN_POINT('Ctrl Pts',(114.575344851931,-4.95968421424995,11.5987650426319));
#54065=CARTESIAN_POINT('Ctrl Pts',(114.622533782786,-6.8545681351975,10.7885041367596));
#54066=CARTESIAN_POINT('Ctrl Pts',(114.669722713641,-8.54675210712326,9.50420718673705));
#54067=CARTESIAN_POINT('Ctrl Pts',(114.716911644497,-9.83690636612127,7.89715715707163));
#54068=CARTESIAN_POINT('Ctrl Pts',(114.764100575352,-11.1270606251194,6.29010712740612));
#54069=CARTESIAN_POINT('Ctrl Pts',(114.811289506207,-12.0151851711896,4.36030401809775));
#54070=CARTESIAN_POINT('Ctrl Pts',(114.858478437062,-12.3966639232179,2.33506779202817));
#54071=CARTESIAN_POINT('Ctrl Pts',(114.905667367917,-12.7781426752463,0.309831565958702));
#54072=CARTESIAN_POINT('Ctrl Pts',(114.952856298772,-12.6529756332327,-1.81083777687195));
#54073=CARTESIAN_POINT('Ctrl Pts',(115.000045229627,-12.0359067713131,-3.77713730377714));
#54074=CARTESIAN_POINT('Ctrl Pts',(115.047234160482,-11.4188379093935,-5.74343683068239));
#54075=CARTESIAN_POINT('Ctrl Pts',(115.094423091337,-10.3098672275678,-7.55536654166215));
#54076=CARTESIAN_POINT('Ctrl Pts',(115.141612022192,-8.83962524112239,-8.99949129761083));
#54077=CARTESIAN_POINT('Ctrl Pts',(115.188800953047,-7.36938325467695,-10.4436160535595));
#54078=CARTESIAN_POINT('Ctrl Pts',(115.235989883902,-5.53786996361174,-11.5199358544771));
#54079=CARTESIAN_POINT('Ctrl Pts',(115.283178814757,-3.56082734221149,-12.1016662760128));
#54080=CARTESIAN_POINT('Ctrl Pts',(115.29779279641,-2.94855526754347,-12.2818228837843));
#54081=CARTESIAN_POINT('Ctrl Pts',(115.312406778063,-2.32232570141222,-12.4145441943231));
#54082=CARTESIAN_POINT('Ctrl Pts',(115.327020759716,-1.68956493984086,-12.4995253250381));
#54083=CARTESIAN_POINT('',(113.51273504543,-1.68935314531931,-12.5));
#54084=CARTESIAN_POINT('Ctrl Pts',(113.51273504543,-1.68923172356653,-12.4990204999488));
#54085=CARTESIAN_POINT('Ctrl Pts',(113.512233140265,-1.6800439586769,-12.4990205731998));
#54086=CARTESIAN_POINT('Ctrl Pts',(113.511736968961,-1.670855904336,-12.4990207456443));
#54087=CARTESIAN_POINT('Ctrl Pts',(113.511246535892,-1.66166754556756,-12.4990210174009));
#54088=CARTESIAN_POINT('Ctrl Pts',(113.498080335484,-1.41499622421194,-12.4990283129998));
#54089=CARTESIAN_POINT('Ctrl Pts',(113.489067459873,-1.16843347430942,-12.4991094506017));
#54090=CARTESIAN_POINT('Ctrl Pts',(113.484258366864,-0.921681029186322,
-12.4992529586073));
#54091=CARTESIAN_POINT('Ctrl Pts',(113.48211281744,-0.811593832833913,-12.4993169838857));
#54092=CARTESIAN_POINT('Ctrl Pts',(113.480804008808,-0.70146820779939,-12.4993931672618));
#54093=CARTESIAN_POINT('Ctrl Pts',(113.480336421755,-0.591274738865397,
-12.4994789473658));
#54094=CARTESIAN_POINT('Ctrl Pts',(113.479583440748,-0.413824168452118,
-12.4996170837591));
#54095=CARTESIAN_POINT('Ctrl Pts',(113.481012995891,-0.236458362509808,
-12.4997801223198));
#54096=CARTESIAN_POINT('Ctrl Pts',(113.484624603499,-0.059056775375869,
-12.4999513037557));
#54097=CARTESIAN_POINT('Ctrl Pts',(113.484893902283,-0.0458288622444513,
-12.4999640678645));
#54098=CARTESIAN_POINT('Ctrl Pts',(113.485175322472,-0.0326012711593641,
-12.4999768735535));
#54099=CARTESIAN_POINT('Ctrl Pts',(113.485468860997,-0.0193739522482943,
-12.4999897123243));
#54100=CARTESIAN_POINT('Ctrl Pts',(113.485549513044,-0.0157396410409706,
-12.4999932398788));
#54101=CARTESIAN_POINT('Ctrl Pts',(113.485631079851,-0.0121053538488512,
-12.4999967699262));
#54102=CARTESIAN_POINT('Ctrl Pts',(113.485713561346,-0.00847108973138637,
-12.5000003022872));
#54103=CARTESIAN_POINT('Ctrl Pts',(113.485762014607,-0.00633616302775324,
-12.5000023773515));
#54104=CARTESIAN_POINT('Ctrl Pts',(113.485810783509,-0.00420124466411693,
-12.5000044532139));
#54105=CARTESIAN_POINT('Ctrl Pts',(113.48585986804,-0.00206633441641477,
-12.5000065298378));
#54106=CARTESIAN_POINT('Ctrl Pts',(113.485902246277,-0.000223111464762653,
-12.5000083227379));
#54107=CARTESIAN_POINT('Ctrl Pts',(113.485944859782,0.00162010521623557,
-12.5000101162055));
#54108=CARTESIAN_POINT('Ctrl Pts',(113.485987708546,0.00346331579858671,
-12.500011910217));
#54109=CARTESIAN_POINT('Ctrl Pts',(113.486039892225,0.00570808321031068,
-12.500014095067));
#54110=CARTESIAN_POINT('Ctrl Pts',(113.486092424826,0.00795284120093064,
-12.5000162807233));
#54111=CARTESIAN_POINT('Ctrl Pts',(113.486145306333,0.0101975900499408,
-12.5000184671433));
#54112=CARTESIAN_POINT('Ctrl Pts',(113.486245074839,0.0144326289741938,
-12.5000225921365));
#54113=CARTESIAN_POINT('Ctrl Pts',(113.486346085202,0.018667633424933,-12.5000267198462));
#54114=CARTESIAN_POINT('Ctrl Pts',(113.486448337302,0.0229026050402846,
-12.5000308499837));
#54115=CARTESIAN_POINT('Ctrl Pts',(113.487030769284,0.0470251697744376,
-12.5000543754093));
#54116=CARTESIAN_POINT('Ctrl Pts',(113.487653483087,0.0711464129353356,
-12.5000779795403));
#54117=CARTESIAN_POINT('Ctrl Pts',(113.488316454118,0.0952666358180398,
-12.5001016076708));
#54118=CARTESIAN_POINT('Ctrl Pts',(113.489164107301,0.126105967784969,-12.5001318178294));
#54119=CARTESIAN_POINT('Ctrl Pts',(113.49007754813,0.156942822632197,-12.5001620666217));
#54120=CARTESIAN_POINT('Ctrl Pts',(113.491056714763,0.187777827657472,-12.5001922342553));
#54121=CARTESIAN_POINT('Ctrl Pts',(113.495878510601,0.339621338049009,-12.5003407913702));
#54122=CARTESIAN_POINT('Ctrl Pts',(113.502292094098,0.491355809643231,-12.5004875912149));
#54123=CARTESIAN_POINT('Ctrl Pts',(113.510285968124,0.643054608681126,-12.5006162471355));
#54124=CARTESIAN_POINT('Ctrl Pts',(113.523057368732,0.885415962900539,-12.5008217940703));
#54125=CARTESIAN_POINT('Ctrl Pts',(113.539840399663,1.12726119776551,-12.5009822132088));
#54126=CARTESIAN_POINT('Ctrl Pts',(113.560543745381,1.36886981331526,-12.5010129660893));
#54127=CARTESIAN_POINT('Ctrl Pts',(113.562246397364,1.3887398089245,-12.5010154952193));
#54128=CARTESIAN_POINT('Ctrl Pts',(113.563975564349,1.4086081755581,-12.5010171404161));
#54129=CARTESIAN_POINT('Ctrl Pts',(113.565731195542,1.42847505288237,-12.5010178514909));
#54130=CARTESIAN_POINT('Ctrl Pts',(113.573419321789,1.51547456714083,-12.5010209653754));
#54131=CARTESIAN_POINT('Ctrl Pts',(113.581614944879,1.60244560010039,-12.5010061863381));
#54132=CARTESIAN_POINT('Ctrl Pts',(113.590313799386,1.68940030132012,-12.5009781087056));
#54133=CARTESIAN_POINT('',(111.7760280851,1.68935314531926,-12.5));
#54134=CARTESIAN_POINT('Ctrl Pts',(111.7760280851,1.68925638115339,-12.4991303417189));
#54135=CARTESIAN_POINT('Ctrl Pts',(111.812543987797,3.26988754097161,-12.284116080938));
#54136=CARTESIAN_POINT('Ctrl Pts',(111.849059890495,4.81020923824029,-11.7696927456239));
#54137=CARTESIAN_POINT('Ctrl Pts',(111.885575793192,6.19900628169252,-10.9861999489504));
#54138=CARTESIAN_POINT('Ctrl Pts',(111.932764724047,7.99372701469248,-9.97370444215502));
#54139=CARTESIAN_POINT('Ctrl Pts',(111.979953654902,9.53540173774336,-8.51186322242636));
#54140=CARTESIAN_POINT('Ctrl Pts',(112.027142585757,10.64200964519,-6.77327960690641));
#54141=CARTESIAN_POINT('Ctrl Pts',(112.074331516612,11.7486175526366,-5.03469599138647));
#54142=CARTESIAN_POINT('Ctrl Pts',(112.121520447468,12.420158644479,-3.01936998007523));
#54143=CARTESIAN_POINT('Ctrl Pts',(112.168709378323,12.5777166450503,-0.964573554423232));
#54144=CARTESIAN_POINT('Ctrl Pts',(112.215898309178,12.7352746456215,1.0902228712287));
#54145=CARTESIAN_POINT('Ctrl Pts',(112.263087240033,12.3788495549217,3.18448971122139));
#54146=CARTESIAN_POINT('Ctrl Pts',(112.310276170888,11.5503385958018,5.07146765373859));
#54147=CARTESIAN_POINT('Ctrl Pts',(112.357465101743,10.7218276366819,6.95844559625586));
#54148=CARTESIAN_POINT('Ctrl Pts',(112.404654032598,9.42123080914186,8.63813464129762));
#54149=CARTESIAN_POINT('Ctrl Pts',(112.451842963453,7.80179199338407,9.91270604401158));
#54150=CARTESIAN_POINT('Ctrl Pts',(112.499031894308,6.18235317762629,11.1872774467255));
#54151=CARTESIAN_POINT('Ctrl Pts',(112.546220825163,4.2440723736507,12.0567312071117));
#54152=CARTESIAN_POINT('Ctrl Pts',(112.593409756018,2.21524905293368,12.4186365821184));
#54153=CARTESIAN_POINT('Ctrl Pts',(112.640598686873,0.186425732216652,12.7805419571252));
#54154=CARTESIAN_POINT('Ctrl Pts',(112.687787617728,-1.93294010524181,12.6348989467525));
#54155=CARTESIAN_POINT('Ctrl Pts',(112.734976548583,-3.89319014102203,11.9988699483865));
#54156=CARTESIAN_POINT('Ctrl Pts',(112.782165479439,-5.85344017680225,11.3628409500206));
#54157=CARTESIAN_POINT('Ctrl Pts',(112.829354410294,-7.65457441090422,10.2364259636613));
#54158=CARTESIAN_POINT('Ctrl Pts',(112.876543341149,-9.08443352514128,8.75230731095469));
#54159=CARTESIAN_POINT('Ctrl Pts',(112.923732272004,-10.5142926393783,7.26818865824804));
#54160=CARTESIAN_POINT('Ctrl Pts',(112.970921202859,-11.5728766337505,5.42636633919398));
#54161=CARTESIAN_POINT('Ctrl Pts',(113.018110133714,-12.1354883111685,3.44379808998662));
#54162=CARTESIAN_POINT('Ctrl Pts',(113.065299064569,-12.6980999885865,1.46122984077925));
#54163=CARTESIAN_POINT('Ctrl Pts',(113.112487995424,-12.7647393490503,-0.662084338581423));
#54164=CARTESIAN_POINT('Ctrl Pts',(113.159676926279,-12.3275575619273,-2.67603063058306));
#54165=CARTESIAN_POINT('Ctrl Pts',(113.206865857134,-11.8903757748043,-4.68997692258463));
#54166=CARTESIAN_POINT('Ctrl Pts',(113.254054787989,-10.9493728400946,-6.59455532722717));
#54167=CARTESIAN_POINT('Ctrl Pts',(113.301243718844,-9.6153931900996,-8.1654169007227));
#54168=CARTESIAN_POINT('Ctrl Pts',(113.348432649699,-8.28141354010458,-9.73627847421828));
#54169=CARTESIAN_POINT('Ctrl Pts',(113.395621580554,-6.55445717482431,-10.9734232165668));
#54170=CARTESIAN_POINT('Ctrl Pts',(113.44281051141,-4.6379500495765,-11.7311225730955));
#54171=CARTESIAN_POINT('Ctrl Pts',(113.466118689416,-3.69132361796918,-12.1053754149728));
#54172=CARTESIAN_POINT('Ctrl Pts',(113.489426867423,-2.6984524927118,-12.3626579793741));
#54173=CARTESIAN_POINT('Ctrl Pts',(113.51273504543,-1.68923172356706,-12.4990204999487));
#54174=CARTESIAN_POINT('',(111.680383100847,0.293137397039349,-12.5));
#54175=CARTESIAN_POINT('Ctrl Pts',(111.680383100847,0.293137397039376,-12.5));
#54176=CARTESIAN_POINT('Ctrl Pts',(111.68465314286,0.409731183256787,-12.5000000034602));
#54177=CARTESIAN_POINT('Ctrl Pts',(111.689860597525,0.526270087563317,-12.4999689964682));
#54178=CARTESIAN_POINT('Ctrl Pts',(111.696000254414,0.642788658290244,-12.4999174059816));
#54179=CARTESIAN_POINT('Ctrl Pts',(111.708516098598,0.880314680028347,-12.499812237484));
#54180=CARTESIAN_POINT('Ctrl Pts',(111.724884633411,1.11734811706522,-12.4996240015796));
#54181=CARTESIAN_POINT('Ctrl Pts',(111.74501991605,1.35416465501358,-12.499421500197));
#54182=CARTESIAN_POINT('Ctrl Pts',(111.754520404583,1.46590248574335,-12.4993259533851));
#54183=CARTESIAN_POINT('Ctrl Pts',(111.764859470146,1.57759136494832,-12.4992269184326));
#54184=CARTESIAN_POINT('Ctrl Pts',(111.7760280851,1.68925638115339,-12.4991303417189));
#54185=CARTESIAN_POINT('',(111.185928218469,1.41330412150968,-11.5105178568576));
#54186=CARTESIAN_POINT('Ctrl Pts',(111.185928218469,1.4133810675711,-11.5111948783535));
#54187=CARTESIAN_POINT('Ctrl Pts',(111.194692020162,1.40292731174206,-11.5283132100807));
#54188=CARTESIAN_POINT('Ctrl Pts',(111.203416294175,1.39232321605708,-11.5453647146798));
#54189=CARTESIAN_POINT('Ctrl Pts',(111.296332057201,1.27717818405291,-11.7270809017656));
#54190=CARTESIAN_POINT('Ctrl Pts',(111.378208707921,1.1561743340081,-11.8882169128781));
#54191=CARTESIAN_POINT('Ctrl Pts',(111.492960338586,0.936239464533711,-12.1161930051839));
#54192=CARTESIAN_POINT('Ctrl Pts',(111.532910695054,0.847236652983905,-12.1960892434571));
#54193=CARTESIAN_POINT('Ctrl Pts',(111.617582618094,0.614009366313158,-12.3672109959224));
#54194=CARTESIAN_POINT('Ctrl Pts',(111.657833646957,0.460862322932455,-12.4502435215011));
#54195=CARTESIAN_POINT('Ctrl Pts',(111.680383100847,0.293137397039347,-12.5));
#54196=CARTESIAN_POINT('Ctrl Pts',(111.185928218469,1.41330412150968,-11.5105178568576));
#54197=CARTESIAN_POINT('Ctrl Pts',(111.223614785545,2.91555500390263,-11.3247312662987));
#54198=CARTESIAN_POINT('Ctrl Pts',(111.308490283475,6.2177932578697,-10.2437804539548));
#54199=CARTESIAN_POINT('Ctrl Pts',(111.440554712261,10.1848431574681,-6.48215877251662));
#54200=CARTESIAN_POINT('Ctrl Pts',(111.582121504826,12.0371931123728,-0.923170511755194));
#54201=CARTESIAN_POINT('Ctrl Pts',(111.723688297391,11.0540455303336,4.85356472268307));
#54202=CARTESIAN_POINT('Ctrl Pts',(111.865255089956,7.46653539266892,9.48674646633624));
#54203=CARTESIAN_POINT('Ctrl Pts',(112.006821882522,2.12006530550471,11.8850101815537));
#54204=CARTESIAN_POINT('Ctrl Pts',(112.148388675087,-3.72590191992946,11.4832747896718));
#54205=CARTESIAN_POINT('Ctrl Pts',(112.289955467652,-8.69407282986275,8.37622032266638));
#54206=CARTESIAN_POINT('Ctrl Pts',(112.41094761607,-11.1896532283784,4.03417878282034));
#54207=CARTESIAN_POINT('Ctrl Pts',(112.484750833632,-11.5964486036021,1.06906004117227));
#54208=CARTESIAN_POINT('Ctrl Pts',(112.51136512034,-11.5967929078458,-0.000103121459272826));
#54209=CARTESIAN_POINT('',(117.38636,8.26359861637683,-9.5301578966699));
#54210=CARTESIAN_POINT('Ctrl Pts',(117.38636,8.26387335187489,-9.53028995448194));
#54211=CARTESIAN_POINT('Ctrl Pts',(117.38636,8.47976957198238,-9.32791670058071));
#54212=CARTESIAN_POINT('Ctrl Pts',(117.38636,8.68824929570293,-9.11813352201538));
#54213=CARTESIAN_POINT('Ctrl Pts',(117.38636,8.88884239823733,-8.90122282433969));
#54214=CARTESIAN_POINT('Ctrl Pts',(117.38636,9.08931532045339,-8.68444208325957));
#54215=CARTESIAN_POINT('Ctrl Pts',(117.38636,9.28191144627861,-8.46054188219358));
#54216=CARTESIAN_POINT('Ctrl Pts',(117.38636,9.46637461395972,-8.23002395669524));
#54217=CARTESIAN_POINT('Ctrl Pts',(117.38636,9.60235548331953,-8.06009286255685));
#54218=CARTESIAN_POINT('Ctrl Pts',(117.38636,9.73391591056565,-7.88656480486491));
#54219=CARTESIAN_POINT('Ctrl Pts',(117.38636,9.86093772130342,-7.70963148326641));
#54220=CARTESIAN_POINT('Ctrl Pts',(117.38636,9.93324774835431,-7.60890820435329));
#54221=CARTESIAN_POINT('Ctrl Pts',(117.38636,10.0040866925942,-7.50708124723151));
#54222=CARTESIAN_POINT('Ctrl Pts',(117.38636,10.0734307086138,-7.40418509686393));
#54223=CARTESIAN_POINT('Ctrl Pts',(117.38636,10.1027826310885,-7.3606312330717));
#54224=CARTESIAN_POINT('Ctrl Pts',(117.38636,10.1318666948828,-7.31688579952516));
#54225=CARTESIAN_POINT('Ctrl Pts',(117.38636,10.1606810083502,-7.27295138321782));
#54226=CARTESIAN_POINT('Ctrl Pts',(117.38636,10.1819607036973,-7.24050532146012));
#54227=CARTESIAN_POINT('Ctrl Pts',(117.38636,10.2030931380199,-7.20795631949656));
#54228=CARTESIAN_POINT('Ctrl Pts',(117.38636,10.2240699550889,-7.17531745591445));
#54229=CARTESIAN_POINT('Ctrl Pts',(117.38636,10.3828565791808,-6.92825352122177));
#54230=CARTESIAN_POINT('Ctrl Pts',(117.38636,10.5328439411404,-6.67587035946744));
#54231=CARTESIAN_POINT('Ctrl Pts',(117.38636,10.6737840324592,-6.41866348831899));
#54232=CARTESIAN_POINT('Ctrl Pts',(117.38636,10.8143371275405,-6.16216286115299));
#54233=CARTESIAN_POINT('Ctrl Pts',(117.38636,10.9458928173572,-5.90086440777249));
#54234=CARTESIAN_POINT('Ctrl Pts',(117.38636,11.0681586584076,-5.63523743592315));
#54235=CARTESIAN_POINT('Ctrl Pts',(117.38636,11.1894667796723,-5.37169114502583));
#54236=CARTESIAN_POINT('Ctrl Pts',(117.38636,11.3016302228804,-5.10388332829134));
#54237=CARTESIAN_POINT('Ctrl Pts',(117.38636,11.4043142401143,-4.83225891361791));
#54238=CARTESIAN_POINT('Ctrl Pts',(117.38636,11.4301093636643,-4.76402448410825));
#54239=CARTESIAN_POINT('Ctrl Pts',(117.38636,11.455306027814,-4.69554916125278));
#54240=CARTESIAN_POINT('Ctrl Pts',(117.38636,11.4798984095742,-4.62683992670232));
#54241=CARTESIAN_POINT('Ctrl Pts',(117.38636,11.4917596009721,-4.59370066472471));
#54242=CARTESIAN_POINT('Ctrl Pts',(117.38636,11.5034804972838,-4.56050606622592));
#54243=CARTESIAN_POINT('Ctrl Pts',(117.38636,11.5150549867001,-4.5272728997837));
#54244=CARTESIAN_POINT('Ctrl Pts',(117.38636,11.6106843556848,-4.25269778705742));
#54245=CARTESIAN_POINT('Ctrl Pts',(117.38636,11.6964150816106,-3.97523906689843));
#54246=CARTESIAN_POINT('Ctrl Pts',(117.38636,11.7720112400975,-3.6953694569451));
#54247=CARTESIAN_POINT('Ctrl Pts',(117.38636,11.780970475401,-3.6622008708682));
#54248=CARTESIAN_POINT('Ctrl Pts',(117.38636,11.7897873083534,-3.62899839917189));
#54249=CARTESIAN_POINT('Ctrl Pts',(117.38636,11.7984613009022,-3.59576281126187));
#54250=CARTESIAN_POINT('Ctrl Pts',(117.38636,11.8714983117827,-3.31591152223404));
#54251=CARTESIAN_POINT('Ctrl Pts',(117.38636,11.9344121502825,-3.03371329005597));
#54252=CARTESIAN_POINT('Ctrl Pts',(117.38636,11.9872470138898,-2.74972118066531));
#54253=CARTESIAN_POINT('Ctrl Pts',(117.38636,12.0403084305658,-2.46451132830214));
#54254=CARTESIAN_POINT('Ctrl Pts',(117.38636,12.083204263492,-2.1774915497814));
#54255=CARTESIAN_POINT('Ctrl Pts',(117.38636,12.1159270329586,-1.88921534265928));
#54256=CARTESIAN_POINT('Ctrl Pts',(117.38636,12.1485656405205,-1.60168057261786));
#54257=CARTESIAN_POINT('Ctrl Pts',(117.38636,12.1710834102292,-1.31289520014115));
#54258=CARTESIAN_POINT('Ctrl Pts',(117.38636,12.1834213208703,-1.02341125602325));
#54259=CARTESIAN_POINT('Ctrl Pts',(117.38636,12.1954299880651,-0.741652338792809));
#54260=CARTESIAN_POINT('Ctrl Pts',(117.38636,12.1977946382116,-0.45923111551291));
#54261=CARTESIAN_POINT('Ctrl Pts',(117.38636,12.1904140997534,-0.176667623965072));
#54262=CARTESIAN_POINT('Ctrl Pts',(117.38636,12.188541218074,-0.104964456292086));
#54263=CARTESIAN_POINT('Ctrl Pts',(117.38636,12.1860405744826,-0.0332522057484106));
#54264=CARTESIAN_POINT('Ctrl Pts',(117.38636,12.1829100435733,0.038460452303122));
#54265=CARTESIAN_POINT('Ctrl Pts',(117.38636,12.1810033822858,0.0821373086886409));
#54266=CARTESIAN_POINT('Ctrl Pts',(117.38636,12.178862664041,0.125820640607877));
#54267=CARTESIAN_POINT('Ctrl Pts',(117.38636,12.1764894055144,0.169474133586869));
#54268=CARTESIAN_POINT('Ctrl Pts',(117.38636,12.1608830020532,0.456536843476998));
#54269=CARTESIAN_POINT('Ctrl Pts',(117.38636,12.135218529062,0.742528071737549));
#54270=CARTESIAN_POINT('Ctrl Pts',(117.38636,12.0995281849933,1.0269159598467));
#54271=CARTESIAN_POINT('Ctrl Pts',(117.38636,12.0639225554078,1.31062882580099));
#54272=CARTESIAN_POINT('Ctrl Pts',(117.38636,12.0183385342614,1.59274657006241));
#54273=CARTESIAN_POINT('Ctrl Pts',(117.38636,11.9627566092262,1.8727375600685));
#54274=CARTESIAN_POINT('Ctrl Pts',(117.38636,11.93197934801,2.02777637587353));
#54275=CARTESIAN_POINT('Ctrl Pts',(117.38636,11.8981356764896,2.18216298153699));
#54276=CARTESIAN_POINT('Ctrl Pts',(117.38636,11.8612155579909,2.33580559846095));
#54277=CARTESIAN_POINT('Ctrl Pts',(117.38636,11.7942814757869,2.61435095447361));
#54278=CARTESIAN_POINT('Ctrl Pts',(117.38636,11.7172385264076,2.89045234807707));
#54279=CARTESIAN_POINT('Ctrl Pts',(117.38636,11.6303372664751,3.16361450639462));
#54280=CARTESIAN_POINT('Ctrl Pts',(117.38636,11.5436997487744,3.43594762728112));
#54281=CARTESIAN_POINT('Ctrl Pts',(117.38636,11.4472633370757,3.70535986996651));
#54282=CARTESIAN_POINT('Ctrl Pts',(117.38636,11.3412316896956,3.97133458703356));
#54283=CARTESIAN_POINT('Ctrl Pts',(117.38636,11.2770779669014,4.13226076983449));
#54284=CARTESIAN_POINT('Ctrl Pts',(117.38636,11.209410806186,4.29192801665162));
#54285=CARTESIAN_POINT('Ctrl Pts',(117.38636,11.138268112713,4.45021599479794));
#54286=CARTESIAN_POINT('Ctrl Pts',(117.38636,11.1166612236889,4.49828995166837));
#54287=CARTESIAN_POINT('Ctrl Pts',(117.38636,11.0947337121375,4.54623664889386));
#54288=CARTESIAN_POINT('Ctrl Pts',(117.38636,11.072486547347,4.59405262188719));
#54289=CARTESIAN_POINT('Ctrl Pts',(117.38636,11.0566186236401,4.62815765138553));
#54290=CARTESIAN_POINT('Ctrl Pts',(117.38636,11.0405865692041,4.66219923462761));
#54291=CARTESIAN_POINT('Ctrl Pts',(117.38636,11.0244019262929,4.69615293251817));
#54292=CARTESIAN_POINT('Ctrl Pts',(117.38636,10.9021816861498,4.95255828744005));
#54293=CARTESIAN_POINT('Ctrl Pts',(117.38636,10.7711447000552,5.20421392423024));
#54294=CARTESIAN_POINT('Ctrl Pts',(117.38636,10.6315896890138,5.45066746458217));
#54295=CARTESIAN_POINT('Ctrl Pts',(117.38636,10.491931120956,5.69730388617308));
#54296=CARTESIAN_POINT('Ctrl Pts',(117.38636,10.3437415528983,5.93873103356036));
#54297=CARTESIAN_POINT('Ctrl Pts',(117.38636,10.1872735402806,6.17447234971671));
#54298=CARTESIAN_POINT('Ctrl Pts',(117.38636,10.0322804114542,6.40799154366195));
#54299=CARTESIAN_POINT('Ctrl Pts',(117.38636,9.86916379395795,6.63593206668975));
#54300=CARTESIAN_POINT('Ctrl Pts',(117.38636,9.69812859331579,6.85780045134778));
#54301=CARTESIAN_POINT('Ctrl Pts',(117.38636,9.5309508879448,7.07466485880448));
#54302=CARTESIAN_POINT('Ctrl Pts',(117.38636,9.3562073581532,7.28572828240745));
#54303=CARTESIAN_POINT('Ctrl Pts',(117.38636,9.1740562320771,7.4904949660174));
#54304=CARTESIAN_POINT('Ctrl Pts',(117.38636,9.01491680449495,7.6693928598683));
#54305=CARTESIAN_POINT('Ctrl Pts',(117.38636,8.85012236963218,7.84348396232437));
#54306=CARTESIAN_POINT('Ctrl Pts',(117.38636,8.67992675680234,8.01255267463112));
#54307=CARTESIAN_POINT('Ctrl Pts',(117.38636,8.60546617618929,8.08652023626532));
#54308=CARTESIAN_POINT('Ctrl Pts',(117.38636,8.52997160945683,8.15952617938624));
#54309=CARTESIAN_POINT('Ctrl Pts',(117.38636,8.45346361051115,8.23155099082254));
#54310=CARTESIAN_POINT('Ctrl Pts',(117.38636,8.42152310743143,8.26161985608107));
#54311=CARTESIAN_POINT('Ctrl Pts',(117.38636,8.38940596978659,8.29151770990631));
#54312=CARTESIAN_POINT('Ctrl Pts',(117.38636,8.35711367457556,8.32124308435686));
#54313=CARTESIAN_POINT('Ctrl Pts',(117.38636,8.33422258085946,8.34231456062843));
#54314=CARTESIAN_POINT('Ctrl Pts',(117.38636,8.31124267485234,8.36330003679656));
#54315=CARTESIAN_POINT('Ctrl Pts',(117.38636,8.28818716392733,8.38418763817203));
#54316=CARTESIAN_POINT('Ctrl Pts',(117.38636,8.0816610990473,8.57129405845009));
#54317=CARTESIAN_POINT('Ctrl Pts',(117.38636,7.86883968089771,8.75076473777949));
#54318=CARTESIAN_POINT('Ctrl Pts',(117.38636,7.65020289170389,8.92236157727182));
#54319=CARTESIAN_POINT('Ctrl Pts',(117.38636,7.43004610510815,9.09515138502521));
#54320=CARTESIAN_POINT('Ctrl Pts',(117.38636,7.2039922968932,9.25995785654159));
#54321=CARTESIAN_POINT('Ctrl Pts',(117.38636,6.97249670012354,9.41649834374283));
#54322=CARTESIAN_POINT('Ctrl Pts',(117.38636,6.74151605838306,9.57269061131363));
#54323=CARTESIAN_POINT('Ctrl Pts',(117.38636,6.50511726314233,9.72065393525675));
#54324=CARTESIAN_POINT('Ctrl Pts',(117.38636,6.26372598957658,9.86006336558048));
#54325=CARTESIAN_POINT('Ctrl Pts',(117.38636,6.02418010005166,9.99840704098249));
#54326=CARTESIAN_POINT('Ctrl Pts',(117.38636,5.77971723647088,10.1283273663033));
#54327=CARTESIAN_POINT('Ctrl Pts',(117.38636,5.53073534339514,10.2494590853848));
#54328=CARTESIAN_POINT('Ctrl Pts',(117.38636,5.28612776267642,10.3684626658734));
#54329=CARTESIAN_POINT('Ctrl Pts',(117.38636,5.03715804284583,10.478983895787));
#54330=CARTESIAN_POINT('Ctrl Pts',(117.38636,4.78419373222444,10.5806272791542));
#54331=CARTESIAN_POINT('Ctrl Pts',(117.38636,4.68063194659597,10.6222393557866));
#54332=CARTESIAN_POINT('Ctrl Pts',(117.38636,4.57640058419126,10.6623628910523));
#54333=CARTESIAN_POINT('Ctrl Pts',(117.38636,4.47152467205382,10.7009682121205));
#54334=CARTESIAN_POINT('Ctrl Pts',(117.218885227957,1.68953572661212,-12.4994363787171));
#54335=CARTESIAN_POINT('Ctrl Pts',(117.234294788862,2.3567517695111,-12.4097921526067));
#54336=CARTESIAN_POINT('Ctrl Pts',(117.249704349766,3.01671750224669,-12.267108816008));
#54337=CARTESIAN_POINT('Ctrl Pts',(117.26511391067,3.66073026855528,-12.0718164881636));
#54338=CARTESIAN_POINT('Ctrl Pts',(117.30552927378,5.34981212877998,-11.559614330598));
#54339=CARTESIAN_POINT('Ctrl Pts',(117.34594463689,6.92915678414743,-10.6855256438983));
#54340=CARTESIAN_POINT('Ctrl Pts',(117.38636,8.26387335187462,-9.53028995448217));
#54341=CARTESIAN_POINT('Ctrl Pts',(95.8594371265034,-5.05456119273957,10.438230919004));
#54342=CARTESIAN_POINT('Ctrl Pts',(95.9067535451842,-6.76502131585771,9.60996553312322));
#54343=CARTESIAN_POINT('Ctrl Pts',(96.001386382546,-9.76939938124694,7.09734914354963));
#54344=CARTESIAN_POINT('Ctrl Pts',(96.1433356385887,-11.962745016736,1.64472530342245));
#54345=CARTESIAN_POINT('Ctrl Pts',(96.2852848946312,-11.3224897112199,-4.19650321983491));
#54346=CARTESIAN_POINT('Ctrl Pts',(96.427234150674,-8.00081238047729,-9.04430323897844));
#54347=CARTESIAN_POINT('Ctrl Pts',(96.5691834067165,-2.78415884399867,-11.7498524979654));
#54348=CARTESIAN_POINT('Ctrl Pts',(96.7111326627592,3.091848831559,-11.6726995174351));
#54349=CARTESIAN_POINT('Ctrl Pts',(96.8530819188018,8.23560924484923,-8.83096106044612));
#54350=CARTESIAN_POINT('Ctrl Pts',(96.9950311748445,11.4288580805009,-3.8977427059358));
#54351=CARTESIAN_POINT('Ctrl Pts',(97.136980430887,11.915327242442,1.95861959274003));
#54352=CARTESIAN_POINT('Ctrl Pts',(97.2789296869297,9.5797960279637,7.35110139990983));
#54353=CARTESIAN_POINT('Ctrl Pts',(97.4208789429723,4.97540930776886,11.0025682116464));
#54354=CARTESIAN_POINT('Ctrl Pts',(97.562828199015,-0.807342216722395,12.0482111751727));
#54355=CARTESIAN_POINT('Ctrl Pts',(97.7047774550576,-6.39888446344168,10.2403845654334));
#54356=CARTESIAN_POINT('Ctrl Pts',(97.8467267111003,-10.474929971616,6.00724889591607));
#54357=CARTESIAN_POINT('Ctrl Pts',(97.9886759671429,-12.0701174780218,0.351370572132009));
#54358=CARTESIAN_POINT('Ctrl Pts',(98.1306252231855,-10.8066465790285,-5.38772560594593));
#54359=CARTESIAN_POINT('Ctrl Pts',(98.2725744792281,-6.98375473307958,-9.85080540269698));
#54360=CARTESIAN_POINT('Ctrl Pts',(98.4145237352708,-1.50684673412838,-11.9808434723489));
#54361=CARTESIAN_POINT('Ctrl Pts',(98.5564729913134,4.32693932863066,-11.2733665501931));
#54362=CARTESIAN_POINT('Ctrl Pts',(98.6984222473561,9.13594318590594,-7.89593182926991));
#54363=CARTESIAN_POINT('Ctrl Pts',(98.8403715033986,11.781211598614,-2.64844305476444));
#54364=CARTESIAN_POINT('Ctrl Pts',(98.9823207594414,11.6362453734974,3.22629678599122));
#54365=CARTESIAN_POINT('Ctrl Pts',(99.124270015484,8.73537797318143,8.33692803205455));
#54366=CARTESIAN_POINT('Ctrl Pts',(99.2662192715265,3.76564405694391,11.4730607154675));
#54367=CARTESIAN_POINT('Ctrl Pts',(99.4081685275693,-2.0959362022484,11.8919404968782));
#54368=CARTESIAN_POINT('Ctrl Pts',(99.5501177836118,-7.46111982681854,9.49436086710135));
#54369=CARTESIAN_POINT('Ctrl Pts',(99.6920670396545,-11.0592292586176,4.84815898566623));
#54370=CARTESIAN_POINT('Ctrl Pts',(99.8340162956972,-12.0380966639746,-0.946269546045479));
#54371=CARTESIAN_POINT('Ctrl Pts',(99.9759655517397,-10.1658893729505,-6.51658580867914));
#54372=CARTESIAN_POINT('Ctrl Pts',(100.117914807782,-5.88601658741872,-10.5435291092497));
#54373=CARTESIAN_POINT('Ctrl Pts',(100.259864063825,-0.212113381356825,
-12.0733676022228));
#54374=CARTESIAN_POINT('Ctrl Pts',(100.401813319868,5.51202626250981,-10.7437779121853));
#54375=CARTESIAN_POINT('Ctrl Pts',(100.54376257591,9.93071048086492,-6.8696569557873));
#54376=CARTESIAN_POINT('Ctrl Pts',(100.685711831953,11.997428424203,-1.36854249151505));
#54377=CARTESIAN_POINT('Ctrl Pts',(100.827661087996,11.2227034420802,4.45669437992771));
#54378=CARTESIAN_POINT('Ctrl Pts',(100.969610344038,7.7900195897285,9.22641816397909));
#54379=CARTESIAN_POINT('Ctrl Pts',(101.111559600081,2.51236569298111,11.8109786203214));
#54380=CARTESIAN_POINT('Ctrl Pts',(101.253508856124,-3.3603110263314,11.5982544872611));
#54381=CARTESIAN_POINT('Ctrl Pts',(101.395458112166,-8.43713953088349,8.63862685161016));
#54382=CARTESIAN_POINT('Ctrl Pts',(101.537407368209,-11.5157356156619,3.63304700976087));
#54383=CARTESIAN_POINT('Ctrl Pts',(101.679356624251,-11.866971774659,-2.23297520013184));
#54384=CARTESIAN_POINT('Ctrl Pts',(101.821305880294,-9.40766205636401,-7.57014477921035));
#54385=CARTESIAN_POINT('Ctrl Pts',(101.963255136337,-4.72026363022087,-11.1144189504522));
#54386=CARTESIAN_POINT('Ctrl Pts',(102.105204392379,1.08507100893144,-12.0263800975411));
#54387=CARTESIAN_POINT('Ctrl Pts',(102.247153648422,6.63341996474086,-10.0900414724784));
#54388=CARTESIAN_POINT('Ctrl Pts',(102.389102904465,10.610725229854,-5.76400099249621));
#54389=CARTESIAN_POINT('Ctrl Pts',(102.531052160507,12.0750111151176,-0.0728279804925511));
#54390=CARTESIAN_POINT('Ctrl Pts',(102.67300141655,10.6794795716148,5.63559344030584));
#54391=CARTESIAN_POINT('Ctrl Pts',(102.814950672592,6.75464503055027,10.0092940738206));
#54392=CARTESIAN_POINT('Ctrl Pts',(102.956899928635,1.23005613734974,12.0124168777114));
#54393=CARTESIAN_POINT('Ctrl Pts',(103.098849184678,-4.58585637836471,11.1705469258209));
#54394=CARTESIAN_POINT('Ctrl Pts',(103.24079844072,-9.31566538066349,7.68307073119021));
#54395=CARTESIAN_POINT('Ctrl Pts',(103.382747696763,-11.8391739529085,2.37595401001747));
#54396=CARTESIAN_POINT('Ctrl Pts',(103.524696952806,-11.5587202190389,-3.49387810934367));
#54397=CARTESIAN_POINT('Ctrl Pts',(103.666646208848,-8.54072618632016,-8.53622829798181));
#54398=CARTESIAN_POINT('Ctrl Pts',(103.808595464891,-3.49996651231003,-11.5568781146813));
#54399=CARTESIAN_POINT('Ctrl Pts',(103.950544720934,2.36971705558015,-11.8404239122457));
#54400=CARTESIAN_POINT('Ctrl Pts',(104.092493976976,7.67816237096933,-9.3197113662083));
#54401=CARTESIAN_POINT('Ctrl Pts',(104.234443233019,11.168129644454,-4.59174014842598));
#54402=CARTESIAN_POINT('Ctrl Pts',(104.376392489061,12.0130631783326,1.22372808128535));
#54403=CARTESIAN_POINT('Ctrl Pts',(104.518341745104,10.0128508883889,6.74937141017876));
#54404=CARTESIAN_POINT('Ctrl Pts',(104.660291001147,5.64121838056578,10.6765093795372));
#54405=CARTESIAN_POINT('Ctrl Pts',(104.802240257189,-0.0664671110029323,
12.0750478032933));
#54406=CARTESIAN_POINT('Ctrl Pts',(104.944189513232,-5.75841068985474,10.6137601120454));
#54407=CARTESIAN_POINT('Ctrl Pts',(105.086138769275,-10.0865457254805,6.63873426049027));
#54408=CARTESIAN_POINT('Ctrl Pts',(105.228088025317,-12.0258068420377,1.09140610544123));
#54409=CARTESIAN_POINT('Ctrl Pts',(105.37003728136,-11.1169039314122,-4.71440814863962));
#54410=CARTESIAN_POINT('Ctrl Pts',(105.511986537402,-7.57509950853803,-9.40367293367282));
#54411=CARTESIAN_POINT('Ctrl Pts',(105.653935793445,-2.23922610928576,-11.8657938991006));
#54412=CARTESIAN_POINT('Ctrl Pts',(105.795885049488,3.6269801590525,-11.5176477156709));
#54413=CARTESIAN_POINT('Ctrl Pts',(105.93783430553,8.63418136051829,-8.44168924241129));
#54414=CARTESIAN_POINT('Ctrl Pts',(106.079783561573,11.5964822941979,-3.36641977915706));
#54415=CARTESIAN_POINT('Ctrl Pts',(106.221732817616,11.8123013659403,2.50614254258396));
#54416=CARTESIAN_POINT('Ctrl Pts',(106.363682073658,9.23051857694247,7.78516037256956));
#54417=CARTESIAN_POINT('Ctrl Pts',(106.505631329701,4.46260964811663,11.2203497277713));
#54418=CARTESIAN_POINT('Ctrl Pts',(106.647580585744,-1.36223065258046,11.9981569780826));
#54419=CARTESIAN_POINT('Ctrl Pts',(106.789529841786,-6.86440734641473,9.9343085302927));
#54420=CARTESIAN_POINT('Ctrl Pts',(106.931479097829,-10.7409089746491,5.51772545751394));
#54421=CARTESIAN_POINT('Ctrl Pts',(107.073428353871,-12.0734023240826,-0.205836963644071));
#54422=CARTESIAN_POINT('Ctrl Pts',(107.215377609914,-10.5467853781223,-5.88028127277808));
#54423=CARTESIAN_POINT('Ctrl Pts',(107.357326865957,-6.5216081564048,-10.1627828959428));
#54424=CARTESIAN_POINT('Ctrl Pts',(107.451959703319,-2.80945746568101,-11.4115686783349));
#54425=CARTESIAN_POINT('Ctrl Pts',(107.499276121999,-0.914933857717795,
-11.5614942635285));
#54426=CARTESIAN_POINT('Ctrl Pts',(96.0549664176689,-5.20216116916647,10.7430412831157));
#54427=CARTESIAN_POINT('Ctrl Pts',(96.1022828363498,-6.96256902547539,9.89058943538993));
#54428=CARTESIAN_POINT('Ctrl Pts',(96.1969156737116,-10.0546789660402,7.30460127213921));
#54429=CARTESIAN_POINT('Ctrl Pts',(96.3388649297541,-12.312073240323,1.69275349157906));
#54430=CARTESIAN_POINT('Ctrl Pts',(96.4808141857969,-11.6531216198553,-4.3190467508565));
#54431=CARTESIAN_POINT('Ctrl Pts',(96.6227634418394,-8.23444684917279,-9.30840904242357));
#54432=CARTESIAN_POINT('Ctrl Pts',(96.7647126978821,-2.86546002209765,-12.0929639740338));
#54433=CARTESIAN_POINT('Ctrl Pts',(96.9066619539248,3.1821349706029,-12.0135580228354));
#54434=CARTESIAN_POINT('Ctrl Pts',(97.0486112099673,8.47610009737803,-9.08883698570373));
#54435=CARTESIAN_POINT('Ctrl Pts',(97.19056046601,11.7625960883999,-4.01156202863798));
#54436=CARTESIAN_POINT('Ctrl Pts',(97.3325097220526,12.2632708033251,2.01581391578688));
#54437=CARTESIAN_POINT('Ctrl Pts',(97.4744589780952,9.85953894015421,7.56576343524082));
#54438=CARTESIAN_POINT('Ctrl Pts',(97.6164082341379,5.12069794283293,11.3238579827559));
#54439=CARTESIAN_POINT('Ctrl Pts',(97.7583574901805,-0.830917693922621,
12.4000351253895));
#54440=CARTESIAN_POINT('Ctrl Pts',(97.9003067462231,-6.58574048515116,10.5394175502613));
#54441=CARTESIAN_POINT('Ctrl Pts',(98.0422560022659,-10.7808119973604,6.18266863298474));
#54442=CARTESIAN_POINT('Ctrl Pts',(98.1842052583084,-12.4225811217076,0.361631064820941));
#54443=CARTESIAN_POINT('Ctrl Pts',(98.3261545143511,-11.1222151752916,-5.54505443076548));
#54444=CARTESIAN_POINT('Ctrl Pts',(98.4681037703937,-7.1876897522964,-10.1384621526662));
#54445=CARTESIAN_POINT('Ctrl Pts',(98.6100530264363,-1.55084868285458,-12.3307001951508));
#54446=CARTESIAN_POINT('Ctrl Pts',(98.7520022824789,4.45329176923893,-11.6025639965412));
#54447=CARTESIAN_POINT('Ctrl Pts',(98.8939515385216,9.40272499889778,-8.12650364498813));
#54448=CARTESIAN_POINT('Ctrl Pts',(99.0359007945642,12.125238802545,-2.72578114951593));
#54449=CARTESIAN_POINT('Ctrl Pts',(99.1778500506069,11.9760393689273,3.32050898590334));
#54450=CARTESIAN_POINT('Ctrl Pts',(99.3197993066495,8.99046274389779,8.58037752926741));
#54451=CARTESIAN_POINT('Ctrl Pts',(99.4617485626922,3.87560592165246,11.8080894996832));
#54452=CARTESIAN_POINT('Ctrl Pts',(99.6036978187347,-2.15714035474506,12.2392011333763));
#54453=CARTESIAN_POINT('Ctrl Pts',(99.7456470747775,-7.67899454799881,9.77160895783289));
#54454=CARTESIAN_POINT('Ctrl Pts',(99.8875963308201,-11.3821736084093,4.98973174039441));
#54455=CARTESIAN_POINT('Ctrl Pts',(100.029545586863,-12.389625256878,-0.973901887877716));
#54456=CARTESIAN_POINT('Ctrl Pts',(100.171494842905,-10.4627469980914,-6.70687886777328));
#54457=CARTESIAN_POINT('Ctrl Pts',(100.313444098948,-6.05789617823254,-10.8514143219596));
#54458=CARTESIAN_POINT('Ctrl Pts',(100.455393354991,-0.218307377016261,
-12.4259261539011));
#54459=CARTESIAN_POINT('Ctrl Pts',(100.597342611033,5.67298483346935,-11.0575106589274));
#54460=CARTESIAN_POINT('Ctrl Pts',(100.739291867076,10.2207005664501,-7.07026016664399));
#54461=CARTESIAN_POINT('Ctrl Pts',(100.881241123118,12.3477694498769,-1.40850577057814));
#54462=CARTESIAN_POINT('Ctrl Pts',(101.023190379161,11.5504214576176,4.58683584232886));
#54463=CARTESIAN_POINT('Ctrl Pts',(101.165139635204,8.01749862578424,9.49584196786224));
#54464=CARTESIAN_POINT('Ctrl Pts',(101.307088891246,2.58573014598101,12.155875061271));
#54465=CARTESIAN_POINT('Ctrl Pts',(101.449038147289,-3.45843662207766,11.9369390977812));
#54466=CARTESIAN_POINT('Ctrl Pts',(101.590987403332,-8.68351533847242,8.89088635961457));
#54467=CARTESIAN_POINT('Ctrl Pts',(101.732936659374,-11.8520105642869,3.73913686257913));
#54468=CARTESIAN_POINT('Ctrl Pts',(101.874885915417,-12.2135032909288,-2.29818107544593));
#54469=CARTESIAN_POINT('Ctrl Pts',(102.01683517146,-9.68237842536282,-7.79120317544952));
#54470=CARTESIAN_POINT('Ctrl Pts',(102.158784427502,-4.85810166877311,-11.4389749133797));
#54471=CARTESIAN_POINT('Ctrl Pts',(102.300733683545,1.11675653992664,-12.3775665509662));
#54472=CARTESIAN_POINT('Ctrl Pts',(102.442682939587,6.82712473813086,-10.384684237042));
#54473=CARTESIAN_POINT('Ctrl Pts',(102.58463219563,10.9205726595475,-5.93231756403941));
#54474=CARTESIAN_POINT('Ctrl Pts',(102.726581451673,12.4276176595801,-0.0749546553499881));
#54475=CARTESIAN_POINT('Ctrl Pts',(102.868530707715,10.9913347204428,5.80016033884008));
#54476=CARTESIAN_POINT('Ctrl Pts',(103.010479963758,6.95188973869892,10.3015789058784));
#54477=CARTESIAN_POINT('Ctrl Pts',(103.152429219801,1.26597542884778,12.3631955863612));
#54478=CARTESIAN_POINT('Ctrl Pts',(103.294378475843,-4.71976954461859,11.4967419010237));
#54479=CARTESIAN_POINT('Ctrl Pts',(103.436327731886,-9.58769532315621,7.90742671691631));
#54480=CARTESIAN_POINT('Ctrl Pts',(103.578276987929,-12.1848937354434,2.44533505863823));
#54481=CARTESIAN_POINT('Ctrl Pts',(103.720226243971,-11.8962503758221,-3.59590404332945));
#54482=CARTESIAN_POINT('Ctrl Pts',(103.862175500014,-8.79012686339186,-8.78549763067218));
#54483=CARTESIAN_POINT('Ctrl Pts',(104.004124756056,-3.60217023584078,-11.8943544795427));
#54484=CARTESIAN_POINT('Ctrl Pts',(104.146074012099,2.43891597675345,-12.1861801952723));
#54485=CARTESIAN_POINT('Ctrl Pts',(104.288023268142,7.90237502598375,-9.59185945691376));
#54486=CARTESIAN_POINT('Ctrl Pts',(104.429972524184,11.4942540317939,-4.72582512866913));
#54487=CARTESIAN_POINT('Ctrl Pts',(104.571921780227,12.3638607598287,1.25946258504604));
#54488=CARTESIAN_POINT('Ctrl Pts',(104.71387103627,10.3052395842098,6.94646212152869));
#54489=CARTESIAN_POINT('Ctrl Pts',(104.855820292312,5.80594953491142,10.9882777947668));
#54490=CARTESIAN_POINT('Ctrl Pts',(104.997769548355,-0.0684080399269323,
12.4276554190998));
#54491=CARTESIAN_POINT('Ctrl Pts',(105.139718804398,-5.92656401705154,10.9236961643755));
#54492=CARTESIAN_POINT('Ctrl Pts',(105.28166806044,-10.3810864095359,6.83259421845467));
#54493=CARTESIAN_POINT('Ctrl Pts',(105.423617316483,-12.376976555632,1.12327662976425));
#54494=CARTESIAN_POINT('Ctrl Pts',(105.565566572526,-11.4415324591217,-4.85207519926421));
#54495=CARTESIAN_POINT('Ctrl Pts',(105.707515828568,-7.79630258952909,-9.6782728149306));
#54496=CARTESIAN_POINT('Ctrl Pts',(105.849465084611,-2.30461451954379,-12.2122910198219));
#54497=CARTESIAN_POINT('Ctrl Pts',(105.991414340653,3.73289285168067,-11.8539785001846));
#54498=CARTESIAN_POINT('Ctrl Pts',(106.133363596696,8.88631105421133,-8.68819790768832));
#54499=CARTESIAN_POINT('Ctrl Pts',(106.275312852739,11.9351151543,-3.46472375869151));
#54500=CARTESIAN_POINT('Ctrl Pts',(106.417262108781,12.1572364328389,2.57932527123291));
#54501=CARTESIAN_POINT('Ctrl Pts',(106.559211364824,9.5000621183921,8.01249751295703));
#54502=CARTESIAN_POINT('Ctrl Pts',(106.701160620867,4.59292384429468,11.5479990116893));
#54503=CARTESIAN_POINT('Ctrl Pts',(106.843109876909,-1.40200961746818,12.3485192785084));
#54504=CARTESIAN_POINT('Ctrl Pts',(106.985059132952,-7.06485726162612,10.2244036837543));
#54505=CARTESIAN_POINT('Ctrl Pts',(107.127008388994,-11.0545579445614,5.67885045262314));
#54506=CARTESIAN_POINT('Ctrl Pts',(107.268957645037,-12.4259618896858,-0.211847679475389));
#54507=CARTESIAN_POINT('Ctrl Pts',(107.41090690108,-10.8547656782573,-6.05199338470034));
#54508=CARTESIAN_POINT('Ctrl Pts',(107.552856157122,-6.71204787479888,-10.4595498077822));
#54509=CARTESIAN_POINT('Ctrl Pts',(107.647488994484,-2.89149739751578,-11.7448018124665));
#54510=CARTESIAN_POINT('Ctrl Pts',(107.694805413165,-0.941651155358861,
-11.899105426137));
#54511=CARTESIAN_POINT('Ctrl Pts',(96.2504957088345,-5.34976114559336,11.0478516472273));
#54512=CARTESIAN_POINT('Ctrl Pts',(96.2978121275154,-7.16011673509306,10.1712133376566));
#54513=CARTESIAN_POINT('Ctrl Pts',(96.3924449648771,-10.3399585508335,7.51185340072878));
#54514=CARTESIAN_POINT('Ctrl Pts',(96.5343942209198,-12.6614014639099,1.74078167973567));
#54515=CARTESIAN_POINT('Ctrl Pts',(96.6763434769622,-11.9837535284907,-4.44159028187809));
#54516=CARTESIAN_POINT('Ctrl Pts',(96.8182927330052,-8.46808131786831,-9.57251484586868));
#54517=CARTESIAN_POINT('Ctrl Pts',(96.9602419890475,-2.94676120019661,-12.4360754501023));
#54518=CARTESIAN_POINT('Ctrl Pts',(97.1021912450904,3.2724211096468,-12.3544165282358));
#54519=CARTESIAN_POINT('Ctrl Pts',(97.2441405011329,8.71659094990683,-9.34671291096133));
#54520=CARTESIAN_POINT('Ctrl Pts',(97.3860897571755,12.0963340962989,-4.12538135134016));
#54521=CARTESIAN_POINT('Ctrl Pts',(97.5280390132182,12.6112143642082,2.07300823883373));
#54522=CARTESIAN_POINT('Ctrl Pts',(97.6699882692608,10.1392818523447,7.7804254705718));
#54523=CARTESIAN_POINT('Ctrl Pts',(97.8119375253035,5.26598657789702,11.6451477538654));
#54524=CARTESIAN_POINT('Ctrl Pts',(97.9538867813461,-0.854493171122856,
12.7518590756063));
#54525=CARTESIAN_POINT('Ctrl Pts',(98.0958360373887,-6.77259650686064,10.8384505350893));
#54526=CARTESIAN_POINT('Ctrl Pts',(98.2377852934314,-11.0866940231047,6.35808837005341));
#54527=CARTESIAN_POINT('Ctrl Pts',(98.379734549474,-12.7750447653935,0.371891557509875));
#54528=CARTESIAN_POINT('Ctrl Pts',(98.5216838055166,-11.4377837715547,-5.70238325558503));
#54529=CARTESIAN_POINT('Ctrl Pts',(98.6636330615593,-7.39162477151322,-10.4261189026355));
#54530=CARTESIAN_POINT('Ctrl Pts',(98.8055823176019,-1.59485063158079,-12.6805569179526));
#54531=CARTESIAN_POINT('Ctrl Pts',(98.9475315736445,4.5796442098472,-11.9317614428894));
#54532=CARTESIAN_POINT('Ctrl Pts',(99.0894808296872,9.66950681188962,-8.35707546070634));
#54533=CARTESIAN_POINT('Ctrl Pts',(99.2314300857298,12.4692660064759,-2.80311924426744));
#54534=CARTESIAN_POINT('Ctrl Pts',(99.3733793417725,12.3158333643572,3.41472118581547));
#54535=CARTESIAN_POINT('Ctrl Pts',(99.5153285978151,9.24554751461416,8.82382702648026));
#54536=CARTESIAN_POINT('Ctrl Pts',(99.6572778538577,3.98556778636102,12.143118283899));
#54537=CARTESIAN_POINT('Ctrl Pts',(99.7992271099004,-2.21834450724171,12.5864617698744));
#54538=CARTESIAN_POINT('Ctrl Pts',(99.941176365943,-7.89686926917907,10.0488570485644));
#54539=CARTESIAN_POINT('Ctrl Pts',(100.083125621986,-11.7051179582011,5.1313044951226));
#54540=CARTESIAN_POINT('Ctrl Pts',(100.225074878028,-12.7411538497813,-1.00153422970996));
#54541=CARTESIAN_POINT('Ctrl Pts',(100.367024134071,-10.7596046232323,-6.89717192686741));
#54542=CARTESIAN_POINT('Ctrl Pts',(100.508973390114,-6.22977576904636,-11.1592995346694));
#54543=CARTESIAN_POINT('Ctrl Pts',(100.650922646156,-0.224501372675697,
-12.7784847055794));
#54544=CARTESIAN_POINT('Ctrl Pts',(100.792871902199,5.83394340442888,-11.3712434056696));
#54545=CARTESIAN_POINT('Ctrl Pts',(100.934821158242,10.5106906520353,-7.2708633775007));
#54546=CARTESIAN_POINT('Ctrl Pts',(101.076770414284,12.6981104755508,-1.44846904964124));
#54547=CARTESIAN_POINT('Ctrl Pts',(101.218719670327,11.8781394731551,4.71697730473001));
#54548=CARTESIAN_POINT('Ctrl Pts',(101.360668926369,8.24497766183999,9.76526577174539));
#54549=CARTESIAN_POINT('Ctrl Pts',(101.502618182412,2.65909459898092,12.5007715022207));
#54550=CARTESIAN_POINT('Ctrl Pts',(101.644567438455,-3.55656221782393,12.2756237083013));
#54551=CARTESIAN_POINT('Ctrl Pts',(101.786516694497,-8.92989114606135,9.14314586761896));
#54552=CARTESIAN_POINT('Ctrl Pts',(101.92846595054,-12.1882855129119,3.84522671539739));
#54553=CARTESIAN_POINT('Ctrl Pts',(102.070415206582,-12.5600348071986,-2.36338695076003));
#54554=CARTESIAN_POINT('Ctrl Pts',(102.212364462625,-9.95709479436164,-8.01226157168866));
#54555=CARTESIAN_POINT('Ctrl Pts',(102.354313718668,-4.99593970732534,-11.7635308763072));
#54556=CARTESIAN_POINT('Ctrl Pts',(102.49626297471,1.14844207092185,-12.7287530043913));
#54557=CARTESIAN_POINT('Ctrl Pts',(102.638212230753,7.02082951152085,-10.6793270016055));
#54558=CARTESIAN_POINT('Ctrl Pts',(102.780161486796,11.230420089241,-6.1006341355826));
#54559=CARTESIAN_POINT('Ctrl Pts',(102.922110742838,12.7802242040426,-0.0770813302074385));
#54560=CARTESIAN_POINT('Ctrl Pts',(103.064059998881,11.3031898692709,5.96472723737434));
#54561=CARTESIAN_POINT('Ctrl Pts',(103.206009254924,7.14913444684757,10.5938637379362));
#54562=CARTESIAN_POINT('Ctrl Pts',(103.347958510966,1.30189472034582,12.713974295011));
#54563=CARTESIAN_POINT('Ctrl Pts',(103.489907767009,-4.85368271087248,11.8229368762265));
#54564=CARTESIAN_POINT('Ctrl Pts',(103.631857023051,-9.85972526564893,8.13178270264242));
#54565=CARTESIAN_POINT('Ctrl Pts',(103.773806279094,-12.5306135179784,2.51471610725899));
#54566=CARTESIAN_POINT('Ctrl Pts',(103.915755535137,-12.2337805326052,-3.69792997731523));
#54567=CARTESIAN_POINT('Ctrl Pts',(104.057704791179,-9.03952754046357,-9.03476696336253));
#54568=CARTESIAN_POINT('Ctrl Pts',(104.199654047222,-3.70437395937153,-12.2318308444042));
#54569=CARTESIAN_POINT('Ctrl Pts',(104.341603303265,2.50811489792676,-12.5319364782989));
#54570=CARTESIAN_POINT('Ctrl Pts',(104.483552559307,8.12658768099816,-9.86400754761923));
#54571=CARTESIAN_POINT('Ctrl Pts',(104.62550181535,11.8203784191338,-4.85991010891227));
#54572=CARTESIAN_POINT('Ctrl Pts',(104.767451071393,12.7146583413247,1.29519708880673));
#54573=CARTESIAN_POINT('Ctrl Pts',(104.909400327435,10.5976282800308,7.14355283287862));
#54574=CARTESIAN_POINT('Ctrl Pts',(105.051349583478,5.97068068925705,11.3000462099963));
#54575=CARTESIAN_POINT('Ctrl Pts',(105.19329883952,-0.0703489688509323,
12.7802630349062));
#54576=CARTESIAN_POINT('Ctrl Pts',(105.335248095563,-6.09471734424833,11.2336322167057));
#54577=CARTESIAN_POINT('Ctrl Pts',(105.477197351606,-10.6756270935914,7.02645417641905));
#54578=CARTESIAN_POINT('Ctrl Pts',(105.619146607648,-12.7281462692263,1.15514715408727));
#54579=CARTESIAN_POINT('Ctrl Pts',(105.761095863691,-11.7661609868312,-4.9897422498888));
#54580=CARTESIAN_POINT('Ctrl Pts',(105.903045119734,-8.01750567052013,-9.95287269618837));
#54581=CARTESIAN_POINT('Ctrl Pts',(106.044994375776,-2.37000292980183,-12.5587881405432));
#54582=CARTESIAN_POINT('Ctrl Pts',(106.186943631819,3.83880554430886,-12.1903092846983));
#54583=CARTESIAN_POINT('Ctrl Pts',(106.328892887862,9.13844074790435,-8.93470657296535));
#54584=CARTESIAN_POINT('Ctrl Pts',(106.470842143904,12.2737480144022,-3.56302773822597));
#54585=CARTESIAN_POINT('Ctrl Pts',(106.612791399947,12.5021714997374,2.65250799988186));
#54586=CARTESIAN_POINT('Ctrl Pts',(106.754740655989,9.76960565984174,8.23983465334451));
#54587=CARTESIAN_POINT('Ctrl Pts',(106.896689912032,4.72323804047272,11.8756482956073));
#54588=CARTESIAN_POINT('Ctrl Pts',(107.038639168075,-1.4417885823559,12.6988815789343));
#54589=CARTESIAN_POINT('Ctrl Pts',(107.180588424117,-7.26530717683752,10.5144988372159));
#54590=CARTESIAN_POINT('Ctrl Pts',(107.32253768016,-11.3682069144738,5.83997544773233));
#54591=CARTESIAN_POINT('Ctrl Pts',(107.464486936203,-12.7785214552891,-0.217858395306709));
#54592=CARTESIAN_POINT('Ctrl Pts',(107.606436192245,-11.1627459783923,-6.22370549662259));
#54593=CARTESIAN_POINT('Ctrl Pts',(107.748385448288,-6.90248759319296,-10.7563167196217));
#54594=CARTESIAN_POINT('Ctrl Pts',(107.84301828565,-2.97353732935054,-12.078034946598));
#54595=CARTESIAN_POINT('Ctrl Pts',(107.890334704331,-0.968368452999927,
-12.2367165887455));
#54596=CARTESIAN_POINT('Ctrl Pts',(96.446025,-5.49736112202026,11.352662011339));
#54597=CARTESIAN_POINT('Ctrl Pts',(96.4933414186809,-7.35766444471074,10.4518372399234));
#54598=CARTESIAN_POINT('Ctrl Pts',(96.5879742560426,-10.6252381356268,7.71910552931836));
#54599=CARTESIAN_POINT('Ctrl Pts',(96.7299235120854,-13.0107296874969,1.78880986789227));
#54600=CARTESIAN_POINT('Ctrl Pts',(96.8718727681279,-12.3143854371262,-4.56413381289968));
#54601=CARTESIAN_POINT('Ctrl Pts',(97.0138220241706,-8.70171578656381,-9.8366206493138));
#54602=CARTESIAN_POINT('Ctrl Pts',(97.1557712802131,-3.02806237829558,-12.7791869261708));
#54603=CARTESIAN_POINT('Ctrl Pts',(97.2977205362559,3.36270724869071,-12.6952750336362));
#54604=CARTESIAN_POINT('Ctrl Pts',(97.4396697922984,8.95708180243563,-9.60458883621892));
#54605=CARTESIAN_POINT('Ctrl Pts',(97.5816190483411,12.4300721041979,-4.23920067404235));
#54606=CARTESIAN_POINT('Ctrl Pts',(97.7235683043837,12.9591579250913,2.13020256188059));
#54607=CARTESIAN_POINT('Ctrl Pts',(97.8655175604264,10.4190247645352,7.99508750590277));
#54608=CARTESIAN_POINT('Ctrl Pts',(98.007466816469,5.41127521296109,11.966437524975));
#54609=CARTESIAN_POINT('Ctrl Pts',(98.1494160725116,-0.878068648323085,
13.103683025823));
#54610=CARTESIAN_POINT('Ctrl Pts',(98.2913653285542,-6.95945252857012,11.1374835199173));
#54611=CARTESIAN_POINT('Ctrl Pts',(98.4333145845969,-11.3925760488491,6.53350810712207));
#54612=CARTESIAN_POINT('Ctrl Pts',(98.5752638406395,-13.1275084090793,0.38215205019881));
#54613=CARTESIAN_POINT('Ctrl Pts',(98.7172130966822,-11.7533523678177,-5.85971208040458));
#54614=CARTESIAN_POINT('Ctrl Pts',(98.8591623527249,-7.59555979073004,-10.7137756526047));
#54615=CARTESIAN_POINT('Ctrl Pts',(99.0011116087674,-1.63885258030699,-13.0304136407544));
#54616=CARTESIAN_POINT('Ctrl Pts',(99.1430608648101,4.70599665045546,-12.2609588892376));
#54617=CARTESIAN_POINT('Ctrl Pts',(99.2850101208528,9.93628862488146,-8.58764727642455));
#54618=CARTESIAN_POINT('Ctrl Pts',(99.4269593768953,12.8132932104068,-2.88045733901893));
#54619=CARTESIAN_POINT('Ctrl Pts',(99.5689086329381,12.6556273597872,3.50893338572759));
#54620=CARTESIAN_POINT('Ctrl Pts',(99.7108578889806,9.50063228533051,9.06727652369311));
#54621=CARTESIAN_POINT('Ctrl Pts',(99.8528071450232,4.09552965106957,12.4781470681147));
#54622=CARTESIAN_POINT('Ctrl Pts',(99.9947564010659,-2.27954865973836,12.9337224063726));
#54623=CARTESIAN_POINT('Ctrl Pts',(100.136705657109,-8.11474399035933,10.326105139296));
#54624=CARTESIAN_POINT('Ctrl Pts',(100.278654913151,-12.0280623079928,5.27287724985078));
#54625=CARTESIAN_POINT('Ctrl Pts',(100.420604169194,-13.0926824426846,-1.02916657154219));
#54626=CARTESIAN_POINT('Ctrl Pts',(100.562553425236,-11.0564622483732,-7.08746498596154));
#54627=CARTESIAN_POINT('Ctrl Pts',(100.704502681279,-6.40165535986017,-11.4671847473793));
#54628=CARTESIAN_POINT('Ctrl Pts',(100.846451937322,-0.230695368335135,
-13.1310432572577));
#54629=CARTESIAN_POINT('Ctrl Pts',(100.988401193364,5.99490197538842,-11.6849761524118));
#54630=CARTESIAN_POINT('Ctrl Pts',(101.130350449407,10.8006807376205,-7.4714665883574));
#54631=CARTESIAN_POINT('Ctrl Pts',(101.27229970545,13.0484515012247,-1.48843232870433));
#54632=CARTESIAN_POINT('Ctrl Pts',(101.414248961492,12.2058574886926,4.84711876713115));
#54633=CARTESIAN_POINT('Ctrl Pts',(101.556198217535,8.47245669789572,10.0346895756286));
#54634=CARTESIAN_POINT('Ctrl Pts',(101.698147473577,2.73245905198082,12.8456679431704));
#54635=CARTESIAN_POINT('Ctrl Pts',(101.84009672962,-3.6546878135702,12.6143083188215));
#54636=CARTESIAN_POINT('Ctrl Pts',(101.982045985663,-9.17626695365029,9.39540537562336));
#54637=CARTESIAN_POINT('Ctrl Pts',(102.123995241705,-12.5245604615368,3.95131656821565));
#54638=CARTESIAN_POINT('Ctrl Pts',(102.265944497748,-12.9065663234684,-2.42859282607413));
#54639=CARTESIAN_POINT('Ctrl Pts',(102.407893753791,-10.2318111633605,-8.23331996792782));
#54640=CARTESIAN_POINT('Ctrl Pts',(102.549843009833,-5.13377774587759,-12.0880868392347));
#54641=CARTESIAN_POINT('Ctrl Pts',(102.691792265876,1.18012760191706,-13.0799394578163));
#54642=CARTESIAN_POINT('Ctrl Pts',(102.833741521919,7.21453428491085,-10.9739697661691));
#54643=CARTESIAN_POINT('Ctrl Pts',(102.975690777961,11.5402675189345,-6.26895070712579));
#54644=CARTESIAN_POINT('Ctrl Pts',(103.117640034004,13.1328307485051,-0.0792080050648763));
#54645=CARTESIAN_POINT('Ctrl Pts',(103.259589290047,11.6150450180989,6.12929413590858));
#54646=CARTESIAN_POINT('Ctrl Pts',(103.401538546089,7.34637915499623,10.886148569994));
#54647=CARTESIAN_POINT('Ctrl Pts',(103.543487802132,1.33781401184385,13.0647530036607));
#54648=CARTESIAN_POINT('Ctrl Pts',(103.685437058174,-4.98759587712636,12.1491318514294));
#54649=CARTESIAN_POINT('Ctrl Pts',(103.827386314217,-10.1317552081416,8.35613868836854));
#54650=CARTESIAN_POINT('Ctrl Pts',(103.96933557026,-12.8763333005133,2.58409715587975));
#54651=CARTESIAN_POINT('Ctrl Pts',(104.111284826302,-12.5713106893884,-3.79995591130102));
#54652=CARTESIAN_POINT('Ctrl Pts',(104.253234082345,-9.28892821753527,-9.28403629605289));
#54653=CARTESIAN_POINT('Ctrl Pts',(104.395183338388,-3.80657768290228,-12.5693072092657));
#54654=CARTESIAN_POINT('Ctrl Pts',(104.53713259443,2.57731381910005,-12.8776927613255));
#54655=CARTESIAN_POINT('Ctrl Pts',(104.679081850473,8.35080033601259,-10.1361556383247));
#54656=CARTESIAN_POINT('Ctrl Pts',(104.821031106516,12.1465028064736,-4.99399508915542));
#54657=CARTESIAN_POINT('Ctrl Pts',(104.962980362558,13.0654559228208,1.33093159256742));
#54658=CARTESIAN_POINT('Ctrl Pts',(105.104929618601,10.8900169758518,7.34064354422855));
#54659=CARTESIAN_POINT('Ctrl Pts',(105.246878874643,6.13541184360268,11.6118146252259));
#54660=CARTESIAN_POINT('Ctrl Pts',(105.388828130686,-0.0722898977749296,
13.1328706507127));
#54661=CARTESIAN_POINT('Ctrl Pts',(105.530777386729,-6.26287067144513,11.5435682690358));
#54662=CARTESIAN_POINT('Ctrl Pts',(105.672726642771,-10.9701677776469,7.22031413438345));
#54663=CARTESIAN_POINT('Ctrl Pts',(105.814675898814,-13.0793159828206,1.18701767841028));
#54664=CARTESIAN_POINT('Ctrl Pts',(105.956625154857,-12.0907895145407,-5.12740930051339));
#54665=CARTESIAN_POINT('Ctrl Pts',(106.098574410899,-8.23870875151118,-10.2274725774461));
#54666=CARTESIAN_POINT('Ctrl Pts',(106.240523666942,-2.43539134005986,-12.9052852612645));
#54667=CARTESIAN_POINT('Ctrl Pts',(106.382472922984,3.94471823693704,-12.526640069212));
#54668=CARTESIAN_POINT('Ctrl Pts',(106.524422179027,9.39057044159739,-9.18121523824236));
#54669=CARTESIAN_POINT('Ctrl Pts',(106.66637143507,12.6123808745043,-3.66133171776043));
#54670=CARTESIAN_POINT('Ctrl Pts',(106.808320691112,12.8471065666359,2.72569072853082));
#54671=CARTESIAN_POINT('Ctrl Pts',(106.950269947155,10.0391492012914,8.46717179373198));
#54672=CARTESIAN_POINT('Ctrl Pts',(107.092219203198,4.85355223665076,12.2032975795253));
#54673=CARTESIAN_POINT('Ctrl Pts',(107.23416845924,-1.48156754724362,13.0492438793601));
#54674=CARTESIAN_POINT('Ctrl Pts',(107.376117715283,-7.46575709204891,10.8045939906775));
#54675=CARTESIAN_POINT('Ctrl Pts',(107.518066971325,-11.6818558843861,6.00110044284153));
#54676=CARTESIAN_POINT('Ctrl Pts',(107.660016227368,-13.1310810208923,-0.223869111138029));
#54677=CARTESIAN_POINT('Ctrl Pts',(107.801965483411,-11.4707262785273,-6.39541760854485));
#54678=CARTESIAN_POINT('Ctrl Pts',(107.943914739453,-7.09292731158704,-11.0530836314612));
#54679=CARTESIAN_POINT('Ctrl Pts',(108.038547576815,-3.05557726118531,-12.4112680807296));
#54680=CARTESIAN_POINT('Ctrl Pts',(108.085863995496,-0.995085750640993,
-12.574327751354));
#54681=CARTESIAN_POINT('',(97.1841636168587,-1.68935314531928,-12.5));
#54682=CARTESIAN_POINT('',(97.2617423708143,1.68935314531928,-12.5));
#54683=CARTESIAN_POINT('Ctrl Pts',(97.1841636168587,-1.68966879435806,-12.5001504794836));
#54684=CARTESIAN_POINT('Ctrl Pts',(97.1836617116955,-1.68048229176406,-12.500141503016));
#54685=CARTESIAN_POINT('Ctrl Pts',(97.1831655403902,-1.67129546732837,-12.500132520818));
#54686=CARTESIAN_POINT('Ctrl Pts',(97.182675107321,-1.66210830628068,-12.5001235359673));
#54687=CARTESIAN_POINT('Ctrl Pts',(97.1694300033715,-1.41399105901218,-12.4998808825057));
#54688=CARTESIAN_POINT('Ctrl Pts',(97.1603881541905,-1.16596021025893,-12.499638689875));
#54689=CARTESIAN_POINT('Ctrl Pts',(97.1556009301936,-0.917715246001572,
-12.4994457080315));
#54690=CARTESIAN_POINT('Ctrl Pts',(97.1535063791998,-0.809100788663271,
-12.4993612728113));
#54691=CARTESIAN_POINT('Ctrl Pts',(97.1522262993178,-0.700444678977253,
-12.4992860395109));
#54692=CARTESIAN_POINT('Ctrl Pts',(97.1517649931838,-0.591718942494721,
-12.4992227758313));
#54693=CARTESIAN_POINT('Ctrl Pts',(97.151012012177,-0.41424804301112,-12.4991195117606));
#54694=CARTESIAN_POINT('Ctrl Pts',(97.15244156732,-0.236852374547013,-12.4990485185025));
#54695=CARTESIAN_POINT('Ctrl Pts',(97.1560531749278,-0.0594127045311677,
-12.4990160668234));
#54696=CARTESIAN_POINT('Ctrl Pts',(97.1563224737121,-0.0461819517430822,
-12.4990136470706));
#54697=CARTESIAN_POINT('Ctrl Pts',(97.1566038939014,-0.0329514754057439,
-12.4990114386038));
#54698=CARTESIAN_POINT('Ctrl Pts',(97.1568974324251,-0.0197212262430592,
-12.4990094424722));
#54699=CARTESIAN_POINT('Ctrl Pts',(97.1569780844716,-0.0160861099501589,
-12.4990088940192));
#54700=CARTESIAN_POINT('Ctrl Pts',(97.1570596512777,-0.0124510142730335,
-12.499008361595));
#54701=CARTESIAN_POINT('Ctrl Pts',(97.1571421327746,-0.00881593818621189,
-12.4990078452187));
#54702=CARTESIAN_POINT('Ctrl Pts',(97.1571905860349,-0.00668053455459407,
-12.4990075418765));
#54703=CARTESIAN_POINT('Ctrl Pts',(97.157239354937,-0.00454513809380544,
-12.4990072440723));
#54704=CARTESIAN_POINT('Ctrl Pts',(97.1572884394683,-0.00240974851892736,
-12.4990069518098));
#54705=CARTESIAN_POINT('Ctrl Pts',(97.1573308177058,-0.000566111752699424,
-12.4990066994783));
#54706=CARTESIAN_POINT('Ctrl Pts',(97.157373431211,0.00127751961241762,
-12.4990064512776));
#54707=CARTESIAN_POINT('Ctrl Pts',(97.1574162799744,0.00312114570776404,
-12.4990062072099));
#54708=CARTESIAN_POINT('Ctrl Pts',(97.1574684636542,0.00536641922499062,
-12.4990059099704));
#54709=CARTESIAN_POINT('Ctrl Pts',(97.1575209962562,0.00761168460872278,
-12.499005618861));
#54710=CARTESIAN_POINT('Ctrl Pts',(97.1575738777611,0.00985694202133178,
-12.4990053338855));
#54711=CARTESIAN_POINT('Ctrl Pts',(97.1576736462671,0.014092940556016,-12.4990047962387));
#54712=CARTESIAN_POINT('Ctrl Pts',(97.1577746566296,0.0183289091899971,
-12.4990042804258));
#54713=CARTESIAN_POINT('Ctrl Pts',(97.1578769087305,0.0225648495757296,
-12.4990037864712));
#54714=CARTESIAN_POINT('Ctrl Pts',(97.1584593407123,0.0466929323328523,
-12.4990009728865));
#54715=CARTESIAN_POINT('Ctrl Pts',(97.1590820545152,0.0708198412374658,
-12.4989988687095));
#54716=CARTESIAN_POINT('Ctrl Pts',(97.1597450255452,0.0949458742036956,
-12.4989974770508));
#54717=CARTESIAN_POINT('Ctrl Pts',(97.1605926787677,0.125792636228222,-12.4989956977212));
#54718=CARTESIAN_POINT('Ctrl Pts',(97.1615061196423,0.15663715691193,-12.4989950834167));
#54719=CARTESIAN_POINT('Ctrl Pts',(97.1624852863278,0.187480056498351,-12.498995634938));
#54720=CARTESIAN_POINT('Ctrl Pts',(97.1673070823745,0.339362441268142,-12.4989983508425));
#54721=CARTESIAN_POINT('Ctrl Pts',(97.1737206661987,0.491141315565022,-12.4990296235006));
#54722=CARTESIAN_POINT('Ctrl Pts',(97.181714540668,0.642889198400638,-12.49908730495));
#54723=CARTESIAN_POINT('Ctrl Pts',(97.1943805598043,0.883328499177757,-12.4991786992227));
#54724=CARTESIAN_POINT('Ctrl Pts',(97.210992279406,1.12327169768875,-12.4993379199478));
#54725=CARTESIAN_POINT('Ctrl Pts',(97.231460625774,1.36298827907735,-12.4995363845337));
#54726=CARTESIAN_POINT('Ctrl Pts',(97.2407610752496,1.47191119417622,-12.4996265632819));
#54727=CARTESIAN_POINT('Ctrl Pts',(97.25085777569,1.58078667024217,-12.4997246141786));
#54728=CARTESIAN_POINT('Ctrl Pts',(97.2617423708143,1.68963646449083,-12.4998270697762));
#54729=CARTESIAN_POINT('',(96.446025,-5.49736112202046,11.3526620113389));
#54730=CARTESIAN_POINT('Ctrl Pts',(96.446025,-5.4973611220203,11.352662011339));
#54731=CARTESIAN_POINT('Ctrl Pts',(96.4933414186809,-7.35766444471076,10.4518372399233));
#54732=CARTESIAN_POINT('Ctrl Pts',(96.5406578373617,-8.9914512901688,9.08547138462084));
#54733=CARTESIAN_POINT('Ctrl Pts',(96.5879742560426,-10.2059266382095,7.41390584673193));
#54734=CARTESIAN_POINT('Ctrl Pts',(96.6352906747235,-11.4204019862502,5.742340308843));
#54735=CARTESIAN_POINT('Ctrl Pts',(96.6826070934045,-12.2155658368735,3.76557508836764));
#54736=CARTESIAN_POINT('Ctrl Pts',(96.7299235120853,-12.4970903871234,1.7183685313313));
#54737=CARTESIAN_POINT('Ctrl Pts',(96.7772399307662,-12.7786149373733,-0.328838025705044));
#54738=CARTESIAN_POINT('Ctrl Pts',(96.824556349447,-12.5465001872497,-2.44648591930237));
#54739=CARTESIAN_POINT('Ctrl Pts',(96.8718727681279,-11.8283312037609,-4.38405767217005));
#54740=CARTESIAN_POINT('Ctrl Pts',(96.9191891868088,-11.110162220272,-6.32162942503772));
#54741=CARTESIAN_POINT('Ctrl Pts',(96.9665056054897,-9.90593900341793,-8.07912503717576));
#54742=CARTESIAN_POINT('Ctrl Pts',(97.0138220241706,-8.35821849361283,-9.44830055605428));
#54743=CARTESIAN_POINT('Ctrl Pts',(97.0611384428514,-6.81049798380774,-10.8174760749328));
#54744=CARTESIAN_POINT('Ctrl Pts',(97.1084548615323,-4.91928018105167,-11.7983315005518));
#54745=CARTESIAN_POINT('Ctrl Pts',(97.1557712802132,-2.90854300850926,-12.2747738979388));
#54746=CARTESIAN_POINT('Ctrl Pts',(97.1652353924284,-2.50636036733103,-12.3700707196056));
#54747=CARTESIAN_POINT('Ctrl Pts',(97.1746995046436,-2.09939611424284,-12.4451874872138));
#54748=CARTESIAN_POINT('Ctrl Pts',(97.1841636168587,-1.68966879435857,-12.5001504794835));
#54749=CARTESIAN_POINT('',(96.446025,-7.10320028565243,-9.16786776036321));
#54750=CARTESIAN_POINT('Ctrl Pts',(96.446025,-7.10371691227606,-9.16818944635625));
#54751=CARTESIAN_POINT('Ctrl Pts',(96.446025,-7.30978227149857,-9.02256097481596));
#54752=CARTESIAN_POINT('Ctrl Pts',(96.446025,-7.51084480534185,-8.8703120063485));
#54753=CARTESIAN_POINT('Ctrl Pts',(96.446025,-7.70654954542632,-8.71164069364237));
#54754=CARTESIAN_POINT('Ctrl Pts',(96.446025,-7.92191546555672,-8.53702870803333));
#54755=CARTESIAN_POINT('Ctrl Pts',(96.446025,-8.13079395813826,-8.35463972061946));
#54756=CARTESIAN_POINT('Ctrl Pts',(96.446025,-8.33291957884125,-8.16495486798257));
#54757=CARTESIAN_POINT('Ctrl Pts',(96.446025,-8.4832417260981,-8.02388500137534));
#54758=CARTESIAN_POINT('Ctrl Pts',(96.446025,-8.62982836664002,-7.87877876499321));
#54759=CARTESIAN_POINT('Ctrl Pts',(96.446025,-8.77255919267182,-7.72981909737944));
#54760=CARTESIAN_POINT('Ctrl Pts',(96.446025,-8.84563001113479,-7.65355943341528));
#54761=CARTESIAN_POINT('Ctrl Pts',(96.446025,-8.91769009145714,-7.57628962582517));
#54762=CARTESIAN_POINT('Ctrl Pts',(96.446025,-8.98872220008187,-7.49803307925646));
#54763=CARTESIAN_POINT('Ctrl Pts',(96.446025,-9.03428838540755,-7.44783250978251));
#54764=CARTESIAN_POINT('Ctrl Pts',(96.446025,-9.07943153913389,-7.39722587640377));
#54765=CARTESIAN_POINT('Ctrl Pts',(96.446025,-9.12414693982324,-7.34621920411752));
#54766=CARTESIAN_POINT('Ctrl Pts',(96.446025,-9.15309102287457,-7.31320280851185));
#54767=CARTESIAN_POINT('Ctrl Pts',(96.446025,-9.18185686627777,-7.28001755106976));
#54768=CARTESIAN_POINT('Ctrl Pts',(96.446025,-9.21042952422747,-7.24668122873893));
#54769=CARTESIAN_POINT('Ctrl Pts',(96.446025,-9.39281579291678,-7.03388732442495));
#54770=CARTESIAN_POINT('Ctrl Pts',(96.446025,-9.56746197962767,-6.81479614168976));
#54771=CARTESIAN_POINT('Ctrl Pts',(96.446025,-9.73409922463371,-6.58989399404312));
#54772=CARTESIAN_POINT('Ctrl Pts',(96.446025,-9.90183700371478,-6.36350650932778));
#54773=CARTESIAN_POINT('Ctrl Pts',(96.446025,-10.0614601394372,-6.13123059900815));
#54774=CARTESIAN_POINT('Ctrl Pts',(96.446025,-10.2126589253177,-5.89352356979185));
#54775=CARTESIAN_POINT('Ctrl Pts',(96.446025,-10.3633936752713,-5.65654607422211));
#54776=CARTESIAN_POINT('Ctrl Pts',(96.446025,-10.5057560910357,-5.41417023874808));
#54777=CARTESIAN_POINT('Ctrl Pts',(96.446025,-10.6393980847918,-5.1668181108504));
#54778=CARTESIAN_POINT('Ctrl Pts',(96.446025,-10.6627641550139,-5.12357087225718));
#54779=CARTESIAN_POINT('Ctrl Pts',(96.446025,-10.6858635375631,-5.08017144590901));
#54780=CARTESIAN_POINT('Ctrl Pts',(96.446025,-10.7086942282531,-5.0366220075035));
#54781=CARTESIAN_POINT('Ctrl Pts',(96.446025,-10.727478568401,-5.00079096430983));
#54782=CARTESIAN_POINT('Ctrl Pts',(96.446025,-10.7460821600203,-4.96485601687245));
#54783=CARTESIAN_POINT('Ctrl Pts',(96.446025,-10.7644932211042,-4.92883954535707));
#54784=CARTESIAN_POINT('Ctrl Pts',(96.446025,-10.8987630685253,-4.66617537228287));
#54785=CARTESIAN_POINT('Ctrl Pts',(96.446025,-11.0229197835297,-4.39894687519522));
#54786=CARTESIAN_POINT('Ctrl Pts',(96.446025,-11.1366626238853,-4.12769733765066));
#54787=CARTESIAN_POINT('Ctrl Pts',(96.446025,-11.2450445015555,-3.86923241709514));
#54788=CARTESIAN_POINT('Ctrl Pts',(96.446025,-11.3439714533202,-3.60711590739578));
#54789=CARTESIAN_POINT('Ctrl Pts',(96.446025,-11.4334649925142,-3.34190306363835));
#54790=CARTESIAN_POINT('Ctrl Pts',(96.446025,-11.5238417961909,-3.0740726780187));
#54791=CARTESIAN_POINT('Ctrl Pts',(96.446025,-11.6045982489161,-2.80308398612925));
#54792=CARTESIAN_POINT('Ctrl Pts',(96.446025,-11.6757096849509,-2.52948279890396));
#54793=CARTESIAN_POINT('Ctrl Pts',(96.446025,-11.7471005597629,-2.25480647123063));
#54794=CARTESIAN_POINT('Ctrl Pts',(96.446025,-11.8087706245828,-1.97749647593278));
#54795=CARTESIAN_POINT('Ctrl Pts',(96.446025,-11.8606454191839,-1.69808769268104));
#54796=CARTESIAN_POINT('Ctrl Pts',(96.446025,-11.9117669507853,-1.42273614570025));
#54797=CARTESIAN_POINT('Ctrl Pts',(96.446025,-11.9533756270982,-1.1453457118012));
#54798=CARTESIAN_POINT('Ctrl Pts',(96.446025,-11.985351194423,-0.866420498375038));
#54799=CARTESIAN_POINT('Ctrl Pts',(96.446025,-11.9963079527002,-0.770843894217156));
#54800=CARTESIAN_POINT('Ctrl Pts',(96.446025,-12.0061332000131,-0.675087055171968));
#54801=CARTESIAN_POINT('Ctrl Pts',(96.446025,-12.0148207414527,-0.579170243646206));
#54802=CARTESIAN_POINT('Ctrl Pts',(96.446025,-12.0171896950221,-0.553015263596951));
#54803=CARTESIAN_POINT('Ctrl Pts',(96.446025,-12.0194738907792,-0.526849902756527));
#54804=CARTESIAN_POINT('Ctrl Pts',(96.446025,-12.0216724868579,-0.500684083298083));
#54805=CARTESIAN_POINT('Ctrl Pts',(96.446025,-12.0456996720184,-0.214732973353064));
#54806=CARTESIAN_POINT('Ctrl Pts',(96.446025,-12.0595364563262,0.071584871261912));
#54807=CARTESIAN_POINT('Ctrl Pts',(96.446025,-12.0631927104438,0.357708958361966));
#54808=CARTESIAN_POINT('Ctrl Pts',(96.446025,-12.0668701045469,0.645487377699364));
#54809=CARTESIAN_POINT('Ctrl Pts',(96.446025,-12.0602490557768,0.933070404419091));
#54810=CARTESIAN_POINT('Ctrl Pts',(96.446025,-12.0432896813139,1.21990410757687));
#54811=CARTESIAN_POINT('Ctrl Pts',(96.446025,-12.0347733144521,1.36394132131739));
#54812=CARTESIAN_POINT('Ctrl Pts',(96.446025,-12.0236491615489,1.50778977852785));
#54813=CARTESIAN_POINT('Ctrl Pts',(96.446025,-12.0099072778166,1.65138012858342));
#54814=CARTESIAN_POINT('Ctrl Pts',(96.446025,-11.9826587599829,1.93610268121525));
#54815=CARTESIAN_POINT('Ctrl Pts',(96.446025,-11.9451211361171,2.21981062774033));
#54816=CARTESIAN_POINT('Ctrl Pts',(96.446025,-11.8975263909157,2.50200891361867));
#54817=CARTESIAN_POINT('Ctrl Pts',(96.446025,-11.8497672155975,2.78518213689705));
#54818=CARTESIAN_POINT('Ctrl Pts',(96.446025,-11.7918811654255,3.06683584840972));
#54819=CARTESIAN_POINT('Ctrl Pts',(96.446025,-11.724050534956,3.34646281732963));
#54820=CARTESIAN_POINT('Ctrl Pts',(96.446025,-11.6817572389484,3.52081393402108));
#54821=CARTESIAN_POINT('Ctrl Pts',(96.446025,-11.6355967773695,3.69437694499245));
#54822=CARTESIAN_POINT('Ctrl Pts',(96.446025,-11.5856035149477,3.86702593820762));
#54823=CARTESIAN_POINT('Ctrl Pts',(96.446025,-11.570956641705,3.9176081126169));
#54824=CARTESIAN_POINT('Ctrl Pts',(96.446025,-11.5559807299102,3.9681118128852));
#54825=CARTESIAN_POINT('Ctrl Pts',(96.446025,-11.5406765247744,4.018533822066));
#54826=CARTESIAN_POINT('Ctrl Pts',(96.446025,-11.5313993558877,4.0490988524368));
#54827=CARTESIAN_POINT('Ctrl Pts',(96.446025,-11.5220010034243,4.07963561824385));
#54828=CARTESIAN_POINT('Ctrl Pts',(96.446025,-11.5124833492986,4.11013787574345));
#54829=CARTESIAN_POINT('Ctrl Pts',(96.446025,-11.4250037595175,4.39049319631259));
#54830=CARTESIAN_POINT('Ctrl Pts',(96.446025,-11.3276603568015,4.66726394819521));
#54831=CARTESIAN_POINT('Ctrl Pts',(96.446025,-11.2207605924677,4.93993847505352));
#54832=CARTESIAN_POINT('Ctrl Pts',(96.446025,-11.1145410184204,5.21087800683767));
#54833=CARTESIAN_POINT('Ctrl Pts',(96.446025,-10.998886044537,5.47777387765371));
#54834=CARTESIAN_POINT('Ctrl Pts',(96.446025,-10.8740437695655,5.74012050388206));
#54835=CARTESIAN_POINT('Ctrl Pts',(96.446025,-10.7480023299831,6.00498708410843));
#54836=CARTESIAN_POINT('Ctrl Pts',(96.446025,-10.6125961267233,6.26521724850586));
#54837=CARTESIAN_POINT('Ctrl Pts',(96.446025,-10.4680284180515,6.52027759435502));
#54838=CARTESIAN_POINT('Ctrl Pts',(96.446025,-10.3234607093797,6.77533794020419));
#54839=CARTESIAN_POINT('Ctrl Pts',(96.446025,-10.1697312994683,7.02522910650024));
#54840=CARTESIAN_POINT('Ctrl Pts',(96.446025,-10.0069941299641,7.26939502098643));
#54841=CARTESIAN_POINT('Ctrl Pts',(96.446025,-9.86517940602884,7.48216953256695));
#54842=CARTESIAN_POINT('Ctrl Pts',(96.446025,-9.71652325830122,7.69059612443967));
#54843=CARTESIAN_POINT('Ctrl Pts',(96.446025,-9.56129306948992,7.89443387712908));
#54844=CARTESIAN_POINT('Ctrl Pts',(96.446025,-9.49337986188497,7.9836128939307));
#54845=CARTESIAN_POINT('Ctrl Pts',(96.446025,-9.42420802625417,8.0719133244014));
#54846=CARTESIAN_POINT('Ctrl Pts',(96.446025,-9.3537985551078,8.15931373120115));
#54847=CARTESIAN_POINT('Ctrl Pts',(96.446025,-9.32159971279966,8.19928267103827));
#54848=CARTESIAN_POINT('Ctrl Pts',(96.446025,-9.28914203146188,8.23906337680869));
#54849=CARTESIAN_POINT('Ctrl Pts',(96.446025,-9.25642746403099,8.27865373987974));
#54850=CARTESIAN_POINT('Ctrl Pts',(96.446025,-9.2389484729194,8.29980638405533));
#54851=CARTESIAN_POINT('Ctrl Pts',(96.446025,-9.22139800546104,8.32090241663264));
#54852=CARTESIAN_POINT('Ctrl Pts',(96.446025,-9.20378185908125,8.34193511893918));
#54853=CARTESIAN_POINT('Ctrl Pts',(96.446025,-9.017527891134,8.56431203252688));
#54854=CARTESIAN_POINT('Ctrl Pts',(96.446025,-8.82376074067442,8.77982359138969));
#54855=CARTESIAN_POINT('Ctrl Pts',(96.446025,-8.62297236676072,8.98819473876588));
#54856=CARTESIAN_POINT('Ctrl Pts',(96.446025,-8.41981989343368,9.19901926577589));
#54857=CARTESIAN_POINT('Ctrl Pts',(96.446025,-8.20947954225884,9.40253470020656));
#54858=CARTESIAN_POINT('Ctrl Pts',(96.446025,-7.99241348006684,9.59843173573151));
#54859=CARTESIAN_POINT('Ctrl Pts',(96.446025,-7.77381751752192,9.7957094704812));
#54860=CARTESIAN_POINT('Ctrl Pts',(96.446025,-7.54840030538829,9.985261502155));
#54861=CARTESIAN_POINT('Ctrl Pts',(96.446025,-7.31659176195654,10.1667404004619));
#54862=CARTESIAN_POINT('Ctrl Pts',(96.446025,-7.0853784788602,10.3477532797503));
#54863=CARTESIAN_POINT('Ctrl Pts',(96.446025,-6.84780618879341,10.5207348556717));
#54864=CARTESIAN_POINT('Ctrl Pts',(96.446025,-6.60426630301782,10.6853025304088));
#54865=CARTESIAN_POINT('Ctrl Pts',(96.446025,-6.36375524498132,10.8478235295608));
#54866=CARTESIAN_POINT('Ctrl Pts',(96.446025,-6.11742362339088,11.0021389485234));
#54867=CARTESIAN_POINT('Ctrl Pts',(96.446025,-5.86562108206444,11.1478377897083));
#54868=CARTESIAN_POINT('Ctrl Pts',(96.446025,-5.74412924799045,11.218135807134));
#54869=CARTESIAN_POINT('Ctrl Pts',(96.446025,-5.62136344491582,11.2864272585636));
#54870=CARTESIAN_POINT('Ctrl Pts',(96.446025,-5.49736112202026,11.352662011339));
#54871=CARTESIAN_POINT('Ctrl Pts',(96.446025,-7.10371691227614,-9.16818944635619));
#54872=CARTESIAN_POINT('Ctrl Pts',(96.4870778022389,-5.79962471393883,-10.1767945155287));
#54873=CARTESIAN_POINT('Ctrl Pts',(96.5754470231585,-2.52487563733554,-11.7464480653471));
#54874=CARTESIAN_POINT('Ctrl Pts',(96.7111326627592,3.091848831559,-11.6726995174351));
#54875=CARTESIAN_POINT('Ctrl Pts',(96.8530819188018,8.23560924484923,-8.83096106044612));
#54876=CARTESIAN_POINT('Ctrl Pts',(96.9950311748445,11.4288580805009,-3.8977427059358));
#54877=CARTESIAN_POINT('Ctrl Pts',(97.136980430887,11.915327242442,1.95861959274003));
#54878=CARTESIAN_POINT('Ctrl Pts',(97.2789296869297,9.5797960279637,7.35110139990983));
#54879=CARTESIAN_POINT('Ctrl Pts',(97.4208789429723,4.97540930776886,11.0025682116464));
#54880=CARTESIAN_POINT('Ctrl Pts',(97.562828199015,-0.807342216722395,12.0482111751727));
#54881=CARTESIAN_POINT('Ctrl Pts',(97.7047774550576,-6.39888446344168,10.2403845654334));
#54882=CARTESIAN_POINT('Ctrl Pts',(97.8467267111003,-10.474929971616,6.00724889591607));
#54883=CARTESIAN_POINT('Ctrl Pts',(97.9441606947658,-11.569866836913,2.12505344398514));
#54884=CARTESIAN_POINT('Ctrl Pts',(97.9942782597504,-11.5985505397983,0.112590341614262));
#54885=CARTESIAN_POINT('Ctrl Pts',(97.9970794060541,-11.5984942842416,0.000109136483176196));
#54886=CARTESIAN_POINT('',(108.068877059804,-1.6708941109609,-12.5));
#54887=CARTESIAN_POINT('Ctrl Pts',(108.068877059804,-1.67089411096091,-12.5));
#54888=CARTESIAN_POINT('Ctrl Pts',(108.030091668611,-1.63767437386533,-12.4356882468672));
#54889=CARTESIAN_POINT('Ctrl Pts',(107.991648922957,-1.60240740323059,-12.3720777992513));
#54890=CARTESIAN_POINT('Ctrl Pts',(107.763118153063,-1.3766207604813,-11.9946044607362));
#54891=CARTESIAN_POINT('Ctrl Pts',(107.609518024559,-1.15600440609235,-11.743732333501));
#54892=CARTESIAN_POINT('Ctrl Pts',(107.499276121999,-0.914933857717767,
-11.5614942635284));
#54893=CARTESIAN_POINT('',(108.069877902573,-1.6893531453193,-12.5));
#54894=CARTESIAN_POINT('Ctrl Pts',(108.069877902573,-1.6893024527008,-12.4997161179536));
#54895=CARTESIAN_POINT('Ctrl Pts',(108.069541715314,-1.68315033687534,-12.4997204364986));
#54896=CARTESIAN_POINT('Ctrl Pts',(108.069208100619,-1.67699808055201,-12.4997247234326));
#54897=CARTESIAN_POINT('Ctrl Pts',(108.068877059804,-1.67084567891917,-12.499728977557));
#54898=CARTESIAN_POINT('',(106.333170942243,1.68935314531927,-12.5));
#54899=CARTESIAN_POINT('Ctrl Pts',(106.333170942243,1.68950627976338,-12.4993304720331));
#54900=CARTESIAN_POINT('Ctrl Pts',(106.349604935823,2.40108951933161,-12.4036781514243));
#54901=CARTESIAN_POINT('Ctrl Pts',(106.366038929404,3.104440874311,-12.2477515181746));
#54902=CARTESIAN_POINT('Ctrl Pts',(106.382472922984,3.78900867488091,-12.0321767960591));
#54903=CARTESIAN_POINT('Ctrl Pts',(106.429789341665,5.76000230515714,-11.4114984588888));
#54904=CARTESIAN_POINT('Ctrl Pts',(106.477105760346,7.57528637337726,-10.2963568485656));
#54905=CARTESIAN_POINT('Ctrl Pts',(106.524422179027,9.01989681297181,-8.81880545665698));
#54906=CARTESIAN_POINT('Ctrl Pts',(106.571738597708,10.4645072525664,-7.34125406474839));
#54907=CARTESIAN_POINT('Ctrl Pts',(106.619055016389,11.5384440635353,-5.50129289125441));
#54908=CARTESIAN_POINT('Ctrl Pts',(106.66637143507,12.1145334177084,-3.51680856345888));
#54909=CARTESIAN_POINT('Ctrl Pts',(106.713687853751,12.6906227718815,-1.53232423566335));
#54910=CARTESIAN_POINT('Ctrl Pts',(106.761004272431,12.7688646692587,0.596683246433734));
#54911=CARTESIAN_POINT('Ctrl Pts',(106.808320691112,12.3399927237232,2.61810049834914));
#54912=CARTESIAN_POINT('Ctrl Pts',(106.855637109793,11.9111207781878,4.63951775026454));
#54913=CARTESIAN_POINT('Ctrl Pts',(106.902953528474,10.9751349897396,6.55334477199826));
#54914=CARTESIAN_POINT('Ctrl Pts',(106.950269947155,9.64287593474204,8.13294591383067));
#54915=CARTESIAN_POINT('Ctrl Pts',(106.997586365836,8.31061687974451,9.71254705566307));
#54916=CARTESIAN_POINT('Ctrl Pts',(107.044902784517,6.58208455819763,10.9579223175942));
#54917=CARTESIAN_POINT('Ctrl Pts',(107.092219203198,4.66196510010847,11.7216009985322));
#54918=CARTESIAN_POINT('Ctrl Pts',(107.139535621879,2.7418456420193,12.4852796794702));
#54919=CARTESIAN_POINT('Ctrl Pts',(107.186852040559,0.630139047387844,12.7672617794151));
#54920=CARTESIAN_POINT('Ctrl Pts',(107.23416845924,-1.4230791740621,12.5341445146072));
#54921=CARTESIAN_POINT('Ctrl Pts',(107.281484877921,-3.47629739551205,12.3010272497992));
#54922=CARTESIAN_POINT('Ctrl Pts',(107.328801296602,-5.47102724378048,11.5528106202384));
#54923=CARTESIAN_POINT('Ctrl Pts',(107.376117715283,-7.17107529997091,10.3781200474853));
#54924=CARTESIAN_POINT('Ctrl Pts',(107.423434133964,-8.87112335616133,9.2034294747322));
#54925=CARTESIAN_POINT('Ctrl Pts',(107.470750552645,-10.2764896202737,7.60226495878686));
#54926=CARTESIAN_POINT('Ctrl Pts',(107.518066971325,-11.220710275081,5.76418777515091));
#54927=CARTESIAN_POINT('Ctrl Pts',(107.565383390006,-12.1649309298882,3.92611059151499));
#54928=CARTESIAN_POINT('Ctrl Pts',(107.612699808687,-12.6480059753902,1.85112074018848));
#54929=CARTESIAN_POINT('Ctrl Pts',(107.660016227368,-12.6128177077471,-0.214965601709239));
#54930=CARTESIAN_POINT('Ctrl Pts',(107.707332646049,-12.5776294401039,-2.28105194360693));
#54931=CARTESIAN_POINT('Ctrl Pts',(107.75464906473,-12.0241778593156,-4.33823477607583));
#54932=CARTESIAN_POINT('Ctrl Pts',(107.801965483411,-11.0178189077648,-6.14310386279632));
#54933=CARTESIAN_POINT('Ctrl Pts',(107.849281902092,-10.0114599562139,-7.94797294951689));
#54934=CARTESIAN_POINT('Ctrl Pts',(107.896598320773,-8.55219363390049,-9.50052829048904));
#54935=CARTESIAN_POINT('Ctrl Pts',(107.943914739453,-6.81322296014332,-10.6163520732922));
#54936=CARTESIAN_POINT('Ctrl Pts',(107.985902460493,-5.27009231793075,-11.6065136076629));
#54937=CARTESIAN_POINT('Ctrl Pts',(108.027890181533,-3.50670955580399,-12.2527725498014));
#54938=CARTESIAN_POINT('Ctrl Pts',(108.069877902573,-1.68930245270044,-12.4997161179536));
#54939=CARTESIAN_POINT('',(106.255592188287,-1.6893531453193,-12.5));
#54940=CARTESIAN_POINT('Ctrl Pts',(106.255592188287,-1.68964924171336,-12.5007055298766));
#54941=CARTESIAN_POINT('Ctrl Pts',(106.255090283124,-1.68046412560261,-12.5006983493389));
#54942=CARTESIAN_POINT('Ctrl Pts',(106.254594111819,-1.67127868122275,-12.5006910846807));
#54943=CARTESIAN_POINT('Ctrl Pts',(106.25410367875,-1.66209289375809,-12.5006837399));
#54944=CARTESIAN_POINT('Ctrl Pts',(106.24084152639,-1.41369342681394,-12.5004851244185));
#54945=CARTESIAN_POINT('Ctrl Pts',(106.231793456185,-1.16537581297815,-12.5002301926239));
#54946=CARTESIAN_POINT('Ctrl Pts',(106.22701103717,-0.916837633820512,-12.4999869955818));
#54947=CARTESIAN_POINT('Ctrl Pts',(106.224927426093,-0.80855416859948,-12.4998810391508));
#54948=CARTESIAN_POINT('Ctrl Pts',(106.223653513649,-0.700228172921927,
-12.4997771026051));
#54949=CARTESIAN_POINT('Ctrl Pts',(106.223193564612,-0.591831854740231,
-12.4996795564133));
#54950=CARTESIAN_POINT('Ctrl Pts',(106.222440583606,-0.414376610795987,
-12.4995198638745));
#54951=CARTESIAN_POINT('Ctrl Pts',(106.22387013875,-0.236993616228443,-12.4993777643298));
#54952=CARTESIAN_POINT('Ctrl Pts',(106.227481746357,-0.0595633864188738,
-12.4992668820702));
#54953=CARTESIAN_POINT('Ctrl Pts',(106.227751045141,-0.04633333754566,-12.4992586141571));
#54954=CARTESIAN_POINT('Ctrl Pts',(106.22803246533,-0.033103547113014,-12.4992505170535));
#54955=CARTESIAN_POINT('Ctrl Pts',(106.228326003854,-0.0198739657211027,
-12.4992425948726));
#54956=CARTESIAN_POINT('Ctrl Pts',(106.2284066559,-0.016239032903646,-12.4992404181903));
#54957=CARTESIAN_POINT('Ctrl Pts',(106.228488222706,-0.0126041193345105,
-12.4992382547142));
#54958=CARTESIAN_POINT('Ctrl Pts',(106.228570704203,-0.00896922399477974,
-12.4992361045266));
#54959=CARTESIAN_POINT('Ctrl Pts',(106.228619157464,-0.00683392653775541,
-12.4992348414118));
#54960=CARTESIAN_POINT('Ctrl Pts',(106.228667926366,-0.0046986357788803,
-12.499233582883));
#54961=CARTESIAN_POINT('Ctrl Pts',(106.228717010897,-0.00256335143549926,
-12.4992323289566));
#54962=CARTESIAN_POINT('Ctrl Pts',(106.228759389134,-0.000719805535707577,
-12.499231246351));
#54963=CARTESIAN_POINT('Ctrl Pts',(106.228802002639,0.0011237353156715,
-12.4992301671762));
#54964=CARTESIAN_POINT('Ctrl Pts',(106.228844851403,0.00296727129289191,
-12.4992290914429));
#54965=CARTESIAN_POINT('Ctrl Pts',(106.228897035082,0.00521243500223122,
-12.4992277813532));
#54966=CARTESIAN_POINT('Ctrl Pts',(106.228949567684,0.00745759110152448,
-12.499226476368));
#54967=CARTESIAN_POINT('Ctrl Pts',(106.22900244919,0.00970273982115463,
-12.499225176506));
#54968=CARTESIAN_POINT('Ctrl Pts',(106.229102217696,0.0139385332193429,
-12.499222724131));
#54969=CARTESIAN_POINT('Ctrl Pts',(106.229203228059,0.0181742985818641,
-12.4992202899931));
#54970=CARTESIAN_POINT('Ctrl Pts',(106.229305480159,0.0224100375279641,
-12.4992178742175));
#54971=CARTESIAN_POINT('Ctrl Pts',(106.229887912142,0.0465369730381842,
-12.4992041138644));
#54972=CARTESIAN_POINT('Ctrl Pts',(106.230510625946,0.0706627953287636,
-12.4991909496053));
#54973=CARTESIAN_POINT('Ctrl Pts',(106.231173596977,0.0947878029303355,
-12.4991784031374));
#54974=CARTESIAN_POINT('Ctrl Pts',(106.232021250125,0.1256332511997,-12.4991623616326));
#54975=CARTESIAN_POINT('Ctrl Pts',(106.232934690913,0.15647655828141,-12.499147330676));
#54976=CARTESIAN_POINT('Ctrl Pts',(106.233913857501,0.187318345679374,-12.4991333498929));
#54977=CARTESIAN_POINT('Ctrl Pts',(106.238735653156,0.339195256385656,-12.4990645030998));
#54978=CARTESIAN_POINT('Ctrl Pts',(106.245149236366,0.49097111824434,-12.4990214443691));
#54979=CARTESIAN_POINT('Ctrl Pts',(106.253143110002,0.642718595914829,-12.4990066325146));
#54980=CARTESIAN_POINT('Ctrl Pts',(106.265792998464,0.882851071655931,-12.4989831935268));
#54981=CARTESIAN_POINT('Ctrl Pts',(106.282378544058,1.12249522883079,-12.4990322697312));
#54982=CARTESIAN_POINT('Ctrl Pts',(106.302811012959,1.36192005952878,-12.4991430117722));
#54983=CARTESIAN_POINT('Ctrl Pts',(106.312133054,1.471154440791,-12.4991935363494));
#54984=CARTESIAN_POINT('Ctrl Pts',(106.322255839342,1.58034251740705,-12.4992566534061));
#54985=CARTESIAN_POINT('Ctrl Pts',(106.333170942243,1.68950627976311,-12.4993304720331));
#54986=CARTESIAN_POINT('',(104.518885227957,1.68935314531927,-12.5));
#54987=CARTESIAN_POINT('Ctrl Pts',(104.518885227957,1.68966509259281,-12.5005876262282));
#54988=CARTESIAN_POINT('Ctrl Pts',(104.524967683448,1.95296088446919,-12.4652318044223));
#54989=CARTESIAN_POINT('Ctrl Pts',(104.531050138939,2.2151108340558,-12.4215019868369));
#54990=CARTESIAN_POINT('Ctrl Pts',(104.53713259443,2.47557965491845,-12.369372315482));
#54991=CARTESIAN_POINT('Ctrl Pts',(104.584449013111,4.50180932473757,-11.9638470536585));
#54992=CARTESIAN_POINT('Ctrl Pts',(104.631765431792,6.42630483037507,-11.0500013459916));
#54993=CARTESIAN_POINT('Ctrl Pts',(104.679081850473,8.02116966160399,-9.73605173396329));
#54994=CARTESIAN_POINT('Ctrl Pts',(104.726398269154,9.61603449283293,-8.42210212193495));
#54995=CARTESIAN_POINT('Ctrl Pts',(104.773714687835,10.8812686496533,-6.70804860554518));
#54996=CARTESIAN_POINT('Ctrl Pts',(104.821031106515,11.667044580788,-4.79686740039649));
#54997=CARTESIAN_POINT('Ctrl Pts',(104.868347525196,12.4528205119227,-2.8856861952478));
#54998=CARTESIAN_POINT('Ctrl Pts',(104.915663943877,12.7591382173717,-0.777377301340174));
#54999=CARTESIAN_POINT('Ctrl Pts',(104.962980362558,12.5497239122681,1.27839580422383));
#55000=CARTESIAN_POINT('Ctrl Pts',(105.010296781239,12.3403096071644,3.3341689097878));
#55001=CARTESIAN_POINT('Ctrl Pts',(105.05761319992,11.6151632915081,5.33740622700816));
#55002=CARTESIAN_POINT('Ctrl Pts',(105.104929618601,10.4601559449718,7.05088673245123));
#55003=CARTESIAN_POINT('Ctrl Pts',(105.152246037282,9.30514859843542,8.76436723789434));
#55004=CARTESIAN_POINT('Ctrl Pts',(105.199562455963,7.72028022101907,10.1880909315601));
#55005=CARTESIAN_POINT('Ctrl Pts',(105.246878874643,5.8932290754146,11.1534621159742));
#55006=CARTESIAN_POINT('Ctrl Pts',(105.294195293324,4.06617792981017,12.1188333003882));
#55007=CARTESIAN_POINT('Ctrl Pts',(105.341511712005,1.99694401601767,12.6258519755504));
#55008=CARTESIAN_POINT('Ctrl Pts',(105.388828130686,-0.0694364031569377,
12.6144775828521));
#55009=CARTESIAN_POINT('Ctrl Pts',(105.436144549367,-2.1358168223316,12.6031031901538));
#55010=CARTESIAN_POINT('Ctrl Pts',(105.483460968048,-4.19934374688837,12.0733357295948));
#55011=CARTESIAN_POINT('Ctrl Pts',(105.530777386729,-6.01565672686706,11.0879096435399));
#55012=CARTESIAN_POINT('Ctrl Pts',(105.57809380541,-7.8319697068457,10.1024835574851));
#55013=CARTESIAN_POINT('Ctrl Pts',(105.62541022409,-9.40106874224627,8.66139884593429));
#55014=CARTESIAN_POINT('Ctrl Pts',(105.672726642771,-10.5371429608089,6.93530708083006));
#55015=CARTESIAN_POINT('Ctrl Pts',(105.720043061452,-11.6732171793715,5.20921531572579));
#55016=CARTESIAN_POINT('Ctrl Pts',(105.767359480133,-12.3762665810961,3.19811649706804));
#55017=CARTESIAN_POINT('Ctrl Pts',(105.814675898814,-12.5630368705784,1.14016259125187));
#55018=CARTESIAN_POINT('Ctrl Pts',(105.861992317495,-12.7498071600607,-0.917791314564243));
#55019=CARTESIAN_POINT('Ctrl Pts',(105.909308736176,-12.4202983373007,-3.02260030753877));
#55020=CARTESIAN_POINT('Ctrl Pts',(105.956625154857,-11.6135304654158,-4.92501535018149));
#55021=CARTESIAN_POINT('Ctrl Pts',(106.003941573537,-10.8067625935309,-6.82743039282427));
#55022=CARTESIAN_POINT('Ctrl Pts',(106.051257992218,-9.52273567252103,-8.52745148513522));
#55023=CARTESIAN_POINT('Ctrl Pts',(106.098574410899,-7.91350264344085,-9.82376414526043));
#55024=CARTESIAN_POINT('Ctrl Pts',(106.14589082958,-6.30426961436072,-11.1200768053856));
#55025=CARTESIAN_POINT('Ctrl Pts',(106.193207248261,-4.36983047721028,-12.0126810333251));
#55026=CARTESIAN_POINT('Ctrl Pts',(106.240523666942,-2.33925931246893,-12.395875615286));
#55027=CARTESIAN_POINT('Ctrl Pts',(106.24554650739,-2.12370548857135,-12.4365533609729));
#55028=CARTESIAN_POINT('Ctrl Pts',(106.250569347839,-1.90706837865939,-12.4714907060993));
#55029=CARTESIAN_POINT('Ctrl Pts',(106.255592188287,-1.68964924171407,-12.5007055298765));
#55030=CARTESIAN_POINT('',(104.441306474002,-1.6893531453193,-12.5));
#55031=CARTESIAN_POINT('Ctrl Pts',(104.441306474002,-1.689543392924,-12.4994338659969));
#55032=CARTESIAN_POINT('Ctrl Pts',(104.440804568837,-1.68035562471557,-12.4994269115715));
#55033=CARTESIAN_POINT('Ctrl Pts',(104.440308397532,-1.67116754787944,-12.4994200217841));
#55034=CARTESIAN_POINT('Ctrl Pts',(104.439817964464,-1.66197914759247,-12.499413198474));
#55035=CARTESIAN_POINT('Ctrl Pts',(104.426601193732,-1.41435926262478,-12.4992293158366));
#55036=CARTESIAN_POINT('Ctrl Pts',(104.417569714248,-1.1668349916106,-12.4990961157117));
#55037=CARTESIAN_POINT('Ctrl Pts',(104.412774567463,-0.919107466037736,
-12.4990367636774));
#55038=CARTESIAN_POINT('Ctrl Pts',(104.410661772918,-0.809955986798895,
-12.4990106125166));
#55039=CARTESIAN_POINT('Ctrl Pts',(104.409371411855,-0.700764382308139,
-12.4989985641351));
#55040=CARTESIAN_POINT('Ctrl Pts',(104.408907850326,-0.591504241844385,
-12.4990011977212));
#55041=CARTESIAN_POINT('Ctrl Pts',(104.40815486932,-0.414028749507104,-12.4990054755574));
#55042=CARTESIAN_POINT('Ctrl Pts',(104.409584424463,-0.236633170009759,
-12.4990487087553));
#55043=CARTESIAN_POINT('Ctrl Pts',(104.413196032071,-0.059198115721675,
-12.4991274190233));
#55044=CARTESIAN_POINT('Ctrl Pts',(104.413465330855,-0.0459677071079966,
-12.4991332880383));
#55045=CARTESIAN_POINT('Ctrl Pts',(104.413746751044,-0.0327376001033777,
-12.4991393509431));
#55046=CARTESIAN_POINT('Ctrl Pts',(104.414040289568,-0.0195077453537486,
-12.4991456047362));
#55047=CARTESIAN_POINT('Ctrl Pts',(104.414120941615,-0.015872737397679,
-12.4991473230157));
#55048=CARTESIAN_POINT('Ctrl Pts',(104.414202508422,-0.0122377519513052,
-12.4991490557029));
#55049=CARTESIAN_POINT('Ctrl Pts',(104.414284989917,-0.00860278808548892,
-12.4991508027325));
#55050=CARTESIAN_POINT('Ctrl Pts',(104.414333443178,-0.00646745033113518,
-12.4991518290146));
#55051=CARTESIAN_POINT('Ctrl Pts',(104.41438221208,-0.0043321204006724,
-12.499152860246));
#55052=CARTESIAN_POINT('Ctrl Pts',(104.414431296611,-0.00219679803272295,
-12.4991538964133));
#55053=CARTESIAN_POINT('Ctrl Pts',(104.414473674849,-0.000353219273919923,
-12.4991547910117));
#55054=CARTESIAN_POINT('Ctrl Pts',(104.414516288354,0.00149035359713489,
-12.4991556892893));
#55055=CARTESIAN_POINT('Ctrl Pts',(104.414559137117,0.00333392070166297,
-12.4991565912373));
#55056=CARTESIAN_POINT('Ctrl Pts',(104.414611320797,0.00557912236092147,
-12.4991576896812));
#55057=CARTESIAN_POINT('Ctrl Pts',(104.414663853398,0.00782431516533509,
-12.499158793569));
#55058=CARTESIAN_POINT('Ctrl Pts',(104.414716734904,0.0100694993497503,
-12.4991599028846));
#55059=CARTESIAN_POINT('Ctrl Pts',(104.41481650341,0.0143053596477874,-12.4991619957667));
#55060=CARTESIAN_POINT('Ctrl Pts',(104.414917513773,0.0185411874785826,
-12.4991641079682));
#55061=CARTESIAN_POINT('Ctrl Pts',(104.415019765873,0.0227769844685048,
-12.4991662393806));
#55062=CARTESIAN_POINT('Ctrl Pts',(104.415602197855,0.0469042505477953,
-12.4991783799892));
#55063=CARTESIAN_POINT('Ctrl Pts',(104.416224911658,0.0710302595856344,
-12.4991911439495));
#55064=CARTESIAN_POINT('Ctrl Pts',(104.416887882689,0.0951553099302959,
-12.4992045098246));
#55065=CARTESIAN_POINT('Ctrl Pts',(104.417735535892,0.126000814885945,-12.4992215989979));
#55066=CARTESIAN_POINT('Ctrl Pts',(104.418648976744,0.15684394323554,-12.4992396718907));
#55067=CARTESIAN_POINT('Ctrl Pts',(104.419628143405,0.187685316122949,-12.49925867807));
#55068=CARTESIAN_POINT('Ctrl Pts',(104.42444993935,0.339560183550717,-12.4993522718595));
#55069=CARTESIAN_POINT('Ctrl Pts',(104.430863523015,0.491328285835151,-12.4994687385499));
#55070=CARTESIAN_POINT('Ctrl Pts',(104.438857397269,0.643062254578234,-12.4995998677619));
#55071=CARTESIAN_POINT('Ctrl Pts',(104.451539138457,0.883777940103603,-12.4998078953935));
#55072=CARTESIAN_POINT('Ctrl Pts',(104.468176381684,1.12398843422842,-12.5000540750527));
#55073=CARTESIAN_POINT('Ctrl Pts',(104.488679721142,1.36396469732121,-12.500286550178));
#55074=CARTESIAN_POINT('Ctrl Pts',(104.497959102239,1.47257291717617,-12.5003917635403));
#55075=CARTESIAN_POINT('Ctrl Pts',(104.508030367173,1.58113250880452,-12.5004939559224));
#55076=CARTESIAN_POINT('Ctrl Pts',(104.518885227957,1.6896650925929,-12.5005876262282));
#55077=CARTESIAN_POINT('',(102.704599513671,1.68935314531927,-12.5));
#55078=CARTESIAN_POINT('Ctrl Pts',(102.704599513671,1.68928977174207,-12.5008279278805));
#55079=CARTESIAN_POINT('Ctrl Pts',(102.747646849754,3.55224433648731,-12.2477504944552));
#55080=CARTESIAN_POINT('Ctrl Pts',(102.790694185836,5.35885448828508,-11.5735404103196));
#55081=CARTESIAN_POINT('Ctrl Pts',(102.833741521919,6.92975537674916,-10.540794871603));
#55082=CARTESIAN_POINT('Ctrl Pts',(102.881057940599,8.65644536291872,-9.40563007982129));
#55083=CARTESIAN_POINT('Ctrl Pts',(102.92837435928,10.0983564409266,-7.83729039347354));
#55084=CARTESIAN_POINT('Ctrl Pts',(102.975690777961,11.084739184859,-6.02149676662285));
#55085=CARTESIAN_POINT('Ctrl Pts',(103.023007196642,12.0711219287913,-4.20570313977216));
#55086=CARTESIAN_POINT('Ctrl Pts',(103.070323615323,12.6019763386482,-2.14245557241852));
#55087=CARTESIAN_POINT('Ctrl Pts',(103.117640034004,12.6144392551756,-0.0760814319127967));
#55088=CARTESIAN_POINT('Ctrl Pts',(103.164956452685,12.626902171703,1.99029270859294));
#55089=CARTESIAN_POINT('Ctrl Pts',(103.212272871366,12.1209735949009,4.05979342225078));
#55090=CARTESIAN_POINT('Ctrl Pts',(103.259589290047,11.1565649959828,5.88735285142727));
#55091=CARTESIAN_POINT('Ctrl Pts',(103.306905708727,10.1921563970646,7.71491228060374));
#55092=CARTESIAN_POINT('Ctrl Pts',(103.354222127408,8.76926777603044,9.30053042529888));
#55093=CARTESIAN_POINT('Ctrl Pts',(103.401538546089,7.05639594165463,10.4564402365909));
#55094=CARTESIAN_POINT('Ctrl Pts',(103.44885496477,5.34352410727879,11.6123500478829));
#55095=CARTESIAN_POINT('Ctrl Pts',(103.496171383451,3.34066905956132,12.3385515257718));
#55096=CARTESIAN_POINT('Ctrl Pts',(103.543487802132,1.28500655420755,12.5490487393444));
#55097=CARTESIAN_POINT('Ctrl Pts',(103.590804220813,-0.770655951146216,
12.7595459529169));
#55098=CARTESIAN_POINT('Ctrl Pts',(103.638120639494,-2.87912591413628,12.4543389021731));
#55099=CARTESIAN_POINT('Ctrl Pts',(103.685437058174,-4.79072078413387,11.6695698496244));
#55100=CARTESIAN_POINT('Ctrl Pts',(103.732753476855,-6.70231565413145,10.8848007970757));
#55101=CARTESIAN_POINT('Ctrl Pts',(103.780069895536,-8.41703543113655,9.62046974272214));
#55102=CARTESIAN_POINT('Ctrl Pts',(103.827386314217,-9.73182500170104,8.02629729346387));
#55103=CARTESIAN_POINT('Ctrl Pts',(103.874702732898,-11.0466145722655,6.43212484420561));
#55104=CARTESIAN_POINT('Ctrl Pts',(103.922019151579,-11.9614739363894,4.50811100004268));
#55105=CARTESIAN_POINT('Ctrl Pts',(103.96933557026,-12.3680665165972,2.48209523343109));
#55106=CARTESIAN_POINT('Ctrl Pts',(104.016651988941,-12.774659096805,0.456079466819497));
#55107=CARTESIAN_POINT('Ctrl Pts',(104.063968407621,-12.6729848930967,-1.67193822224076));
#55108=CARTESIAN_POINT('Ctrl Pts',(104.111284826302,-12.0750840459337,-3.64996046422953));
#55109=CARTESIAN_POINT('Ctrl Pts',(104.158601244983,-11.4771831987707,-5.62798270621831));
#55110=CARTESIAN_POINT('Ctrl Pts',(104.205917663664,-10.383055708153,-7.4560095011356));
#55111=CARTESIAN_POINT('Ctrl Pts',(104.253234082345,-8.92226687373862,-8.91756805079638));
#55112=CARTESIAN_POINT('Ctrl Pts',(104.300550501026,-7.46147803932427,-10.3791266004572));
#55113=CARTESIAN_POINT('Ctrl Pts',(104.347866919707,-5.63402786111328,-11.4742169048614));
#55114=CARTESIAN_POINT('Ctrl Pts',(104.395183338388,-3.65632085500738,-12.0731596490735));
#55115=CARTESIAN_POINT('Ctrl Pts',(104.410557716926,-3.01371059419662,-12.2677722746447));
#55116=CARTESIAN_POINT('Ctrl Pts',(104.425932095464,-2.35523659191329,-12.4100028771332));
#55117=CARTESIAN_POINT('Ctrl Pts',(104.441306474002,-1.68954339292365,-12.499433865997));
#55118=CARTESIAN_POINT('',(102.627020759716,-1.68935314531929,-12.5));
#55119=CARTESIAN_POINT('Ctrl Pts',(102.627020759716,-1.68914447211972,-12.499042498534));
#55120=CARTESIAN_POINT('Ctrl Pts',(102.626518854552,-1.67995707528232,-12.4990448625818));
#55121=CARTESIAN_POINT('Ctrl Pts',(102.626022683247,-1.67076939350443,-12.4990473235431));
#55122=CARTESIAN_POINT('Ctrl Pts',(102.625532250178,-1.66158141178441,-12.4990498810209));
#55123=CARTESIAN_POINT('Ctrl Pts',(102.612383688404,-1.4152506627532,-12.4991184472672));
#55124=CARTESIAN_POINT('Ctrl Pts',(102.603377330541,-1.1690313997046,-12.4992586077918));
#55125=CARTESIAN_POINT('Ctrl Pts',(102.598563431873,-0.92262521463345,-12.4994487371169));
#55126=CARTESIAN_POINT('Ctrl Pts',(102.596406399541,-0.812214475966295,
-12.4995339310792));
#55127=CARTESIAN_POINT('Ctrl Pts',(102.595091127173,-0.701765534330746,
-12.4996288943628));
#55128=CARTESIAN_POINT('Ctrl Pts',(102.594622136041,-0.591248584118155,
-12.499730091944));
#55129=CARTESIAN_POINT('Ctrl Pts',(102.593869155034,-0.41380991033001,-12.4998925680579));
#55130=CARTESIAN_POINT('Ctrl Pts',(102.595298710177,-0.236456608632446,
-12.500071092898));
#55131=CARTESIAN_POINT('Ctrl Pts',(102.598910317785,-0.059067595309641,
-12.5002449761604));
#55132=CARTESIAN_POINT('Ctrl Pts',(102.599179616569,-0.0458406197222311,
-12.5002579417304));
#55133=CARTESIAN_POINT('Ctrl Pts',(102.599461036759,-0.0326139665295593,
-12.5002708777699));
#55134=CARTESIAN_POINT('Ctrl Pts',(102.599754575282,-0.0193875856951232,
-12.5002837741577));
#55135=CARTESIAN_POINT('Ctrl Pts',(102.599835227328,-0.0157535322845329,
-12.5002873175429));
#55136=CARTESIAN_POINT('Ctrl Pts',(102.599916794133,-0.0121195028984813,
-12.5002908579301));
#55137=CARTESIAN_POINT('Ctrl Pts',(102.599999275632,-0.00848549640073772,
-12.5002943951067));
#55138=CARTESIAN_POINT('Ctrl Pts',(102.600047728893,-0.00635072106825237,
-12.5002964729999));
#55139=CARTESIAN_POINT('Ctrl Pts',(102.600096497797,-0.00421595407720239,
-12.5002985497847));
#55140=CARTESIAN_POINT('Ctrl Pts',(102.600145582325,-0.00208119532421411,
-12.5003006254177));
#55141=CARTESIAN_POINT('Ctrl Pts',(102.600187960563,-0.000238103086124358,
-12.5003024174623));
#55142=CARTESIAN_POINT('Ctrl Pts',(102.600230574068,0.00160498288079793,
-12.5003042086483));
#55143=CARTESIAN_POINT('Ctrl Pts',(102.600273422832,0.00344806271039932,
-12.5003059989476));
#55144=CARTESIAN_POINT('Ctrl Pts',(102.60032560651,0.00569267088955102,
-12.5003081792766));
#55145=CARTESIAN_POINT('Ctrl Pts',(102.60037813911,0.00793726964793562,
-12.5003103582903));
#55146=CARTESIAN_POINT('Ctrl Pts',(102.600431020618,0.0101818593436699,
-12.500312535938));
#55147=CARTESIAN_POINT('Ctrl Pts',(102.600530789125,0.014416597910145,-12.500316644381));
#55148=CARTESIAN_POINT('Ctrl Pts',(102.600631799488,0.0186513020079477,
-12.5003207479601));
#55149=CARTESIAN_POINT('Ctrl Pts',(102.600734051588,0.0228859732661158,
-12.5003248463334));
#55150=CARTESIAN_POINT('Ctrl Pts',(102.60131648357,0.0470068272114195,-12.5003481908287));
#55151=CARTESIAN_POINT('Ctrl Pts',(102.601939197373,0.0711263600042235,
-12.5003713663617));
#55152=CARTESIAN_POINT('Ctrl Pts',(102.602602168403,0.0952448742825837,
-12.5003943084139));
#55153=CARTESIAN_POINT('Ctrl Pts',(102.60344982162,0.126082022963942,-12.5004236413763));
#55154=CARTESIAN_POINT('Ctrl Pts',(102.604363262488,0.156916697488337,-12.5004525920831));
#55155=CARTESIAN_POINT('Ctrl Pts',(102.605342429167,0.187749527997318,-12.500481020301));
#55156=CARTESIAN_POINT('Ctrl Pts',(102.610164225186,0.339582328914088,-12.5006210118578));
#55157=CARTESIAN_POINT('Ctrl Pts',(102.616577808967,0.491306236465511,-12.5007485459572));
#55158=CARTESIAN_POINT('Ctrl Pts',(102.624571683377,0.642994952392699,-12.5008448327383));
#55159=CARTESIAN_POINT('Ctrl Pts',(102.633100273966,0.804830238842706,-12.5009475602136));
#55160=CARTESIAN_POINT('Ctrl Pts',(102.643417815241,0.966434895985585,-12.5010150028948));
#55161=CARTESIAN_POINT('Ctrl Pts',(102.655497113968,1.12789502530787,-12.501019908215));
#55162=CARTESIAN_POINT('Ctrl Pts',(102.669508357471,1.31517884361736,-12.5010255980848));
#55163=CARTESIAN_POINT('Ctrl Pts',(102.685889970392,1.50226880459108,-12.5009473534237));
#55164=CARTESIAN_POINT('Ctrl Pts',(102.704599513671,1.68928977174265,-12.5008279278804));
#55165=CARTESIAN_POINT('',(100.890313799386,1.68935314531927,-12.5));
#55166=CARTESIAN_POINT('Ctrl Pts',(100.890313799386,1.68901725126337,-12.4995884691532));
#55167=CARTESIAN_POINT('Ctrl Pts',(100.923009597379,3.10436959511541,-12.3070954004652));
#55168=CARTESIAN_POINT('Ctrl Pts',(100.955705395371,4.48781279745029,-11.8755333660407));
#55169=CARTESIAN_POINT('Ctrl Pts',(100.988401193364,5.75826554513978,-11.2237357425437));
#55170=CARTESIAN_POINT('Ctrl Pts',(101.035717612045,7.59682822946574,-10.2804729643937));
#55171=CARTESIAN_POINT('Ctrl Pts',(101.083034030726,9.1987544835431,-8.87596977637554));
#55172=CARTESIAN_POINT('Ctrl Pts',(101.130350449407,10.3743460711825,-7.17654580575761));
#55173=CARTESIAN_POINT('Ctrl Pts',(101.177666868088,11.5499376588219,-5.47712183513971));
#55174=CARTESIAN_POINT('Ctrl Pts',(101.224983286769,12.2991945800233,-3.48277708192202));
#55175=CARTESIAN_POINT('Ctrl Pts',(101.27229970545,12.533390705202,-1.42967952267392));
#55176=CARTESIAN_POINT('Ctrl Pts',(101.31961612413,12.7675868303807,0.62341803657417));
#55177=CARTESIAN_POINT('Ctrl Pts',(101.366932542811,12.4867221595366,2.73526840185267));
#55178=CARTESIAN_POINT('Ctrl Pts',(101.414248961492,11.7240563589818,4.65578871924149));
#55179=CARTESIAN_POINT('Ctrl Pts',(101.461565380173,10.9613905584269,6.57630903663028));
#55180=CARTESIAN_POINT('Ctrl Pts',(101.508881798854,9.71692362816134,8.3054993061294));
#55181=CARTESIAN_POINT('Ctrl Pts',(101.556198217535,8.13802388870941,9.63859083546926));
#55182=CARTESIAN_POINT('Ctrl Pts',(101.603514636216,6.55912414925745,10.9716823648091));
#55183=CARTESIAN_POINT('Ctrl Pts',(101.650831054897,4.64579160061914,11.9086751539898));
#55184=CARTESIAN_POINT('Ctrl Pts',(101.698147473577,2.62460084870815,12.3386116111886));
#55185=CARTESIAN_POINT('Ctrl Pts',(101.745463892258,0.603410096797157,12.7685480683874));
#55186=CARTESIAN_POINT('Ctrl Pts',(101.792780310939,-1.52563885838652,12.6914281936044));
#55187=CARTESIAN_POINT('Ctrl Pts',(101.84009672962,-3.51042652599171,12.1163844323466));
#55188=CARTESIAN_POINT('Ctrl Pts',(101.887413148301,-5.4952141935969,11.5413406710888));
#55189=CARTESIAN_POINT('Ctrl Pts',(101.934729566982,-7.3357405736236,10.4683730233561));
#55190=CARTESIAN_POINT('Ctrl Pts',(101.982045985663,-8.81405268161804,9.02454106492175));
#55191=CARTESIAN_POINT('Ctrl Pts',(102.029362404344,-10.2923647896125,7.58070910648745));
#55192=CARTESIAN_POINT('Ctrl Pts',(102.076678823025,-11.4084626255746,5.76601283735156));
#55193=CARTESIAN_POINT('Ctrl Pts',(102.123995241705,-12.030179187211,3.79534647040199));
#55194=CARTESIAN_POINT('Ctrl Pts',(102.171311660386,-12.6518957488473,1.8246801034524));
#55195=CARTESIAN_POINT('Ctrl Pts',(102.218628079067,-12.7792310361579,-0.301956361310865));
#55196=CARTESIAN_POINT('Ctrl Pts',(102.265944497748,-12.3971061531285,-2.33272911733478));
#55197=CARTESIAN_POINT('Ctrl Pts',(102.313260916429,-12.0149812700991,-4.3635018733587));
#55198=CARTESIAN_POINT('Ctrl Pts',(102.36057733511,-11.1233962167298,-6.29841092064327));
#55199=CARTESIAN_POINT('Ctrl Pts',(102.407893753791,-9.82793145379795,-7.90832658950336));
#55200=CARTESIAN_POINT('Ctrl Pts',(102.455210172472,-8.53246669086617,-9.51824225836343));
#55201=CARTESIAN_POINT('Ctrl Pts',(102.502526591152,-6.8331222183719,-10.803164548799));
#55202=CARTESIAN_POINT('Ctrl Pts',(102.549843009833,-4.93113242415901,-11.6109344637805));
#55203=CARTESIAN_POINT('Ctrl Pts',(102.575568926461,-3.89702138540229,-12.0501186215501));
#55204=CARTESIAN_POINT('Ctrl Pts',(102.601294843088,-2.80300652002858,-12.3482521351367));
#55205=CARTESIAN_POINT('Ctrl Pts',(102.627020759716,-1.68914447211892,-12.4990424985341));
#55206=CARTESIAN_POINT('',(100.81273504543,-1.68935314531929,-12.5));
#55207=CARTESIAN_POINT('Ctrl Pts',(100.81273504543,-1.68904687944112,-12.5000065800334));
#55208=CARTESIAN_POINT('Ctrl Pts',(100.812233140265,-1.67986234589066,-12.5000153813875));
#55209=CARTESIAN_POINT('Ctrl Pts',(100.811736968961,-1.67067753085417,-12.500024197569));
#55210=CARTESIAN_POINT('Ctrl Pts',(100.811246535893,-1.6614924188256,-12.5000330258491));
#55211=CARTESIAN_POINT('Ctrl Pts',(100.798193427403,-1.41702631010753,-12.5002679947065));
#55212=CARTESIAN_POINT('Ctrl Pts',(100.789222599649,-1.17267204576433,-12.5005136843555));
#55213=CARTESIAN_POINT('Ctrl Pts',(100.784383221339,-0.928128757686291,
-12.5007042010178));
#55214=CARTESIAN_POINT('Ctrl Pts',(100.782163525937,-0.81596319065912,-12.5007915859942));
#55215=CARTESIAN_POINT('Ctrl Pts',(100.780813011206,-0.70375717139188,-12.5008670670383));
#55216=CARTESIAN_POINT('Ctrl Pts',(100.780336421755,-0.591478528683606,
-12.500922451509));
#55217=CARTESIAN_POINT('Ctrl Pts',(100.779810184042,-0.467503363071267,
-12.5009836056052));
#55218=CARTESIAN_POINT('Ctrl Pts',(100.780349946661,-0.343566876696398,
-12.5010201462746));
#55219=CARTESIAN_POINT('Ctrl Pts',(100.781955544507,-0.219626668121229,
-12.5010194195077));
#55220=CARTESIAN_POINT('Ctrl Pts',(100.782647358368,-0.166223784873483,
-12.5010191063612));
#55221=CARTESIAN_POINT('Ctrl Pts',(100.783537049102,-0.112820200000195,
-12.5010118523632));
#55222=CARTESIAN_POINT('Ctrl Pts',(100.784624603499,-0.0594125214676394,
-12.500998703149));
#55223=CARTESIAN_POINT('Ctrl Pts',(100.784893902284,-0.046187782611698,
-12.5009954471579));
#55224=CARTESIAN_POINT('Ctrl Pts',(100.785175322473,-0.0329633147788684,
-12.5009918295968));
#55225=CARTESIAN_POINT('Ctrl Pts',(100.785468860997,-0.0197390670073646,
-12.5009878659091));
#55226=CARTESIAN_POINT('Ctrl Pts',(100.785549513043,-0.0161055996369931,
-12.5009867768544));
#55227=CARTESIAN_POINT('Ctrl Pts',(100.785631079849,-0.0124721523439735,
-12.5009856616697));
#55228=CARTESIAN_POINT('Ctrl Pts',(100.785713561346,-0.0088387240911394,
-12.5009845206726));
#55229=CARTESIAN_POINT('Ctrl Pts',(100.785762014606,-0.00670428845895918,
-12.5009838504007));
#55230=CARTESIAN_POINT('Ctrl Pts',(100.785810783508,-0.00456985979954622,
-12.5009831712213));
#55231=CARTESIAN_POINT('Ctrl Pts',(100.78585986804,-0.00243543782588915,
-12.5009824831985));
#55232=CARTESIAN_POINT('Ctrl Pts',(100.785902246277,-0.000592636453217514,
-12.5009818891786));
#55233=CARTESIAN_POINT('Ctrl Pts',(100.785944859783,0.00125015967138045,
-12.5009812885668));
#55234=CARTESIAN_POINT('Ctrl Pts',(100.785987708546,0.00309295067176889,
-12.5009806814044));
#55235=CARTESIAN_POINT('Ctrl Pts',(100.786039892226,0.00533720716887695,
-12.5009799419672));
#55236=CARTESIAN_POINT('Ctrl Pts',(100.786092424827,0.00758145576628483,
-12.5009791928144));
#55237=CARTESIAN_POINT('Ctrl Pts',(100.786145306333,0.00982569664479346,
-12.5009784340204));
#55238=CARTESIAN_POINT('Ctrl Pts',(100.786245074838,0.0140597773254563,
-12.5009770024471));
#55239=CARTESIAN_POINT('Ctrl Pts',(100.786346085201,0.0182938289677911,
-12.5009755365572));
#55240=CARTESIAN_POINT('Ctrl Pts',(100.786448337302,0.0225278532933111,
-12.5009740368479));
#55241=CARTESIAN_POINT('Ctrl Pts',(100.787030769284,0.0466450220426878,
-12.5009654944453));
#55242=CARTESIAN_POINT('Ctrl Pts',(100.787653483087,0.0707610468272474,
-12.5009558550683));
#55243=CARTESIAN_POINT('Ctrl Pts',(100.788316454117,0.0948762357697601,
-12.5009452092726));
#55244=CARTESIAN_POINT('Ctrl Pts',(100.789164107338,0.125709132916537,-12.5009315979041));
#55245=CARTESIAN_POINT('Ctrl Pts',(100.79007754821,0.156539854627723,-12.5009163418817));
#55246=CARTESIAN_POINT('Ctrl Pts',(100.791056714894,0.187369042442589,-12.5008996248898));
#55247=CARTESIAN_POINT('Ctrl Pts',(100.795878510932,0.339183905208656,-12.5008173039462));
#55248=CARTESIAN_POINT('Ctrl Pts',(100.802292094743,0.490897403440178,-12.5006999080129));
#55249=CARTESIAN_POINT('Ctrl Pts',(100.810285969195,0.642584577087836,-12.5005670786308));
#55250=CARTESIAN_POINT('Ctrl Pts',(100.822840468179,0.880811544388206,-12.500358468106));
#55251=CARTESIAN_POINT('Ctrl Pts',(100.839271492313,1.11856274394623,-12.5001140814977));
#55252=CARTESIAN_POINT('Ctrl Pts',(100.859492300037,1.3561101677418,-12.4998886286552));
#55253=CARTESIAN_POINT('Ctrl Pts',(100.868941507161,1.4671163570085,-12.499783274278));
#55254=CARTESIAN_POINT('Ctrl Pts',(100.879218290784,1.57807738894463,-12.49968175614));
#55255=CARTESIAN_POINT('Ctrl Pts',(100.890313799386,1.68901725126355,-12.4995884691532));
#55256=CARTESIAN_POINT('',(99.0760280851,1.68935314531928,-12.5));
#55257=CARTESIAN_POINT('Ctrl Pts',(99.0760280851,1.68926961768441,-12.4990067873254));
#55258=CARTESIAN_POINT('Ctrl Pts',(99.0983723450034,2.65676718946135,-12.3683919466809));
#55259=CARTESIAN_POINT('Ctrl Pts',(99.1207166049067,3.60921449755032,-12.1266511028957));
#55260=CARTESIAN_POINT('Ctrl Pts',(99.1430608648101,4.52023710773274,-11.7769827456882));
#55261=CARTESIAN_POINT('Ctrl Pts',(99.190377283491,6.44942730859747,-11.0365216849666));
#55262=CARTESIAN_POINT('Ctrl Pts',(99.2376937021719,8.19285796673946,-9.81208448069556));
#55263=CARTESIAN_POINT('Ctrl Pts',(99.2850101208527,9.54407406006468,-8.24866755565912));
#55264=CARTESIAN_POINT('Ctrl Pts',(99.3323265395336,10.8952901533899,-6.68525063062268));
#55265=CARTESIAN_POINT('Ctrl Pts',(99.3796429582144,11.8542916818983,-4.78285398482082));
#55266=CARTESIAN_POINT('Ctrl Pts',(99.4269593768953,12.3075148043826,-2.76675720779547));
#55267=CARTESIAN_POINT('Ctrl Pts',(99.4742757955762,12.7607379268669,-0.750660430770102));
#55268=CARTESIAN_POINT('Ctrl Pts',(99.5215922142571,12.708182643327,1.37913647747874));
#55269=CARTESIAN_POINT('Ctrl Pts',(99.568908632938,12.1560724891477,3.37042545459742));
#55270=CARTESIAN_POINT('Ctrl Pts',(99.6162250516189,11.6039623349683,5.3617144317161));
#55271=CARTESIAN_POINT('Ctrl Pts',(99.6635414702997,10.5522973101494,7.2144954777046));
#55272=CARTESIAN_POINT('Ctrl Pts',(99.7108578889806,9.12561435869646,8.70936442476912));
#55273=CARTESIAN_POINT('Ctrl Pts',(99.7581743076614,7.69893140724353,10.2042333718336));
#55274=CARTESIAN_POINT('Ctrl Pts',(99.8054907263423,5.89723052915655,11.3411902199742));
#55275=CARTESIAN_POINT('Ctrl Pts',(99.8528071450232,3.93386703831174,11.9855978670874));
#55276=CARTESIAN_POINT('Ctrl Pts',(99.9001235637041,1.97050354746692,12.6300055142007));
#55277=CARTESIAN_POINT('Ctrl Pts',(99.947439982385,-0.154522556135726,12.7818639602866));
#55278=CARTESIAN_POINT('Ctrl Pts',(99.9947564010659,-2.18956816304055,12.4231903054835));
#55279=CARTESIAN_POINT('Ctrl Pts',(100.042072819747,-4.22461376994535,12.0645166506804));
#55280=CARTESIAN_POINT('Ctrl Pts',(100.089389238428,-6.16967888015232,11.1953108949882));
#55281=CARTESIAN_POINT('Ctrl Pts',(100.136705657109,-7.79443115486138,9.91850336890124));
#55282=CARTESIAN_POINT('Ctrl Pts',(100.184022075789,-9.41918342957046,8.64169584281428));
#55283=CARTESIAN_POINT('Ctrl Pts',(100.23133849447,-10.7236228687816,6.95728654633254));
#55284=CARTESIAN_POINT('Ctrl Pts',(100.278654913151,-11.5532792775025,5.06474126119284));
#55285=CARTESIAN_POINT('Ctrl Pts',(100.325971331832,-12.3829356862234,3.17219597605314));
#55286=CARTESIAN_POINT('Ctrl Pts',(100.373287750513,-12.737809064454,1.07151470225547));
#55287=CARTESIAN_POINT('Ctrl Pts',(100.420604169194,-12.5758757211841,-0.988542337046582));
#55288=CARTESIAN_POINT('Ctrl Pts',(100.467920587875,-12.4139423779141,-3.04859937634864));
#55289=CARTESIAN_POINT('Ctrl Pts',(100.515237006556,-11.7352023131437,-5.06803218115509));
#55290=CARTESIAN_POINT('Ctrl Pts',(100.562553425236,-10.6200311326729,-6.80770187712794));
#55291=CARTESIAN_POINT('Ctrl Pts',(100.609869843917,-9.5048599522022,-8.5473715731008));
#55292=CARTESIAN_POINT('Ctrl Pts',(100.657186262598,-7.95325765603118,-10.00727816024));
#55293=CARTESIAN_POINT('Ctrl Pts',(100.704502681279,-6.14896317602482,-11.0145412054561));
#55294=CARTESIAN_POINT('Ctrl Pts',(100.740580135996,-4.77323876125789,-11.7825512940261));
#55295=CARTESIAN_POINT('Ctrl Pts',(100.776657590713,-3.25060823709326,-12.2874107750916));
#55296=CARTESIAN_POINT('Ctrl Pts',(100.81273504543,-1.68904687944152,-12.5000065800333));
#55297=CARTESIAN_POINT('',(98.9984493311445,-1.68935314531929,-12.5));
#55298=CARTESIAN_POINT('Ctrl Pts',(98.9984493311444,-1.68945110984984,-12.5010138634865));
#55299=CARTESIAN_POINT('Ctrl Pts',(98.9979474259811,-1.6802677427303,-12.5010150828114));
#55300=CARTESIAN_POINT('Ctrl Pts',(98.9974512546758,-1.67108405301431,-12.5010161252244));
#55301=CARTESIAN_POINT('Ctrl Pts',(98.9969608216067,-1.66190002447542,-12.5010169855558));
#55302=CARTESIAN_POINT('Ctrl Pts',(98.9953653343946,-1.63202234898023,-12.5010197844042));
#55303=CARTESIAN_POINT('Ctrl Pts',(98.993830837603,-1.60214584008525,-12.501020667113));
#55304=CARTESIAN_POINT('Ctrl Pts',(98.9923574210217,-1.57226996295488,-12.5010194467146));
#55305=CARTESIAN_POINT('Ctrl Pts',(98.9800706385758,-1.32313580271385,-12.501009269844));
#55306=CARTESIAN_POINT('Ctrl Pts',(98.9720312814802,-1.0740498127315,-12.5008541512912));
#55307=CARTESIAN_POINT('Ctrl Pts',(98.9682914170034,-0.824698135317126,
-12.5006462662282));
#55308=CARTESIAN_POINT('Ctrl Pts',(98.9671276888522,-0.747107739094962,
-12.5005815789376));
#55309=CARTESIAN_POINT('Ctrl Pts',(98.9663802627598,-0.669491254130434,
-12.5005116497004));
#55310=CARTESIAN_POINT('Ctrl Pts',(98.9660507074694,-0.591838307311,-12.5004388277769));
#55311=CARTESIAN_POINT('Ctrl Pts',(98.9652977264628,-0.414413772565412,
-12.5002724413558));
#55312=CARTESIAN_POINT('Ctrl Pts',(98.9667272816058,-0.237059727277439,
-12.5000915331407));
#55313=CARTESIAN_POINT('Ctrl Pts',(98.9703388892135,-0.0596558322633638,
-12.4999195073644));
#55314=CARTESIAN_POINT('Ctrl Pts',(98.9706081879978,-0.0464277470335215,
-12.4999066802975));
#55315=CARTESIAN_POINT('Ctrl Pts',(98.970889608187,-0.0331999056257905,
-12.4998939000497));
#55316=CARTESIAN_POINT('Ctrl Pts',(98.9711831467108,-0.019972258301805,
-12.4998811748209));
#55317=CARTESIAN_POINT('Ctrl Pts',(98.9712637987576,-0.0163378568726815,
-12.4998776784629));
#55318=CARTESIAN_POINT('Ctrl Pts',(98.971345365564,-0.0127034735610646,
-12.4998741862605));
#55319=CARTESIAN_POINT('Ctrl Pts',(98.9714278470603,-0.00906910737247381,
-12.499870698381));
#55320=CARTESIAN_POINT('Ctrl Pts',(98.9714763003207,-0.00693412074554248,
-12.4998686494471));
#55321=CARTESIAN_POINT('Ctrl Pts',(98.9715250692229,-0.00479914042401758,
-12.4998666020053));
#55322=CARTESIAN_POINT('Ctrl Pts',(98.971574153754,-0.00266416613580766,
-12.4998645560894));
#55323=CARTESIAN_POINT('Ctrl Pts',(98.9716165319915,-0.000820887908404128,
-12.4998627897016));
#55324=CARTESIAN_POINT('Ctrl Pts',(98.9716591454966,0.00102238556451054,
-12.4998610244515));
#55325=CARTESIAN_POINT('Ctrl Pts',(98.9717019942601,0.00286565441603858,
-12.4998592603605));
#55326=CARTESIAN_POINT('Ctrl Pts',(98.9717541779398,0.00511049285387701,
-12.4998571119494));
#55327=CARTESIAN_POINT('Ctrl Pts',(98.9718067105416,0.00735532411911638,
-12.499854965258));
#55328=CARTESIAN_POINT('Ctrl Pts',(98.9718595920468,0.00960014839710077,
-12.499852820325));
#55329=CARTESIAN_POINT('Ctrl Pts',(98.9719593605523,0.0138353297160231,
-12.4998487736029));
#55330=CARTESIAN_POINT('Ctrl Pts',(98.9720603709144,0.018070484562572,-12.4998447331417));
#55331=CARTESIAN_POINT('Ctrl Pts',(98.9721626230162,0.0223056146626419,
-12.4998406992006));
#55332=CARTESIAN_POINT('Ctrl Pts',(98.9727450549982,0.0464290817843739,
-12.4998177217141));
#55333=CARTESIAN_POINT('Ctrl Pts',(98.9733677688012,0.0705514868195058,
-12.4997949562095));
#55334=CARTESIAN_POINT('Ctrl Pts',(98.9740307398311,0.094673130418238,-12.4997724491959));
#55335=CARTESIAN_POINT('Ctrl Pts',(98.9748783930467,0.125514280088803,-12.4997436724596));
#55336=CARTESIAN_POINT('Ctrl Pts',(98.9757918339131,0.156353375762838,-12.4997153192498));
#55337=CARTESIAN_POINT('Ctrl Pts',(98.9767710005896,0.187191043402697,-12.4996874810608));
#55338=CARTESIAN_POINT('Ctrl Pts',(98.9815927965995,0.339047664282832,-12.4995503950348));
#55339=CARTESIAN_POINT('Ctrl Pts',(98.9880063803661,0.490805467490059,-12.4994261570224));
#55340=CARTESIAN_POINT('Ctrl Pts',(98.9960002547573,0.642537640964607,-12.499323396877));
#55341=CARTESIAN_POINT('Ctrl Pts',(99.008622407575,0.882119424117457,-12.4991611408552));
#55342=CARTESIAN_POINT('Ctrl Pts',(99.0251629778626,1.12122192559231,-12.4990545261512));
#55343=CARTESIAN_POINT('Ctrl Pts',(99.0455338141878,1.36011436106045,-12.499016424172));
#55344=CARTESIAN_POINT('Ctrl Pts',(99.0548929207919,1.46987027558398,-12.4989989187304));
#55345=CARTESIAN_POINT('Ctrl Pts',(99.0650605273681,1.57958119595339,-12.4989956130992));
#55346=CARTESIAN_POINT('Ctrl Pts',(99.0760280851,1.68926961768503,-12.4990067873254));
#55347=CARTESIAN_POINT('Ctrl Pts',(97.2617423708144,1.68963646449132,-12.4998270697761));
#55348=CARTESIAN_POINT('Ctrl Pts',(97.2737350926282,2.20887124184649,-12.4301620153288));
#55349=CARTESIAN_POINT('Ctrl Pts',(97.285727814442,2.72368641886456,-12.3282504960299));
#55350=CARTESIAN_POINT('Ctrl Pts',(97.2977205362559,3.22997473648381,-12.1941459828224));
#55351=CARTESIAN_POINT('Ctrl Pts',(97.3450369549367,5.22749876660567,-11.6650463011637));
#55352=CARTESIAN_POINT('Ctrl Pts',(97.3923533736176,7.09229028452064,-10.6348175686913));
#55353=CARTESIAN_POINT('Ctrl Pts',(97.4396697922984,8.6035177604385,-9.22547184209238));
#55354=CARTESIAN_POINT('Ctrl Pts',(97.4869862109793,10.1147452363564,-7.81612611549341));
#55355=CARTESIAN_POINT('Ctrl Pts',(97.5343026296602,11.2724086702771,-6.02766339476788));
#55356=CARTESIAN_POINT('Ctrl Pts',(97.5816190483411,11.9394213573864,-4.07186482841795));
#55357=CARTESIAN_POINT('Ctrl Pts',(97.628935467022,12.6064340444957,-2.11606626206803));
#55358=CARTESIAN_POINT('Ctrl Pts',(97.6762518857028,12.7827959847935,0.00706814990629356));
#55359=CARTESIAN_POINT('Ctrl Pts',(97.7235683043837,12.447621428183,2.04611617989715));
#55360=CARTESIAN_POINT('Ctrl Pts',(97.7708847230646,12.1124468715726,4.085164209888));
#55361=CARTESIAN_POINT('Ctrl Pts',(97.8182011417455,11.2657358180539,6.04012585789538));
#55362=CARTESIAN_POINT('Ctrl Pts',(97.8655175604264,10.0077553660322,7.67949835174444));
#55363=CARTESIAN_POINT('Ctrl Pts',(97.9128339791073,8.74977491401052,9.3188708455935));
#55364=CARTESIAN_POINT('Ctrl Pts',(97.9601503977881,7.08052506348581,10.6426541852842));
#55365=CARTESIAN_POINT('Ctrl Pts',(98.007466816469,5.19767616134277,11.4940867719376));
#55366=CARTESIAN_POINT('Ctrl Pts',(98.0547832351499,3.31482725919971,12.345519358591));
#55367=CARTESIAN_POINT('Ctrl Pts',(98.1020996538307,1.21837930543832,12.724601192207));
#55368=CARTESIAN_POINT('Ctrl Pts',(98.1494160725116,-0.843408651483552,
12.586442191364));
#55369=CARTESIAN_POINT('Ctrl Pts',(98.1967324911925,-2.90519660840542,12.4482831905211));
#55370=CARTESIAN_POINT('Ctrl Pts',(98.2440489098734,-4.93232456848778,11.7928833552192));
#55371=CARTESIAN_POINT('Ctrl Pts',(98.2913653285542,-6.68474246857545,10.6978542021024));
#55372=CARTESIAN_POINT('Ctrl Pts',(98.3386817472351,-8.43716036866312,9.60282504898553));
#55373=CARTESIAN_POINT('Ctrl Pts',(98.385998165916,-9.91486820875611,8.0681665780538));
#55374=CARTESIAN_POINT('Ctrl Pts',(98.4333145845969,-10.9428775221743,6.27561133310073));
#55375=CARTESIAN_POINT('Ctrl Pts',(98.4806310032778,-11.9708868355925,4.48305608814765));
#55376=CARTESIAN_POINT('Ctrl Pts',(98.5279474219587,-12.5491976223359,2.43260406917324));
#55377=CARTESIAN_POINT('Ctrl Pts',(98.5752638406395,-12.6093270088307,0.367067371252128));
#55378=CARTESIAN_POINT('Ctrl Pts',(98.6225802593204,-12.6694563953254,-1.69846932666899));
#55379=CARTESIAN_POINT('Ctrl Pts',(98.6698966780013,-12.2114043815716,-3.77909070353679));
#55380=CARTESIAN_POINT('Ctrl Pts',(98.7172130966822,-11.28941294518,-5.62841198733738));
#55381=CARTESIAN_POINT('Ctrl Pts',(98.7645295153631,-10.3674215087885,-7.47773327113796));
#55382=CARTESIAN_POINT('Ctrl Pts',(98.811845934044,-8.98149064975927,-9.09575446187132));
#55383=CARTESIAN_POINT('Ctrl Pts',(98.8591623527248,-7.29574068517416,-10.2908713885963));
#55384=CARTESIAN_POINT('Ctrl Pts',(98.9055913455314,-5.64160719068382,-11.4635737346495));
#55385=CARTESIAN_POINT('Ctrl Pts',(98.9520203383379,-3.69879542401664,-12.2290863120461));
#55386=CARTESIAN_POINT('Ctrl Pts',(98.9984493311445,-1.68945110984913,-12.5010138634866));
#55387=CARTESIAN_POINT('Ctrl Pts',(107.547344722949,1.01347785817195,-11.5532729648613));
#55388=CARTESIAN_POINT('Ctrl Pts',(107.609159016559,3.48672851139089,-11.3363141184487));
#55389=CARTESIAN_POINT('Ctrl Pts',(107.701880456974,7.0775262685878,-9.77461236926229));
#55390=CARTESIAN_POINT('Ctrl Pts',(107.825509044195,10.2343745743181,-5.85997992529276));
#55391=CARTESIAN_POINT('Ctrl Pts',(107.949137631415,12.0158490350764,-1.15276339618737));
#55392=CARTESIAN_POINT('Ctrl Pts',(108.072766218635,11.3809885644172,4.02471057714319));
#55393=CARTESIAN_POINT('Ctrl Pts',(108.227301952661,7.79854554867288,9.20330948728365));
#55394=CARTESIAN_POINT('Ctrl Pts',(108.320023393076,4.34404808711794,11.0362375708885));
#55395=CARTESIAN_POINT('Ctrl Pts',(108.381837686686,1.89465380507476,11.4418329182223));
#55396=CARTESIAN_POINT('Ctrl Pts',(107.742874014115,1.04307277299664,-11.8906440545054));
#55397=CARTESIAN_POINT('Ctrl Pts',(107.804688307725,3.58854566751268,-11.667349718345));
#55398=CARTESIAN_POINT('Ctrl Pts',(107.89740974814,7.28419954260115,-10.0600441803081));
#55399=CARTESIAN_POINT('Ctrl Pts',(108.02103833536,10.5332320593325,-6.03109921059844));
#55400=CARTESIAN_POINT('Ctrl Pts',(108.144666922581,12.3667279673315,-1.18642563581908));
#55401=CARTESIAN_POINT('Ctrl Pts',(108.268295509801,11.7133287181453,4.14223753223569));
#55402=CARTESIAN_POINT('Ctrl Pts',(108.422831243826,8.0262735541824,9.47205848676629));
#55403=CARTESIAN_POINT('Ctrl Pts',(108.515552684241,4.47090012645561,11.3585105325147));
#55404=CARTESIAN_POINT('Ctrl Pts',(108.577366977851,1.94998024119902,11.7759498088114));
#55405=CARTESIAN_POINT('Ctrl Pts',(107.93840330528,1.07266768782132,-12.2280151441495));
#55406=CARTESIAN_POINT('Ctrl Pts',(108.00021759889,3.69036282363445,-11.9983853182413));
#55407=CARTESIAN_POINT('Ctrl Pts',(108.092939039306,7.49087281661451,-10.3454759913538));
#55408=CARTESIAN_POINT('Ctrl Pts',(108.216567626526,10.8320895443469,-6.20221849590413));
#55409=CARTESIAN_POINT('Ctrl Pts',(108.340196213746,12.7176068995866,-1.2200878754508));
#55410=CARTESIAN_POINT('Ctrl Pts',(108.463824800966,12.0456688718733,4.25976448732819));
#55411=CARTESIAN_POINT('Ctrl Pts',(108.618360534992,8.25400155969191,9.74080748624894));
#55412=CARTESIAN_POINT('Ctrl Pts',(108.711081975407,4.59775216579328,11.6807834941409));
#55413=CARTESIAN_POINT('Ctrl Pts',(108.772896269017,2.00530667732328,12.1100666994004));
#55414=CARTESIAN_POINT('Ctrl Pts',(108.133932596446,1.10226260264601,-12.5653862337935));
#55415=CARTESIAN_POINT('Ctrl Pts',(108.195746890056,3.79217997975623,-12.3294209181376));
#55416=CARTESIAN_POINT('Ctrl Pts',(108.288468330471,7.69754609062786,-10.6309078023996));
#55417=CARTESIAN_POINT('Ctrl Pts',(108.412096917691,11.1309470293613,-6.37333778120981));
#55418=CARTESIAN_POINT('Ctrl Pts',(108.535725504912,13.0684858318418,-1.2537501150825));
#55419=CARTESIAN_POINT('Ctrl Pts',(108.659354092132,12.3780090256014,4.37729144242069));
#55420=CARTESIAN_POINT('Ctrl Pts',(108.813889826157,8.48172956520142,10.0095564857316));
#55421=CARTESIAN_POINT('Ctrl Pts',(108.906611266572,4.72460420513094,12.0030564557671));
#55422=CARTESIAN_POINT('Ctrl Pts',(108.968425560183,2.06063311344754,12.4441835899895));
#55423=CARTESIAN_POINT('',(108.966713351645,2.13438641081836,12.4317460036358));
#55424=CARTESIAN_POINT('Ctrl Pts',(108.966713351645,2.13438197832376,12.4317378478958));
#55425=CARTESIAN_POINT('Ctrl Pts',(108.904270759855,2.11878011600994,12.3247891977871));
#55426=CARTESIAN_POINT('Ctrl Pts',(108.841707114744,2.10024321437466,12.2180180253493));
#55427=CARTESIAN_POINT('Ctrl Pts',(108.779287547041,2.07859884281513,12.111899302578));
#55428=CARTESIAN_POINT('Ctrl Pts',(108.744012990319,2.06636717187634,12.051929471908));
#55429=CARTESIAN_POINT('Ctrl Pts',(108.708784446274,2.05314400460933,11.9921676130932));
#55430=CARTESIAN_POINT('Ctrl Pts',(108.673649764967,2.03890467453726,11.9326960190957));
#55431=CARTESIAN_POINT('Ctrl Pts',(108.614852890925,2.01507556707034,11.8331720248194));
#55432=CARTESIAN_POINT('Ctrl Pts',(108.556034583919,1.98828429254243,11.7339812222009));
#55433=CARTESIAN_POINT('Ctrl Pts',(108.497516928003,1.95832745664509,11.6356749683345));
#55434=CARTESIAN_POINT('Ctrl Pts',(108.458794424042,1.93850431645706,11.5706234168811));
#55435=CARTESIAN_POINT('Ctrl Pts',(108.420203568548,1.91729608573862,11.5059586389564));
#55436=CARTESIAN_POINT('Ctrl Pts',(108.381837686686,1.89465380507476,11.4418329182223));
#55437=CARTESIAN_POINT('',(108.14853343171,1.73584852417216,-12.4932937197078));
#55438=CARTESIAN_POINT('Ctrl Pts',(108.14853343171,1.73578194556693,-12.4930929274479));
#55439=CARTESIAN_POINT('Ctrl Pts',(108.205480780232,4.19849975430616,-12.1469930389749));
#55440=CARTESIAN_POINT('Ctrl Pts',(108.262428128754,6.55419777563119,-11.0556206944382));
#55441=CARTESIAN_POINT('Ctrl Pts',(108.319375477276,8.40808350233105,-9.40044147486277));
#55442=CARTESIAN_POINT('Ctrl Pts',(108.350282624081,9.41424655999455,-8.50212279180473));
#55443=CARTESIAN_POINT('Ctrl Pts',(108.381189770886,10.2725967946779,-7.43773028650731));
#55444=CARTESIAN_POINT('Ctrl Pts',(108.412096917691,10.9439642623296,-6.2655855755927));
#55445=CARTESIAN_POINT('Ctrl Pts',(108.443004064496,11.6153317299814,-5.09344086467804));
#55446=CARTESIAN_POINT('Ctrl Pts',(108.473911211301,12.0997164306015,-3.81354394814619));
#55447=CARTESIAN_POINT('Ctrl Pts',(108.504818358107,12.3650998304949,-2.49102587399968));
#55448=CARTESIAN_POINT('Ctrl Pts',(108.566632651717,12.8958666302817,0.154010274293264));
#55449=CARTESIAN_POINT('Ctrl Pts',(108.628446945327,12.5506282271615,2.96953105304482));
#55450=CARTESIAN_POINT('Ctrl Pts',(108.690261238937,11.3965409033481,5.40997532417824));
#55451=CARTESIAN_POINT('Ctrl Pts',(108.721168385742,10.8194972414414,6.63019745974499));
#55452=CARTESIAN_POINT('Ctrl Pts',(108.752075532547,10.0402413493614,7.75665046840719));
#55453=CARTESIAN_POINT('Ctrl Pts',(108.782982679352,9.10327904796693,8.72911913751927));
#55454=CARTESIAN_POINT('Ctrl Pts',(108.844226236783,7.246656536744,10.6560987180694));
#55455=CARTESIAN_POINT('Ctrl Pts',(108.905469794214,4.77080353486937,11.9784624269707));
#55456=CARTESIAN_POINT('Ctrl Pts',(108.966713351645,2.13438197832402,12.4317378478958));
#55457=CARTESIAN_POINT('Ctrl Pts',(107.547344722949,1.01347785817195,-11.5532729648613));
#55458=CARTESIAN_POINT('Ctrl Pts',(107.555157200122,1.02853006148911,-11.5649311188494));
#55459=CARTESIAN_POINT('Ctrl Pts',(107.563081485634,1.04337171979055,-11.5767876635257));
#55460=CARTESIAN_POINT('Ctrl Pts',(107.571107356017,1.05800344929602,-11.5888274417128));
#55461=CARTESIAN_POINT('Ctrl Pts',(107.601592993975,1.11358092402132,-11.6345595930381));
#55462=CARTESIAN_POINT('Ctrl Pts',(107.633652536267,1.16633032082653,-11.6830998317929));
#55463=CARTESIAN_POINT('Ctrl Pts',(107.666874561659,1.2163822695299,-11.7338367536604));
#55464=CARTESIAN_POINT('Ctrl Pts',(107.703659888335,1.27180264989783,-11.7900155754933));
#55465=CARTESIAN_POINT('Ctrl Pts',(107.741870440797,1.32391544230277,-11.8488877529446));
#55466=CARTESIAN_POINT('Ctrl Pts',(107.780947707395,1.37283791092559,-11.9095908316944));
#55467=CARTESIAN_POINT('Ctrl Pts',(107.811334718166,1.41088068388255,-11.9567943663416));
#55468=CARTESIAN_POINT('Ctrl Pts',(107.842245816055,1.44699286001964,-12.0051043086855));
#55469=CARTESIAN_POINT('Ctrl Pts',(107.873418383575,1.48121215166239,-12.0541027667175));
#55470=CARTESIAN_POINT('Ctrl Pts',(107.923912309557,1.53664122013029,-12.1334714138957));
#55471=CARTESIAN_POINT('Ctrl Pts',(107.97573271635,1.58784070065421,-12.215649995053));
#55472=CARTESIAN_POINT('Ctrl Pts',(108.028235752821,1.63507762537721,-12.2995995033468));
#55473=CARTESIAN_POINT('Ctrl Pts',(108.068036194817,1.6708860396869,-12.3632382518832));
#55474=CARTESIAN_POINT('Ctrl Pts',(108.108228913152,1.70441636021813,-12.4278934158814));
#55475=CARTESIAN_POINT('Ctrl Pts',(108.14853343171,1.73578194556773,-12.4930929274478));
#55476=CARTESIAN_POINT('Ctrl Pts',(108.477958351107,-1.94818655881014,11.4328396604549));
#55477=CARTESIAN_POINT('Ctrl Pts',(108.53784915696,-4.31949723671962,11.0287619573935));
#55478=CARTESIAN_POINT('Ctrl Pts',(108.627685365739,-7.67204750982751,9.27780206687928));
#55479=CARTESIAN_POINT('Ctrl Pts',(108.747466977445,-10.5120654759104,5.32006485465251));
#55480=CARTESIAN_POINT('Ctrl Pts',(108.86724858915,-12.0211681894647,0.692105791054637));
#55481=CARTESIAN_POINT('Ctrl Pts',(109.016975603782,-11.068234710412,-5.54964839940795));
#55482=CARTESIAN_POINT('Ctrl Pts',(109.166702618414,-6.63827437718498,-10.0475317645548));
#55483=CARTESIAN_POINT('Ctrl Pts',(109.256538827193,-3.17834332867996,-11.2182879948304));
#55484=CARTESIAN_POINT('Ctrl Pts',(109.286484230119,-1.99349831895978,-11.4250259527891));
#55485=CARTESIAN_POINT('Ctrl Pts',(108.673487642273,-2.00507622325195,11.7666939358369));
#55486=CARTESIAN_POINT('Ctrl Pts',(108.733378448126,-4.44563235824741,11.3508166210639));
#55487=CARTESIAN_POINT('Ctrl Pts',(108.823214656905,-7.89608160268274,9.54872634974918));
#55488=CARTESIAN_POINT('Ctrl Pts',(108.94299626861,-10.8190319082629,5.47541789464821));
#55489=CARTESIAN_POINT('Ctrl Pts',(109.062777880316,-12.372202448173,0.712316209832714));
#55490=CARTESIAN_POINT('Ctrl Pts',(109.212504894948,-11.3914420314928,-5.71170558730129));
#55491=CARTESIAN_POINT('Ctrl Pts',(109.362231909579,-6.83212090593912,-10.3409331885453));
#55492=CARTESIAN_POINT('Ctrl Pts',(109.452068118358,-3.27115522322458,-11.545877073377));
#55493=CARTESIAN_POINT('Ctrl Pts',(109.482013521285,-2.05171114766354,-11.7586520574114));
#55494=CARTESIAN_POINT('Ctrl Pts',(108.869016933439,-2.06196588769375,12.1005482112188));
#55495=CARTESIAN_POINT('Ctrl Pts',(108.928907739291,-4.5717674797752,11.6728712847344));
#55496=CARTESIAN_POINT('Ctrl Pts',(109.01874394807,-8.12011569553795,9.81965063261907));
#55497=CARTESIAN_POINT('Ctrl Pts',(109.138525559776,-11.1259983406154,5.63077093464392));
#55498=CARTESIAN_POINT('Ctrl Pts',(109.258307171481,-12.7232367068813,0.732526628610785));
#55499=CARTESIAN_POINT('Ctrl Pts',(109.408034186113,-11.7146493525736,-5.87376277519463));
#55500=CARTESIAN_POINT('Ctrl Pts',(109.557761200745,-7.02596743469325,-10.6343346125358));
#55501=CARTESIAN_POINT('Ctrl Pts',(109.647597409524,-3.3639671177692,-11.8734661519237));
#55502=CARTESIAN_POINT('Ctrl Pts',(109.67754281245,-2.1099239763673,-12.0922781620336));
#55503=CARTESIAN_POINT('Ctrl Pts',(109.064546224604,-2.11885555213556,12.4344024866008));
#55504=CARTESIAN_POINT('Ctrl Pts',(109.124437030457,-4.69790260130299,11.9949259484048));
#55505=CARTESIAN_POINT('Ctrl Pts',(109.214273239236,-8.34414978839318,10.090574915489));
#55506=CARTESIAN_POINT('Ctrl Pts',(109.334054850941,-11.4329647729678,5.78612397463963));
#55507=CARTESIAN_POINT('Ctrl Pts',(109.453836462647,-13.0742709655896,0.752737047388862));
#55508=CARTESIAN_POINT('Ctrl Pts',(109.603563477279,-12.0378566736544,-6.03581996308797));
#55509=CARTESIAN_POINT('Ctrl Pts',(109.75329049191,-7.21981396344739,-10.9277360365263));
#55510=CARTESIAN_POINT('Ctrl Pts',(109.84312670069,-3.45677901231382,-12.2010552304703));
#55511=CARTESIAN_POINT('Ctrl Pts',(109.873072103616,-2.16813680507106,-12.4259042666559));
#55512=CARTESIAN_POINT('',(109.873072103616,-2.16813680507102,-12.4259042666559));
#55513=CARTESIAN_POINT('',(109.281532350295,-2.18912582690727,-11.3891607102353));
#55514=CARTESIAN_POINT('Ctrl Pts',(109.873072103616,-2.16813680507115,-12.4259042666558));
#55515=CARTESIAN_POINT('Ctrl Pts',(109.802888483755,-2.18021332655258,-12.3017367690068));
#55516=CARTESIAN_POINT('Ctrl Pts',(109.732266767812,-2.1888609950872,-12.177170292616));
#55517=CARTESIAN_POINT('Ctrl Pts',(109.661457734895,-2.19407037232472,-12.0527002541065));
#55518=CARTESIAN_POINT('Ctrl Pts',(109.633303673289,-2.19614164941518,-12.0032102810333));
#55519=CARTESIAN_POINT('Ctrl Pts',(109.605119998715,-2.19766992928173,-11.95373538301));
#55520=CARTESIAN_POINT('Ctrl Pts',(109.576922474526,-2.19865677093697,-11.9043059834552));
#55521=CARTESIAN_POINT('Ctrl Pts',(109.510004507875,-2.20099872963269,-11.7870008296852));
#55522=CARTESIAN_POINT('Ctrl Pts',(109.442772533832,-2.20029775063903,-11.6695389907235));
#55523=CARTESIAN_POINT('Ctrl Pts',(109.375440744552,-2.19647822257344,-11.552340529106));
#55524=CARTESIAN_POINT('Ctrl Pts',(109.344152335973,-2.19470332610961,-11.4978795769887));
#55525=CARTESIAN_POINT('Ctrl Pts',(109.312842373612,-2.19225573972214,-11.4434752830729));
#55526=CARTESIAN_POINT('Ctrl Pts',(109.281532350295,-2.18913148123183,-11.3891685808071));
#55527=CARTESIAN_POINT('',(109.065424143392,-2.15665106701421,12.4279028892547));
#55528=CARTESIAN_POINT('Ctrl Pts',(109.065424143392,-2.15665025088522,12.4279009233094));
#55529=CARTESIAN_POINT('Ctrl Pts',(109.125022309649,-4.72164364222117,11.982505130978));
#55530=CARTESIAN_POINT('Ctrl Pts',(109.184620475906,-7.13772412654634,10.716279968349));
#55531=CARTESIAN_POINT('Ctrl Pts',(109.244218642162,-8.96861620690796,8.86735249441881));
#55532=CARTESIAN_POINT('Ctrl Pts',(109.274164045089,-9.88855728068048,7.93834944506434));
#55533=CARTESIAN_POINT('Ctrl Pts',(109.304109448015,-10.6607610268242,6.86223670985195));
#55534=CARTESIAN_POINT('Ctrl Pts',(109.334054850941,-11.2520261739738,5.69500697633937));
#55535=CARTESIAN_POINT('Ctrl Pts',(109.364000253868,-11.8432913211233,4.52777724282685));
#55536=CARTESIAN_POINT('Ctrl Pts',(109.393945656794,-12.2536178692787,3.26943051101414));
#55537=CARTESIAN_POINT('Ctrl Pts',(109.42389105972,-12.4580746152533,1.97796222244055));
#55538=CARTESIAN_POINT('Ctrl Pts',(109.483781865573,-12.8669881072025,-0.60497435470658));
#55539=CARTESIAN_POINT('Ctrl Pts',(109.543672671426,-12.4524223904284,-3.32039715889727));
#55540=CARTESIAN_POINT('Ctrl Pts',(109.603563477279,-11.28153099,-5.65649177568027));
#55541=CARTESIAN_POINT('Ctrl Pts',(109.663454283131,-10.1106395895716,-7.99258639246326));
#55542=CARTESIAN_POINT('Ctrl Pts',(109.723345088984,-8.18342250548884,-9.94935282183856));
#55543=CARTESIAN_POINT('Ctrl Pts',(109.783235894837,-5.86855683251303,-11.1675279400499));
#55544=CARTESIAN_POINT('Ctrl Pts',(109.813181297763,-4.7111239960251,-11.7766154991556));
#55545=CARTESIAN_POINT('Ctrl Pts',(109.84312670069,-3.4567790123139,-12.2010552304703));
#55546=CARTESIAN_POINT('Ctrl Pts',(109.873072103616,-2.16813680507115,-12.4259042666558));
#55547=CARTESIAN_POINT('',(108.477958351107,-1.9481865588103,11.4328396604549));
#55548=CARTESIAN_POINT('Ctrl Pts',(108.477958351107,-1.9481865588103,11.4328396604549));
#55549=CARTESIAN_POINT('Ctrl Pts',(108.478836583785,-1.94864729003221,11.434295047288));
#55550=CARTESIAN_POINT('Ctrl Pts',(108.479714849452,-1.94910728118743,11.4357506492995));
#55551=CARTESIAN_POINT('Ctrl Pts',(108.480593146676,-1.949566532967,11.437206463898));
#55552=CARTESIAN_POINT('Ctrl Pts',(108.538946250772,-1.98007871742698,11.5339291888642));
#55553=CARTESIAN_POINT('Ctrl Pts',(108.597609547501,-2.00742552408462,11.6318734233243));
#55554=CARTESIAN_POINT('Ctrl Pts',(108.656284391412,-2.03178856868386,11.7304879191871));
#55555=CARTESIAN_POINT('Ctrl Pts',(108.695850475067,-2.04821724912794,11.796986424047));
#55556=CARTESIAN_POINT('Ctrl Pts',(108.735421809435,-2.06328990179688,11.8637890556732));
#55557=CARTESIAN_POINT('Ctrl Pts',(108.774906821129,-2.07707374906138,11.9307197670003));
#55558=CARTESIAN_POINT('Ctrl Pts',(108.837124803449,-2.09879346316566,12.0361849456926));
#55559=CARTESIAN_POINT('Ctrl Pts',(108.899470076242,-2.11742830718139,12.1425486267099));
#55560=CARTESIAN_POINT('Ctrl Pts',(108.961695535961,-2.13312920500828,12.249330872859));
#55561=CARTESIAN_POINT('Ctrl Pts',(108.996323035935,-2.14186651030987,12.3087535310842));
#55562=CARTESIAN_POINT('Ctrl Pts',(109.030913432804,-2.14969603440291,12.3683053914907));
#55563=CARTESIAN_POINT('Ctrl Pts',(109.065424143392,-2.15665025088575,12.4279009233093));
#55564=CARTESIAN_POINT('Ctrl Pts',(108.477958351107,-1.94818655881014,11.4328396604549));
#55565=CARTESIAN_POINT('Ctrl Pts',(108.53784915696,-4.31949723671962,11.0287619573935));
#55566=CARTESIAN_POINT('Ctrl Pts',(108.627685365739,-7.67204750982751,9.27780206687928));
#55567=CARTESIAN_POINT('Ctrl Pts',(108.747466977445,-10.5120654759104,5.32006485465251));
#55568=CARTESIAN_POINT('Ctrl Pts',(108.86724858915,-12.0211681894647,0.692105791054637));
#55569=CARTESIAN_POINT('Ctrl Pts',(109.016975603782,-11.068234710412,-5.54964839940795));
#55570=CARTESIAN_POINT('Ctrl Pts',(109.165051991806,-6.687111324995,-9.99794601691013));
#55571=CARTESIAN_POINT('Ctrl Pts',(109.253237573977,-3.30521629928841,-11.1747498326638));
#55572=CARTESIAN_POINT('Ctrl Pts',(109.281532350295,-2.18913148123183,-11.3891685808071));
#55573=CARTESIAN_POINT('Ctrl Pts',(109.38579409552,1.97561503404851,-11.4281319036333));
#55574=CARTESIAN_POINT('Ctrl Pts',(109.416044709093,3.17286165411581,-11.2211603319002));
#55575=CARTESIAN_POINT('Ctrl Pts',(109.506796549814,6.66901151712989,-10.0383350847298));
#55576=CARTESIAN_POINT('Ctrl Pts',(109.658049617681,11.1270467960305,-5.46893215383385));
#55577=CARTESIAN_POINT('Ctrl Pts',(109.809302685548,12.0200961191123,0.853135904503782));
#55578=CARTESIAN_POINT('Ctrl Pts',(109.930305139842,10.4208972763816,5.50447055552805));
#55579=CARTESIAN_POINT('Ctrl Pts',(110.051307594136,7.47576055358735,9.44837079282557));
#55580=CARTESIAN_POINT('Ctrl Pts',(110.142059434856,4.04474488933938,11.1377843017737));
#55581=CARTESIAN_POINT('Ctrl Pts',(110.202560662003,1.63912736726564,11.4812244574993));
#55582=CARTESIAN_POINT('Ctrl Pts',(109.581323386685,2.0333056468109,-11.7618487061923));
#55583=CARTESIAN_POINT('Ctrl Pts',(109.611574000259,3.26551347639981,-11.5488332865476));
#55584=CARTESIAN_POINT('Ctrl Pts',(109.702325840979,6.86375561165841,-10.3314679533159));
#55585=CARTESIAN_POINT('Ctrl Pts',(109.853578908847,11.4519715090114,-5.62863231893341));
#55586=CARTESIAN_POINT('Ctrl Pts',(110.004831976714,12.3710990719262,0.878048618900141));
#55587=CARTESIAN_POINT('Ctrl Pts',(110.125834431008,10.7252014748451,5.66520848969443));
#55588=CARTESIAN_POINT('Ctrl Pts',(110.246836885302,7.69406280365562,9.72427591161154));
#55589=CARTESIAN_POINT('Ctrl Pts',(110.337588726022,4.16285687325936,11.4630225643455));
#55590=CARTESIAN_POINT('Ctrl Pts',(110.398089953169,1.68699208816697,11.8164916339484));
#55591=CARTESIAN_POINT('Ctrl Pts',(109.776852677851,2.09099625957329,-12.0955655087513));
#55592=CARTESIAN_POINT('Ctrl Pts',(109.807103291424,3.3581652986838,-11.876506241195));
#55593=CARTESIAN_POINT('Ctrl Pts',(109.897855132145,7.05849970618694,-10.624600821902));
#55594=CARTESIAN_POINT('Ctrl Pts',(110.049108200012,11.7768962219922,-5.78833248403296));
#55595=CARTESIAN_POINT('Ctrl Pts',(110.200361267879,12.7221020247401,0.902961333296493));
#55596=CARTESIAN_POINT('Ctrl Pts',(110.321363722173,11.0295056733086,5.82594642386081));
#55597=CARTESIAN_POINT('Ctrl Pts',(110.442366176467,7.91236505372388,10.0001810303975));
#55598=CARTESIAN_POINT('Ctrl Pts',(110.533118017188,4.28096885717935,11.7882608269174));
#55599=CARTESIAN_POINT('Ctrl Pts',(110.593619244335,1.73485680906831,12.1517588103975));
#55600=CARTESIAN_POINT('Ctrl Pts',(109.972381969016,2.14868687233568,-12.4292823113103));
#55601=CARTESIAN_POINT('Ctrl Pts',(110.00263258259,3.45081712096779,-12.2041791958424));
#55602=CARTESIAN_POINT('Ctrl Pts',(110.09338442331,7.25324380071547,-10.917733690488));
#55603=CARTESIAN_POINT('Ctrl Pts',(110.244637491178,12.1018209349731,-5.94803264913252));
#55604=CARTESIAN_POINT('Ctrl Pts',(110.395890559045,13.073104977554,0.927874047692852));
#55605=CARTESIAN_POINT('Ctrl Pts',(110.516893013339,11.333809871772,5.98668435802718));
#55606=CARTESIAN_POINT('Ctrl Pts',(110.637895467633,8.13066730379214,10.2760861491835));
#55607=CARTESIAN_POINT('Ctrl Pts',(110.728647308353,4.39908084109933,12.1134990894893));
#55608=CARTESIAN_POINT('Ctrl Pts',(110.7891485355,1.78272152996964,12.4870259868466));
#55609=CARTESIAN_POINT('',(109.391405608182,2.19731819681764,-11.3875829881294));
#55610=CARTESIAN_POINT('',(109.972381969016,2.14868687233581,-12.4292823113103));
#55611=CARTESIAN_POINT('Ctrl Pts',(109.391405608182,2.1973257056837,-11.3875934426363));
#55612=CARTESIAN_POINT('Ctrl Pts',(109.392396565347,2.19737466243356,-11.3893444745));
#55613=CARTESIAN_POINT('Ctrl Pts',(109.39338746931,2.19742294454714,-11.3910955560154));
#55614=CARTESIAN_POINT('Ctrl Pts',(109.394378319473,2.19747055234629,-11.3928466858768));
#55615=CARTESIAN_POINT('Ctrl Pts',(109.461338464392,2.20068781490421,-11.51118537485));
#55616=CARTESIAN_POINT('Ctrl Pts',(109.528177183617,2.20083641292418,-11.6299636424174));
#55617=CARTESIAN_POINT('Ctrl Pts',(109.594689085937,2.19796783634277,-11.7487490106668));
#55618=CARTESIAN_POINT('Ctrl Pts',(109.624936761945,2.19666329126121,-11.8027691365074));
#55619=CARTESIAN_POINT('Ctrl Pts',(109.655116846808,2.19473541263824,-11.8567905206786));
#55620=CARTESIAN_POINT('Ctrl Pts',(109.685210022632,2.19219250554556,-11.9107715248805));
#55621=CARTESIAN_POINT('Ctrl Pts',(109.755294163322,2.18627031709048,-12.036488142997));
#55622=CARTESIAN_POINT('Ctrl Pts',(109.825179300418,2.17698401578315,-12.1624758836485));
#55623=CARTESIAN_POINT('Ctrl Pts',(109.894618363154,2.16432091039785,-12.2882242713375));
#55624=CARTESIAN_POINT('Ctrl Pts',(109.920606362969,2.15958166468455,-12.3352863851853));
#55625=CARTESIAN_POINT('Ctrl Pts',(109.946531882172,2.15436993164035,-12.3823148221297));
#55626=CARTESIAN_POINT('Ctrl Pts',(109.972381969016,2.14868687233568,-12.4292823113103));
#55627=CARTESIAN_POINT('',(110.191221970063,2.08852238929011,11.4078504030635));
#55628=CARTESIAN_POINT('Ctrl Pts',(109.391405608182,2.19732570568378,-11.3875934426363));
#55629=CARTESIAN_POINT('Ctrl Pts',(109.419785717535,3.31663241499189,-11.1717392207365));
#55630=CARTESIAN_POINT('Ctrl Pts',(109.508667054035,6.72414278767814,-9.98182656169961));
#55631=CARTESIAN_POINT('Ctrl Pts',(109.658049617681,11.1270467960305,-5.46893215383385));
#55632=CARTESIAN_POINT('Ctrl Pts',(109.809302685548,12.0200961191123,0.853135904503782));
#55633=CARTESIAN_POINT('Ctrl Pts',(109.930305139842,10.4208972763816,5.50447055552805));
#55634=CARTESIAN_POINT('Ctrl Pts',(110.047528030156,7.56775317257574,9.32518136360488));
#55635=CARTESIAN_POINT('Ctrl Pts',(110.134500306896,4.32840974362946,10.9948652468278));
#55636=CARTESIAN_POINT('Ctrl Pts',(110.191221970063,2.0884820668001,11.4077475491063));
#55637=CARTESIAN_POINT('',(110.7891485355,1.78272152996986,12.4870259868466));
#55638=CARTESIAN_POINT('Ctrl Pts',(110.7891485355,1.78272152996991,12.4870259868466));
#55639=CARTESIAN_POINT('Ctrl Pts',(110.73086285581,1.82486995155475,12.3813009097418));
#55640=CARTESIAN_POINT('Ctrl Pts',(110.671639795078,1.86334704785855,12.2739780744279));
#55641=CARTESIAN_POINT('Ctrl Pts',(110.611907449059,1.89832348357942,12.1658919835167));
#55642=CARTESIAN_POINT('Ctrl Pts',(110.571370896696,1.92205977074311,12.092540813239));
#55643=CARTESIAN_POINT('Ctrl Pts',(110.530599794242,1.94418497331027,12.0188377356399));
#55644=CARTESIAN_POINT('Ctrl Pts',(110.489727940626,1.96476502139403,11.94503854261));
#55645=CARTESIAN_POINT('Ctrl Pts',(110.424075796662,1.9978225942717,11.8264954667157));
#55646=CARTESIAN_POINT('Ctrl Pts',(110.357675707854,2.02713460334668,11.7068242062579));
#55647=CARTESIAN_POINT('Ctrl Pts',(110.290889857939,2.05284419609184,11.5867407952597));
#55648=CARTESIAN_POINT('Ctrl Pts',(110.257747473351,2.06560254552451,11.5271495705457));
#55649=CARTESIAN_POINT('Ctrl Pts',(110.224510090202,2.07747454356665,11.4674565629599));
#55650=CARTESIAN_POINT('Ctrl Pts',(110.191221970063,2.08848206680026,11.4077475491063));
#55651=CARTESIAN_POINT('Ctrl Pts',(109.972381969016,2.14868687233568,-12.4292823113103));
#55652=CARTESIAN_POINT('Ctrl Pts',(110.00263258259,3.45081712096779,-12.2041791958424));
#55653=CARTESIAN_POINT('Ctrl Pts',(110.032883196163,4.71829268088368,-11.7753640273909));
#55654=CARTESIAN_POINT('Ctrl Pts',(110.063133809737,5.88651486311146,-11.1581738456663));
#55655=CARTESIAN_POINT('Ctrl Pts',(110.123635036884,8.22295922756701,-9.92379348221692));
#55656=CARTESIAN_POINT('Ctrl Pts',(110.184136264031,10.1623900812701,-7.93591306567471));
#55657=CARTESIAN_POINT('Ctrl Pts',(110.244637491178,11.3263623166378,-5.56679151803852));
#55658=CARTESIAN_POINT('Ctrl Pts',(110.305138718325,12.4903345520055,-3.19766997040239));
#55659=CARTESIAN_POINT('Ctrl Pts',(110.365639945472,12.8788481690378,-0.447307291672291));
#55660=CARTESIAN_POINT('Ctrl Pts',(110.426141172618,12.428587672788,2.15575037134916));
#55661=CARTESIAN_POINT('Ctrl Pts',(110.456391786192,12.203457424663,3.45727920285992));
#55662=CARTESIAN_POINT('Ctrl Pts',(110.486642399765,11.7686336482176,4.72198178044351));
#55663=CARTESIAN_POINT('Ctrl Pts',(110.516893013339,11.1508289389973,5.89050829312984));
#55664=CARTESIAN_POINT('Ctrl Pts',(110.547143626912,10.5330242297771,7.05903480581618));
#55665=CARTESIAN_POINT('Ctrl Pts',(110.577394240486,9.73223858778215,8.13138525360525));
#55666=CARTESIAN_POINT('Ctrl Pts',(110.607644854059,8.78376077504186,9.05044254549862));
#55667=CARTESIAN_POINT('Ctrl Pts',(110.668146081206,6.88680514956126,10.8885571292854));
#55668=CARTESIAN_POINT('Ctrl Pts',(110.728647308353,4.39908084109936,12.1134990894893));
#55669=CARTESIAN_POINT('Ctrl Pts',(110.7891485355,1.78272152996964,12.4870259868466));
#55670=CARTESIAN_POINT('Ctrl Pts',(111.097169771268,-0.290214146636271,
12.6103009400526));
#55671=CARTESIAN_POINT('Ctrl Pts',(111.144815151789,-2.37096670930334,12.5624143882402));
#55672=CARTESIAN_POINT('Ctrl Pts',(111.240105912831,-6.50629452391662,11.4165924521908));
#55673=CARTESIAN_POINT('Ctrl Pts',(111.383042054393,-11.1491329074663,6.95494094815187));
#55674=CARTESIAN_POINT('Ctrl Pts',(111.525978195955,-13.1145440767032,0.824063538448764));
#55675=CARTESIAN_POINT('Ctrl Pts',(111.668914337517,-11.9318640492024,-5.5049451877202));
#55676=CARTESIAN_POINT('Ctrl Pts',(111.811850479079,-7.88447155714136,-10.5122325482705));
#55677=CARTESIAN_POINT('Ctrl Pts',(111.954786620641,-1.94430045531652,-12.9958610226402));
#55678=CARTESIAN_POINT('Ctrl Pts',(112.097722762203,4.4626861392344,-12.3594863000869));
#55679=CARTESIAN_POINT('Ctrl Pts',(112.240658903765,9.79827742810367,-8.75592671286024));
#55680=CARTESIAN_POINT('Ctrl Pts',(112.383595045327,12.7815601968128,-3.05028594329674));
#55681=CARTESIAN_POINT('Ctrl Pts',(112.526531186889,12.696311862802,3.38764795390582));
#55682=CARTESIAN_POINT('Ctrl Pts',(112.669467328451,9.56300415581823,9.01229516996203));
#55683=CARTESIAN_POINT('Ctrl Pts',(112.812403470013,4.13386177705519,12.4733191545619));
#55684=CARTESIAN_POINT('Ctrl Pts',(112.955339611575,-2.28771515821232,12.9398170902243));
#55685=CARTESIAN_POINT('Ctrl Pts',(113.098275753138,-8.16007012053368,10.2997942704675));
#55686=CARTESIAN_POINT('Ctrl Pts',(113.2412118947,-12.0733999250621,5.18705315684538));
#55687=CARTESIAN_POINT('Ctrl Pts',(113.384148036262,-13.0882138535401,-1.1709673804415));
#55688=CARTESIAN_POINT('Ctrl Pts',(113.527084177824,-10.9608808597989,-7.24786845005694));
#55689=CARTESIAN_POINT('Ctrl Pts',(113.670020319386,-6.20211945919366,-11.5847408517043));
#55690=CARTESIAN_POINT('Ctrl Pts',(113.812956460948,0.0456129136003346,
-13.1404119346645));
#55691=CARTESIAN_POINT('Ctrl Pts',(113.95589260251,6.28239478521566,-11.5414046858392));
#55692=CARTESIAN_POINT('Ctrl Pts',(114.098828744072,11.0109336279624,-7.1716000307795));
#55693=CARTESIAN_POINT('Ctrl Pts',(114.241764885634,13.0960276590931,-1.08007680700643));
#55694=CARTESIAN_POINT('Ctrl Pts',(114.384701027196,12.0370988918816,5.27074535791014));
#55695=CARTESIAN_POINT('Ctrl Pts',(114.527637168758,8.08836916076015,10.3561957628697));
#55696=CARTESIAN_POINT('Ctrl Pts',(114.67057331032,2.19782793558771,12.9553872468603));
#55697=CARTESIAN_POINT('Ctrl Pts',(114.813509451882,-4.22035581903552,12.4443201159399));
#55698=CARTESIAN_POINT('Ctrl Pts',(114.956445593445,-9.62533959369969,8.945688570367));
#55699=CARTESIAN_POINT('Ctrl Pts',(115.099381735007,-12.7195244136438,3.29942497607923));
#55700=CARTESIAN_POINT('Ctrl Pts',(115.242317876569,-12.7600752611215,-3.1389465642066));
#55701=CARTESIAN_POINT('Ctrl Pts',(115.385254018131,-9.73725696256094,-8.82373691986794));
#55702=CARTESIAN_POINT('Ctrl Pts',(115.528190159693,-4.37677111438902,-12.3901727827269));
#55703=CARTESIAN_POINT('Ctrl Pts',(115.671126301255,2.03446587665453,-12.982043464728));
#55704=CARTESIAN_POINT('Ctrl Pts',(115.814062442817,7.95727976006216,-10.4572564057129));
#55705=CARTESIAN_POINT('Ctrl Pts',(115.956998584379,11.9697526294507,-5.42194758061048));
#55706=CARTESIAN_POINT('Ctrl Pts',(116.099934725941,13.1085942544627,0.915031186620946));
#55707=CARTESIAN_POINT('Ctrl Pts',(116.242870867503,11.1003927484593,7.03233773286076));
#55708=CARTESIAN_POINT('Ctrl Pts',(116.385807009065,6.42727687176741,11.4613516302832));
#55709=CARTESIAN_POINT('Ctrl Pts',(116.528743150627,0.211119866039206,13.1388026997321));
#55710=CARTESIAN_POINT('Ctrl Pts',(116.671679292189,-6.05568826983115,11.6619279908134));
#55711=CARTESIAN_POINT('Ctrl Pts',(116.814615433752,-10.8687510776711,7.38539445257166));
#55712=CARTESIAN_POINT('Ctrl Pts',(116.957551575314,-13.0723504975697,1.33566445033233));
#55713=CARTESIAN_POINT('Ctrl Pts',(117.100487716876,-12.1379349596952,-5.03437216491156));
#55714=CARTESIAN_POINT('Ctrl Pts',(117.243423858438,-8.28879524507787,-10.1963878425912));
#55715=CARTESIAN_POINT('Ctrl Pts',(117.338714619479,-4.39706681368208,-12.0042301641757));
#55716=CARTESIAN_POINT('Ctrl Pts',(117.38636,-2.35227454062139,-12.3923653325402));
#55717=CARTESIAN_POINT('Ctrl Pts',(111.292699062434,-0.282422116923941,
12.2717239246129));
#55718=CARTESIAN_POINT('Ctrl Pts',(111.340344442955,-2.30730805151564,12.2251230903951));
#55719=CARTESIAN_POINT('Ctrl Pts',(111.435635203996,-6.33160545091578,11.1100656042329));
#55720=CARTESIAN_POINT('Ctrl Pts',(111.578571345558,-10.8497871454186,6.76820605895459));
#55721=CARTESIAN_POINT('Ctrl Pts',(111.72150748712,-12.7624285155083,0.801938057486237));
#55722=CARTESIAN_POINT('Ctrl Pts',(111.864443628682,-11.6115025496937,-5.3571415848817));
#55723=CARTESIAN_POINT('Ctrl Pts',(112.007379770244,-7.6727794761334,-10.229987077784));
#55724=CARTESIAN_POINT('Ctrl Pts',(112.150315911806,-1.89209746282579,-12.6469320114269));
#55725=CARTESIAN_POINT('Ctrl Pts',(112.293252053368,4.34286640130357,-12.0276434674896));
#55726=CARTESIAN_POINT('Ctrl Pts',(112.436188194931,9.53520111106505,-8.52083672191218));
#55727=CARTESIAN_POINT('Ctrl Pts',(112.579124336493,12.4383850002277,-2.96838807933386));
#55728=CARTESIAN_POINT('Ctrl Pts',(112.722060478055,12.355425519325,3.29669217584419));
#55729=CARTESIAN_POINT('Ctrl Pts',(112.864996619617,9.30624474768778,8.770321880394));
#55730=CARTESIAN_POINT('Ctrl Pts',(113.007932761179,4.0228707238385,12.1384199961632));
#55731=CARTESIAN_POINT('Ctrl Pts',(113.150868902741,-2.22629174142586,12.5923928160875));
#55732=CARTESIAN_POINT('Ctrl Pts',(113.293805044303,-7.9409784271377,10.0232526066075));
#55733=CARTESIAN_POINT('Ctrl Pts',(113.436741185865,-11.7492382946403,5.04778471391757));
#55734=CARTESIAN_POINT('Ctrl Pts',(113.579677327427,-12.7368052388659,-1.13952779444496));
#55735=CARTESIAN_POINT('Ctrl Pts',(113.722613468989,-10.6665895224436,-7.05326867961644));
#55736=CARTESIAN_POINT('Ctrl Pts',(113.865549610551,-6.03559725596654,-11.2736993467585));
#55737=CARTESIAN_POINT('Ctrl Pts',(114.008485752114,0.0443882414671669,
-12.7876018411039));
#55738=CARTESIAN_POINT('Ctrl Pts',(114.151421893675,6.11371725037299,-11.2315267240768));
#55739=CARTESIAN_POINT('Ctrl Pts',(114.294358035238,10.7152984117464,-6.97904800954766));
#55740=CARTESIAN_POINT('Ctrl Pts',(114.4372941768,12.7444092496665,-1.05107756396691));
#55741=CARTESIAN_POINT('Ctrl Pts',(114.580230318362,11.7139119166666,5.12922984286356));
#55742=CARTESIAN_POINT('Ctrl Pts',(114.723166459924,7.87120258374953,10.0781397617187));
#55743=CARTESIAN_POINT('Ctrl Pts',(114.866102601486,2.13881792255004,12.6075449258277));
#55744=CARTESIAN_POINT('Ctrl Pts',(115.009038743048,-4.10704246639664,12.1101995597327));
#55745=CARTESIAN_POINT('Ctrl Pts',(115.15197488461,-9.36690652634302,8.70550361747755));
#55746=CARTESIAN_POINT('Ctrl Pts',(115.294911026172,-12.3780148307832,3.21083791805588));
#55747=CARTESIAN_POINT('Ctrl Pts',(115.437847167734,-12.4174769187636,-3.05466822982062));
#55748=CARTESIAN_POINT('Ctrl Pts',(115.580783309296,-9.47581899873865,-8.58682627629518));
#55749=CARTESIAN_POINT('Ctrl Pts',(115.723719450858,-4.25925812970948,-12.0575060413461));
#55750=CARTESIAN_POINT('Ctrl Pts',(115.86665559242,1.97984201099058,-12.6334854444642));
#55751=CARTESIAN_POINT('Ctrl Pts',(116.009591733983,7.74363283403016,-10.1764870029551));
#55752=CARTESIAN_POINT('Ctrl Pts',(116.152527875545,11.6483738503004,-5.2763724005699));
#55753=CARTESIAN_POINT('Ctrl Pts',(116.295464017107,12.7566384414821,0.890463293303174));
#55754=CARTESIAN_POINT('Ctrl Pts',(116.438400158669,10.802355622712,6.84352479869885));
#55755=CARTESIAN_POINT('Ctrl Pts',(116.581336300231,6.25470936279257,11.1536230323429));
#55756=CARTESIAN_POINT('Ctrl Pts',(116.724272441793,0.205451457768569,12.7860358129088));
#55757=CARTESIAN_POINT('Ctrl Pts',(116.867208583355,-5.89309763297169,11.3488140697284));
#55758=CARTESIAN_POINT('Ctrl Pts',(117.010144724917,-10.5769333550863,7.18710221327586));
#55759=CARTESIAN_POINT('Ctrl Pts',(117.153080866479,-12.7213678019711,1.29980287293045));
#55760=CARTESIAN_POINT('Ctrl Pts',(117.296017008041,-11.8120406125427,-4.89920309081004));
#55761=CARTESIAN_POINT('Ctrl Pts',(117.438953149603,-8.06624737972471,-9.92262256288682));
#55762=CARTESIAN_POINT('Ctrl Pts',(117.534243910645,-4.27900890487063,-11.681925689369));
#55763=CARTESIAN_POINT('Ctrl Pts',(117.581889291165,-2.28911775338493,-12.05963972286));
#55764=CARTESIAN_POINT('Ctrl Pts',(111.4882283536,-0.27463008721161,11.9331469091732));
#55765=CARTESIAN_POINT('Ctrl Pts',(111.53587373412,-2.24364939372795,11.8878317925501));
#55766=CARTESIAN_POINT('Ctrl Pts',(111.631164495162,-6.15691637791494,10.8035387562751));
#55767=CARTESIAN_POINT('Ctrl Pts',(111.774100636724,-10.5504413833709,6.58147116975733));
#55768=CARTESIAN_POINT('Ctrl Pts',(111.917036778286,-12.4103129543134,0.779812576523712));
#55769=CARTESIAN_POINT('Ctrl Pts',(112.059972919848,-11.2911410501849,-5.20933798204321));
#55770=CARTESIAN_POINT('Ctrl Pts',(112.20290906141,-7.46108739512543,-9.94774160729745));
#55771=CARTESIAN_POINT('Ctrl Pts',(112.345845202972,-1.83989447033507,-12.2980030002136));
#55772=CARTESIAN_POINT('Ctrl Pts',(112.488781344534,4.22304666337274,-11.6958006348923));
#55773=CARTESIAN_POINT('Ctrl Pts',(112.631717486096,9.27212479402644,-8.28574673096412));
#55774=CARTESIAN_POINT('Ctrl Pts',(112.774653627658,12.0952098036425,-2.88649021537098));
#55775=CARTESIAN_POINT('Ctrl Pts',(112.91758976922,12.0145391758479,3.20573639778256));
#55776=CARTESIAN_POINT('Ctrl Pts',(113.060525910782,9.04948533955733,8.52834859082596));
#55777=CARTESIAN_POINT('Ctrl Pts',(113.203462052344,3.9118796706218,11.8035208377644));
#55778=CARTESIAN_POINT('Ctrl Pts',(113.346398193907,-2.1648683246394,12.2449685419508));
#55779=CARTESIAN_POINT('Ctrl Pts',(113.489334335469,-7.72188673374172,9.74671094274739));
#55780=CARTESIAN_POINT('Ctrl Pts',(113.632270477031,-11.4250766642184,4.90851627098979));
#55781=CARTESIAN_POINT('Ctrl Pts',(113.775206618593,-12.3853966241917,-1.10808820844843));
#55782=CARTESIAN_POINT('Ctrl Pts',(113.918142760155,-10.3722981850883,-6.85866890917593));
#55783=CARTESIAN_POINT('Ctrl Pts',(114.061078901717,-5.86907505273941,-10.9626578418128));
#55784=CARTESIAN_POINT('Ctrl Pts',(114.204015043279,0.0431635693339993,
-12.4347917475433));
#55785=CARTESIAN_POINT('Ctrl Pts',(114.346951184841,5.94503971553032,-10.9216487623144));
#55786=CARTESIAN_POINT('Ctrl Pts',(114.489887326403,10.4196631955305,-6.78649598831582));
#55787=CARTESIAN_POINT('Ctrl Pts',(114.632823467965,12.3927908402399,-1.02207832092739));
#55788=CARTESIAN_POINT('Ctrl Pts',(114.775759609527,11.3907249414516,4.98771432781699));
#55789=CARTESIAN_POINT('Ctrl Pts',(114.918695751089,7.65403600673891,9.80008376056765));
#55790=CARTESIAN_POINT('Ctrl Pts',(115.061631892651,2.07980790951236,12.259702604795));
#55791=CARTESIAN_POINT('Ctrl Pts',(115.204568034214,-3.99372911375776,11.7760790035254));
#55792=CARTESIAN_POINT('Ctrl Pts',(115.347504175776,-9.10847345898634,8.4653186645881));
#55793=CARTESIAN_POINT('Ctrl Pts',(115.490440317338,-12.0365052479226,3.12225086003253));
#55794=CARTESIAN_POINT('Ctrl Pts',(115.6333764589,-12.0748785764056,-2.97038989543463));
#55795=CARTESIAN_POINT('Ctrl Pts',(115.776312600462,-9.21438103491635,-8.34991563272242));
#55796=CARTESIAN_POINT('Ctrl Pts',(115.919248742024,-4.14174514502994,-11.7248392999654));
#55797=CARTESIAN_POINT('Ctrl Pts',(116.062184883586,1.92521814532663,-12.2849274242003));
#55798=CARTESIAN_POINT('Ctrl Pts',(116.205121025148,7.52998590799816,-9.89571760019732));
#55799=CARTESIAN_POINT('Ctrl Pts',(116.34805716671,11.3269950711502,-5.13079722052934));
#55800=CARTESIAN_POINT('Ctrl Pts',(116.490993308272,12.4046826285015,0.865895399985405));
#55801=CARTESIAN_POINT('Ctrl Pts',(116.633929449834,10.5043184969647,6.65471186453694));
#55802=CARTESIAN_POINT('Ctrl Pts',(116.776865591396,6.08214185381772,10.8458944344027));
#55803=CARTESIAN_POINT('Ctrl Pts',(116.919801732959,0.199783049497946,12.4332689260855));
#55804=CARTESIAN_POINT('Ctrl Pts',(117.062737874521,-5.73050699611223,11.0357001486433));
#55805=CARTESIAN_POINT('Ctrl Pts',(117.205674016083,-10.2851156325015,6.98880997398006));
#55806=CARTESIAN_POINT('Ctrl Pts',(117.348610157645,-12.3703851063725,1.26394129552858));
#55807=CARTESIAN_POINT('Ctrl Pts',(117.491546299207,-11.4861462653902,-4.76403401670852));
#55808=CARTESIAN_POINT('Ctrl Pts',(117.634482440769,-7.84369951437156,-9.64885728318242));
#55809=CARTESIAN_POINT('Ctrl Pts',(117.72977320181,-4.16095099605918,-11.3596212145623));
#55810=CARTESIAN_POINT('Ctrl Pts',(117.777418582331,-2.22596096614847,-11.7269141131798));
#55811=CARTESIAN_POINT('Ctrl Pts',(111.683757644765,-0.266838057499279,
11.5945698937334));
#55812=CARTESIAN_POINT('Ctrl Pts',(111.731403025286,-2.17999073594025,11.550540494705));
#55813=CARTESIAN_POINT('Ctrl Pts',(111.826693786327,-5.98222730491411,10.4970119083172));
#55814=CARTESIAN_POINT('Ctrl Pts',(111.969629927889,-10.2510956213232,6.39473628056006));
#55815=CARTESIAN_POINT('Ctrl Pts',(112.112566069451,-12.0581973931186,0.757687095561184));
#55816=CARTESIAN_POINT('Ctrl Pts',(112.255502211013,-10.9707795506762,-5.06153437920471));
#55817=CARTESIAN_POINT('Ctrl Pts',(112.398438352575,-7.24939531411746,-9.66549613681094));
#55818=CARTESIAN_POINT('Ctrl Pts',(112.541374494138,-1.78769147784434,-11.9490739890003));
#55819=CARTESIAN_POINT('Ctrl Pts',(112.6843106357,4.1032269254419,-11.363957802295));
#55820=CARTESIAN_POINT('Ctrl Pts',(112.827246777262,9.00904847698782,-8.05065674001605));
#55821=CARTESIAN_POINT('Ctrl Pts',(112.970182918824,11.7520346070574,-2.80459235140811));
#55822=CARTESIAN_POINT('Ctrl Pts',(113.113119060386,11.6736528323709,3.11478061972093));
#55823=CARTESIAN_POINT('Ctrl Pts',(113.256055201948,8.79272593142687,8.28637530125792));
#55824=CARTESIAN_POINT('Ctrl Pts',(113.39899134351,3.80088861740511,11.4686216793657));
#55825=CARTESIAN_POINT('Ctrl Pts',(113.541927485072,-2.10344490785294,11.897544267814));
#55826=CARTESIAN_POINT('Ctrl Pts',(113.684863626634,-7.50279504034574,9.47016927888733));
#55827=CARTESIAN_POINT('Ctrl Pts',(113.827799768196,-11.1009150337966,4.76924782806198));
#55828=CARTESIAN_POINT('Ctrl Pts',(113.970735909758,-12.0339880095176,-1.07664862245189));
#55829=CARTESIAN_POINT('Ctrl Pts',(114.11367205132,-10.078006847733,-6.66406913873543));
#55830=CARTESIAN_POINT('Ctrl Pts',(114.256608192883,-5.7025528495123,-10.6516163368671));
#55831=CARTESIAN_POINT('Ctrl Pts',(114.399544334445,0.0419388972008348,
-12.0819816539827));
#55832=CARTESIAN_POINT('Ctrl Pts',(114.542480476007,5.77636218068765,-10.6117708005521));
#55833=CARTESIAN_POINT('Ctrl Pts',(114.685416617569,10.1240279793146,-6.59394396708397));
#55834=CARTESIAN_POINT('Ctrl Pts',(114.828352759131,12.0411724308134,-0.993079077887869));
#55835=CARTESIAN_POINT('Ctrl Pts',(114.971288900693,11.0675379662367,4.84619881277042));
#55836=CARTESIAN_POINT('Ctrl Pts',(115.114225042255,7.43686942972829,9.52202775941664));
#55837=CARTESIAN_POINT('Ctrl Pts',(115.257161183817,2.02079789647468,11.9118602837624));
#55838=CARTESIAN_POINT('Ctrl Pts',(115.400097325379,-3.88041576111888,11.4419584473181));
#55839=CARTESIAN_POINT('Ctrl Pts',(115.543033466941,-8.85004039162967,8.22513371169866));
#55840=CARTESIAN_POINT('Ctrl Pts',(115.685969608503,-11.694995665062,3.03366380200918));
#55841=CARTESIAN_POINT('Ctrl Pts',(115.828905750065,-11.7322802340477,-2.88611156104865));
#55842=CARTESIAN_POINT('Ctrl Pts',(115.971841891627,-8.95294307109407,-8.11300498914965));
#55843=CARTESIAN_POINT('Ctrl Pts',(116.11477803319,-4.0242321603504,-11.3921725585846));
#55844=CARTESIAN_POINT('Ctrl Pts',(116.257714174752,1.87059427966267,-11.9363694039364));
#55845=CARTESIAN_POINT('Ctrl Pts',(116.400650316314,7.31633898196617,-9.61494819743955));
#55846=CARTESIAN_POINT('Ctrl Pts',(116.543586457876,11.005616292,-4.98522204048877));
#55847=CARTESIAN_POINT('Ctrl Pts',(116.686522599438,12.0527268155209,0.841327506667632));
#55848=CARTESIAN_POINT('Ctrl Pts',(116.829458741,10.2062813712173,6.46589893037503));
#55849=CARTESIAN_POINT('Ctrl Pts',(116.972394882562,5.9095743448429,10.5381658364625));
#55850=CARTESIAN_POINT('Ctrl Pts',(117.115331024124,0.194114641227306,12.0805020392623));
#55851=CARTESIAN_POINT('Ctrl Pts',(117.258267165686,-5.56791635925277,10.7225862275582));
#55852=CARTESIAN_POINT('Ctrl Pts',(117.401203307248,-9.99329790991669,6.79051773468426));
#55853=CARTESIAN_POINT('Ctrl Pts',(117.54413944881,-12.0194024107739,1.2280797181267));
#55854=CARTESIAN_POINT('Ctrl Pts',(117.687075590372,-11.1602519182376,-4.628864942607));
#55855=CARTESIAN_POINT('Ctrl Pts',(117.830011731934,-7.6211516490184,-9.375092003478));
#55856=CARTESIAN_POINT('Ctrl Pts',(117.925302492976,-4.04289308724772,-11.0373167397556));
#55857=CARTESIAN_POINT('Ctrl Pts',(117.972947873497,-2.16280417891201,-11.3941885034995));
#55858=CARTESIAN_POINT('',(115.665029240284,1.6893531453192,-12.5));
#55859=CARTESIAN_POINT('',(115.587450486329,-1.68935314531919,-12.5));
#55860=CARTESIAN_POINT('Ctrl Pts',(115.665029240284,1.68957794637807,-12.5009920189267));
#55861=CARTESIAN_POINT('Ctrl Pts',(115.665531145448,1.68039383998756,-12.5009881210131));
#55862=CARTESIAN_POINT('Ctrl Pts',(115.666027316753,1.67120940348572,-12.5009840718973));
#55863=CARTESIAN_POINT('Ctrl Pts',(115.666517749822,1.66202462200871,-12.5009798762235));
#55864=CARTESIAN_POINT('Ctrl Pts',(115.679790027354,1.41346273549435,-12.5008663313784));
#55865=CARTESIAN_POINT('Ctrl Pts',(115.688841785677,1.16498141737867,-12.5006475672998));
#55866=CARTESIAN_POINT('Ctrl Pts',(115.693621337552,0.91627655910125,-12.5004053081459));
#55867=CARTESIAN_POINT('Ctrl Pts',(115.695698464643,0.808192870062367,-12.5003000256707));
#55868=CARTESIAN_POINT('Ctrl Pts',(115.69696872091,0.700066299056772,-12.5001901057846));
#55869=CARTESIAN_POINT('Ctrl Pts',(115.697427863959,0.591869115320174,-12.5000810369122));
#55870=CARTESIAN_POINT('Ctrl Pts',(115.698180844966,0.414428937293237,-12.4999021671905));
#55871=CARTESIAN_POINT('Ctrl Pts',(115.696751289823,0.237059544937474,-12.4997260835975));
#55872=CARTESIAN_POINT('Ctrl Pts',(115.693139682215,0.059641091855054,-12.499571625275));
#55873=CARTESIAN_POINT('Ctrl Pts',(115.692870383431,0.0464119211050218,
-12.4995601081217));
#55874=CARTESIAN_POINT('Ctrl Pts',(115.692588963242,0.0331829986088157,
-12.4995487085824));
#55875=CARTESIAN_POINT('Ctrl Pts',(115.692295424718,0.0199542748338118,
-12.4995374329471));
#55876=CARTESIAN_POINT('Ctrl Pts',(115.692214772672,0.0163195776711995,
-12.4995343348766));
#55877=CARTESIAN_POINT('Ctrl Pts',(115.692133205866,0.0126848989764344,
-12.4995312461615));
#55878=CARTESIAN_POINT('Ctrl Pts',(115.692050724368,0.00905023766942509,
-12.4995281669295));
#55879=CARTESIAN_POINT('Ctrl Pts',(115.692002271107,0.0069150776746254,
-12.4995263580531));
#55880=CARTESIAN_POINT('Ctrl Pts',(115.691953502204,0.00477992410763924,
-12.4995245524496));
#55881=CARTESIAN_POINT('Ctrl Pts',(115.691904417675,0.00264477680910505,
-12.4995227501446));
#55882=CARTESIAN_POINT('Ctrl Pts',(115.691862039437,0.000801349139794612,
-12.4995211940839));
#55883=CARTESIAN_POINT('Ctrl Pts',(115.691819425932,-0.0010420736832491,
-12.4995196404822));
#55884=CARTESIAN_POINT('Ctrl Pts',(115.691776577169,-0.0028854917766748,
-12.4995180893558));
#55885=CARTESIAN_POINT('Ctrl Pts',(115.691724393489,-0.00513051196352565,
-12.4995162003052));
#55886=CARTESIAN_POINT('Ctrl Pts',(115.691671860888,-0.00737552484080946,
-12.4995143149263));
#55887=CARTESIAN_POINT('Ctrl Pts',(115.691618979382,-0.00962053064940818,
-12.4995124332486));
#55888=CARTESIAN_POINT('Ctrl Pts',(115.691519210876,-0.0138560543912522,
-12.4995088831952));
#55889=CARTESIAN_POINT('Ctrl Pts',(115.691418200514,-0.0180915511691172,
-12.4995053463176));
#55890=CARTESIAN_POINT('Ctrl Pts',(115.691315948412,-0.0223270226677909,
-12.4995018228123));
#55891=CARTESIAN_POINT('Ctrl Pts',(115.690733516431,-0.0464524345272299,
-12.4994817527879));
#55892=CARTESIAN_POINT('Ctrl Pts',(115.690110802628,-0.070576768109223,
-12.4994621170303));
#55893=CARTESIAN_POINT('Ctrl Pts',(115.689447831599,-0.0947003228280837,
-12.4994429504498));
#55894=CARTESIAN_POINT('Ctrl Pts',(115.688600178345,-0.125543917413364,
-12.4994184446818));
#55895=CARTESIAN_POINT('Ctrl Pts',(115.687686737434,-0.156385429448937,
-12.4993947067422));
#55896=CARTESIAN_POINT('Ctrl Pts',(115.686707570708,-0.187225482320612,
-12.4993718038707));
#55897=CARTESIAN_POINT('Ctrl Pts',(115.681885774495,-0.339093847577508,
-12.4992590212612));
#55898=CARTESIAN_POINT('Ctrl Pts',(115.675472190412,-0.490862634991197,
-12.499166833351));
#55899=CARTESIAN_POINT('Ctrl Pts',(115.667478315592,-0.642604728235641,
-12.4991009813609));
#55900=CARTESIAN_POINT('Ctrl Pts',(115.654842096987,-0.882469162560806,
-12.4989968866432));
#55901=CARTESIAN_POINT('Ctrl Pts',(115.638278723029,-1.12185056467011,-12.4989605577552));
#55902=CARTESIAN_POINT('Ctrl Pts',(115.617876640176,-1.36101788355078,-12.4989937660998));
#55903=CARTESIAN_POINT('Ctrl Pts',(115.608536321962,-1.47051155050242,-12.4990089692783));
#55904=CARTESIAN_POINT('Ctrl Pts',(115.598391441759,-1.5799596952695,-12.4990384938089));
#55905=CARTESIAN_POINT('Ctrl Pts',(115.587450486329,-1.68938454186076,-12.4990815932618));
#55906=CARTESIAN_POINT('',(117.38636,-2.35227454062139,-12.3923653325402));
#55907=CARTESIAN_POINT('Ctrl Pts',(117.38636,-2.35227454062139,-12.3923653325402));
#55908=CARTESIAN_POINT('Ctrl Pts',(117.338714619479,-4.39706681368208,-12.0042301641757));
#55909=CARTESIAN_POINT('Ctrl Pts',(117.291069238959,-6.34293102937998,-11.1003090033835));
#55910=CARTESIAN_POINT('Ctrl Pts',(117.243423858438,-7.95738642299848,-9.78801247670741));
#55911=CARTESIAN_POINT('Ctrl Pts',(117.195778477917,-9.57184181661693,-8.47571595003138));
#55912=CARTESIAN_POINT('Ctrl Pts',(117.148133097396,-10.854888388156,-6.75504405747155));
#55913=CARTESIAN_POINT('Ctrl Pts',(117.100487716876,-11.6521475969046,-4.83303534198435));
#55914=CARTESIAN_POINT('Ctrl Pts',(117.052842336355,-12.4494068056533,-2.91102662649703));
#55915=CARTESIAN_POINT('Ctrl Pts',(117.005196955834,-12.7608786516115,-0.78768108808232));
#55916=CARTESIAN_POINT('Ctrl Pts',(116.957551575314,-12.5493480046075,1.28228001483163));
#55917=CARTESIAN_POINT('Ctrl Pts',(116.909906194793,-12.3378173576035,3.35224111774546));
#55918=CARTESIAN_POINT('Ctrl Pts',(116.862260814272,-11.6032842176373,5.36881778515853));
#55919=CARTESIAN_POINT('Ctrl Pts',(116.814615433752,-10.4338405130142,7.08986170857202));
#55920=CARTESIAN_POINT('Ctrl Pts',(116.766970053231,-9.26439680839113,8.81090563198556));
#55921=CARTESIAN_POINT('Ctrl Pts',(116.71932467271,-7.66004253911114,10.2364168113995));
#55922=CARTESIAN_POINT('Ctrl Pts',(116.671679292189,-5.81339738182608,11.1953181859262));
#55923=CARTESIAN_POINT('Ctrl Pts',(116.624033911669,-3.96675222454101,12.154219560453));
#55924=CARTESIAN_POINT('Ctrl Pts',(116.576388531148,-1.87781617925087,12.6465111300925));
#55925=CARTESIAN_POINT('Ctrl Pts',(116.528743150627,0.202678011015574,12.6130817366708));
#55926=CARTESIAN_POINT('Ctrl Pts',(116.481097770107,2.28317220128196,12.5796523432491));
#55927=CARTESIAN_POINT('Ctrl Pts',(116.433452389586,4.35522453652466,12.0205019867661));
#55928=CARTESIAN_POINT('Ctrl Pts',(116.385807009065,6.17010335026131,11.0027578256209));
#55929=CARTESIAN_POINT('Ctrl Pts',(116.338161628545,7.98498216399802,9.98501366447572));
#55930=CARTESIAN_POINT('Ctrl Pts',(116.290516248024,9.54268745622868,8.50867569866824));
#55931=CARTESIAN_POINT('Ctrl Pts',(116.242870867503,10.6562403533446,6.75095562472453));
#55932=CARTESIAN_POINT('Ctrl Pts',(116.195225486983,11.7697932504605,4.99323555078082));
#55933=CARTESIAN_POINT('Ctrl Pts',(116.147580106462,12.4391937524616,2.95413336870088));
#55934=CARTESIAN_POINT('Ctrl Pts',(116.099934725941,12.5840870659602,0.878419149789012));
#55935=CARTESIAN_POINT('Ctrl Pts',(116.05228934542,12.7289803794587,-1.19729506912286));
#55936=CARTESIAN_POINT('Ctrl Pts',(116.0046439649,12.3493665044547,-3.30962132486667));
#55937=CARTESIAN_POINT('Ctrl Pts',(115.956998584379,11.4908140887213,-5.20500259025563));
#55938=CARTESIAN_POINT('Ctrl Pts',(115.909353203858,10.6322616729878,-7.1003838556446));
#55939=CARTESIAN_POINT('Ctrl Pts',(115.861707823338,9.294770716525,-8.77882013067873));
#55940=CARTESIAN_POINT('Ctrl Pts',(115.814062442817,7.63888959105897,-10.038836111365));
#55941=CARTESIAN_POINT('Ctrl Pts',(115.766417062296,5.98300846559295,-11.2988520920513));
#55942=CARTESIAN_POINT('Ctrl Pts',(115.718771681776,4.00873717112374,-12.1404477783896));
#55943=CARTESIAN_POINT('Ctrl Pts',(115.671126301255,1.95306202538188,-12.462600507892));
#55944=CARTESIAN_POINT('Ctrl Pts',(115.669093947598,1.86537547835027,-12.476342202695));
#55945=CARTESIAN_POINT('Ctrl Pts',(115.667061593941,1.77754081533774,-12.4891387603591));
#55946=CARTESIAN_POINT('Ctrl Pts',(115.665029240284,1.68957794637772,-12.5009920189268));
#55947=CARTESIAN_POINT('Ctrl Pts',(117.38636,-9.24570028839869,7.00280438584343));
#55948=CARTESIAN_POINT('Ctrl Pts',(117.38636,-9.37284071329502,6.84941999305855));
#55949=CARTESIAN_POINT('Ctrl Pts',(117.38636,-9.49588388830964,6.69285254633599));
#55950=CARTESIAN_POINT('Ctrl Pts',(117.38636,-9.61468485491513,6.53324017247767));
#55951=CARTESIAN_POINT('Ctrl Pts',(117.38636,-9.78004470797177,6.31107465109028));
#55952=CARTESIAN_POINT('Ctrl Pts',(117.38636,-9.9371875313824,6.08301130262427));
#55953=CARTESIAN_POINT('Ctrl Pts',(117.38636,-10.0859821306484,5.84958579014008));
#55954=CARTESIAN_POINT('Ctrl Pts',(117.38636,-10.2358733994428,5.61443984796328));
#55955=CARTESIAN_POINT('Ctrl Pts',(117.38636,-10.3772932439531,5.37385189057232));
#55956=CARTESIAN_POINT('Ctrl Pts',(117.38636,-10.5100664873751,5.12833571523603));
#55957=CARTESIAN_POINT('Ctrl Pts',(117.38636,-10.5658598569975,5.02516602256461));
#55958=CARTESIAN_POINT('Ctrl Pts',(117.38636,-10.620125878563,4.92112573792297));
#55959=CARTESIAN_POINT('Ctrl Pts',(117.38636,-10.6728492069859,4.81625156664499));
#55960=CARTESIAN_POINT('Ctrl Pts',(117.38636,-10.6937228617391,4.77473090948504));
#55961=CARTESIAN_POINT('Ctrl Pts',(117.38636,-10.7143546925228,4.73307953733116));
#55962=CARTESIAN_POINT('Ctrl Pts',(117.38636,-10.7347436840285,4.69129969754066));
#55963=CARTESIAN_POINT('Ctrl Pts',(117.38636,-10.7509151596584,4.65816212617968));
#55964=CARTESIAN_POINT('Ctrl Pts',(117.38636,-10.7669324216288,4.62494663051733));
#55965=CARTESIAN_POINT('Ctrl Pts',(117.38636,-10.7827907480625,4.59166356955379));
#55966=CARTESIAN_POINT('Ctrl Pts',(117.38636,-10.9034104334192,4.33850997494812));
#55967=CARTESIAN_POINT('Ctrl Pts',(117.38636,-11.014913595354,4.08129723752002));
#55968=CARTESIAN_POINT('Ctrl Pts',(117.38636,-11.1171584437568,3.8205625901497));
#55969=CARTESIAN_POINT('Ctrl Pts',(117.38636,-11.2200231885224,3.55824714470407));
#55970=CARTESIAN_POINT('Ctrl Pts',(117.38636,-11.313517322248,3.2923664039607));
#55971=CARTESIAN_POINT('Ctrl Pts',(117.38636,-11.3974521500579,3.02343941709135));
#55972=CARTESIAN_POINT('Ctrl Pts',(117.38636,-11.4811108269362,2.75539721714456));
#55973=CARTESIAN_POINT('Ctrl Pts',(117.38636,-11.5552732415844,2.48432819553525));
#55974=CARTESIAN_POINT('Ctrl Pts',(117.38636,-11.6197046335814,2.21072714127617));
#55975=CARTESIAN_POINT('Ctrl Pts',(117.38636,-11.6316456897028,2.16002071630966));
#55976=CARTESIAN_POINT('Ctrl Pts',(117.38636,-11.6432523742739,2.10922728434781));
#55977=CARTESIAN_POINT('Ctrl Pts',(117.38636,-11.654523000657,2.05834994746899));
#55978=CARTESIAN_POINT('Ctrl Pts',(117.38636,-11.6617905024604,2.02554332919));
#55979=CARTESIAN_POINT('Ctrl Pts',(117.38636,-11.6689182842477,1.99270157512914));
#55980=CARTESIAN_POINT('Ctrl Pts',(117.38636,-11.6759028644632,1.95984029488391));
#55981=CARTESIAN_POINT('Ctrl Pts',(117.38636,-11.7290005457511,1.71002459639411));
#55982=CARTESIAN_POINT('Ctrl Pts',(117.38636,-11.7738715396368,1.45887320689027));
#55983=CARTESIAN_POINT('Ctrl Pts',(117.38636,-11.8104156759069,1.20677663752006));
#55984=CARTESIAN_POINT('Ctrl Pts',(117.38636,-11.8505820658636,0.929692263785574));
#55985=CARTESIAN_POINT('Ctrl Pts',(117.38636,-11.8806903110308,0.651465919625066));
#55986=CARTESIAN_POINT('Ctrl Pts',(117.38636,-11.9009063549852,0.372629730453109));
#55987=CARTESIAN_POINT('Ctrl Pts',(117.38636,-11.9213338464699,0.0908770842498219));
#55988=CARTESIAN_POINT('Ctrl Pts',(117.38636,-11.931661168529,-0.191498807233445));
#55989=CARTESIAN_POINT('Ctrl Pts',(117.38636,-11.9320077592467,-0.473963199932295));
#55990=CARTESIAN_POINT('Ctrl Pts',(117.38636,-11.932355959454,-0.75773929399841));
#55991=CARTESIAN_POINT('Ctrl Pts',(117.38636,-11.9226305225265,-1.04160533140647));
#55992=CARTESIAN_POINT('Ctrl Pts',(117.38636,-11.9029002560441,-1.32502434709932));
#55993=CARTESIAN_POINT('Ctrl Pts',(117.38636,-11.8832211539417,-1.60770840271309));
#55994=CARTESIAN_POINT('Ctrl Pts',(117.38636,-11.8535889969035,-1.889948378621));
#55995=CARTESIAN_POINT('Ctrl Pts',(117.38636,-11.8140205502011,-2.17120735959316));
#55996=CARTESIAN_POINT('Ctrl Pts',(117.38636,-11.7991823826877,-2.27667947745771));
#55997=CARTESIAN_POINT('Ctrl Pts',(117.38636,-11.7829464081973,-2.38201355312953));
#55998=CARTESIAN_POINT('Ctrl Pts',(117.38636,-11.7653116551779,-2.48718084494898));
#55999=CARTESIAN_POINT('Ctrl Pts',(117.38636,-11.7600470974409,-2.51857676408778));
#56000=CARTESIAN_POINT('Ctrl Pts',(117.38636,-11.7546578709007,-2.54995781703081));
#56001=CARTESIAN_POINT('Ctrl Pts',(117.38636,-11.7491439322613,-2.58132323346777));
#56002=CARTESIAN_POINT('Ctrl Pts',(117.38636,-11.7438282333261,-2.61156098576466));
#56003=CARTESIAN_POINT('Ctrl Pts',(117.38636,-11.7383980260217,-2.64177618345329));
#56004=CARTESIAN_POINT('Ctrl Pts',(117.38636,-11.7328543766207,-2.67196331422791));
#56005=CARTESIAN_POINT('Ctrl Pts',(117.38636,-11.6810079485269,-2.95428544390265));
#56006=CARTESIAN_POINT('Ctrl Pts',(117.38636,-11.6192195647412,-3.23428733063864));
#56007=CARTESIAN_POINT('Ctrl Pts',(117.38636,-11.5476371290337,-3.51142874506684));
#56008=CARTESIAN_POINT('Ctrl Pts',(117.38636,-11.4756696433579,-3.7900609343167));
#56009=CARTESIAN_POINT('Ctrl Pts',(117.38636,-11.3938024458907,-4.06580242731433));
#56010=CARTESIAN_POINT('Ctrl Pts',(117.38636,-11.3021334566762,-4.33810671920979));
#56011=CARTESIAN_POINT('Ctrl Pts',(117.38636,-11.2677183953176,-4.44033724443006));
#56012=CARTESIAN_POINT('Ctrl Pts',(117.38636,-11.2319212866881,-4.54208328651749));
#56013=CARTESIAN_POINT('Ctrl Pts',(117.38636,-11.1947454245643,-4.64331573484444));
#56014=CARTESIAN_POINT('Ctrl Pts',(117.38636,-11.0961898713248,-4.91168933482804));
#56015=CARTESIAN_POINT('Ctrl Pts',(117.38636,-10.9879479086506,-5.17645443756622));
#56016=CARTESIAN_POINT('Ctrl Pts',(117.38636,-10.8703739909169,-5.43719361311492));
#56017=CARTESIAN_POINT('Ctrl Pts',(117.38636,-10.7523359767629,-5.69896199752504));
#56018=CARTESIAN_POINT('Ctrl Pts',(117.38636,-10.6248919031944,-5.95667315088571));
#56019=CARTESIAN_POINT('Ctrl Pts',(117.38636,-10.488351543623,-6.20988512596418));
#56020=CARTESIAN_POINT('Ctrl Pts',(117.38636,-10.402408064239,-6.369265972977));
#56021=CARTESIAN_POINT('Ctrl Pts',(117.38636,-10.3128597651542,-6.52686387259263));
#56022=CARTESIAN_POINT('Ctrl Pts',(117.38636,-10.2197748068755,-6.68256318039236));
#56023=CARTESIAN_POINT('Ctrl Pts',(117.38636,-10.1765977533944,-6.75478362786477));
#56024=CARTESIAN_POINT('Ctrl Pts',(117.38636,-10.1326596830689,-6.82659552196018));
#56025=CARTESIAN_POINT('Ctrl Pts',(117.38636,-10.0879669200322,-6.8979869548852));
#56026=CARTESIAN_POINT('Ctrl Pts',(117.38636,-10.0639646559907,-6.93632774894085));
#56027=CARTESIAN_POINT('Ctrl Pts',(117.38636,-10.0397410183703,-6.97455292077738));
#56028=CARTESIAN_POINT('Ctrl Pts',(117.38636,-10.0153169542022,-7.01262974883411));
#56029=CARTESIAN_POINT('Ctrl Pts',(117.38636,-9.85868284503341,-7.25682047817356));
#56030=CARTESIAN_POINT('Ctrl Pts',(117.38636,-9.69369422294742,-7.49510168726722));
#56031=CARTESIAN_POINT('Ctrl Pts',(117.38636,-9.52075996409615,-7.72707136358586));
#56032=CARTESIAN_POINT('Ctrl Pts',(117.38636,-9.346793083249,-7.96042617314377));
#56033=CARTESIAN_POINT('Ctrl Pts',(117.38636,-9.16478509439432,-8.18739439224378));
#56034=CARTESIAN_POINT('Ctrl Pts',(117.38636,-8.97510211448885,-8.40754900414395));
#56035=CARTESIAN_POINT('Ctrl Pts',(117.38636,-8.78560397283429,-8.62748908444294));
#56036=CARTESIAN_POINT('Ctrl Pts',(117.38636,-8.58844544212308,-8.84062935769821));
#56037=CARTESIAN_POINT('Ctrl Pts',(117.38636,-8.38394663465303,-9.04651838120069));
#56038=CARTESIAN_POINT('Ctrl Pts',(117.38636,-8.19583745966281,-9.23590635284578));
#56039=CARTESIAN_POINT('Ctrl Pts',(117.38636,-8.00151675320351,-9.41915884654599));
#56040=CARTESIAN_POINT('Ctrl Pts',(117.38636,-7.80120380491192,-9.59589947210861));
#56041=CARTESIAN_POINT('Ctrl Pts',(117.38636,-7.60816020747953,-9.76622618569375));
#56042=CARTESIAN_POINT('Ctrl Pts',(117.38636,-7.40955096338507,-9.93050511826213));
#56043=CARTESIAN_POINT('Ctrl Pts',(117.38636,-7.20570423293078,-10.0885700721869));
#56044=CARTESIAN_POINT('Ctrl Pts',(117.38636,-7.11652128835703,-10.157723489529));
#56045=CARTESIAN_POINT('Ctrl Pts',(117.38636,-7.02633560821988,-10.2256871780914));
#56046=CARTESIAN_POINT('Ctrl Pts',(117.38636,-6.93517361060053,-10.2924456014955));
#56047=CARTESIAN_POINT('Ctrl Pts',(117.38636,-6.89807959236754,-10.3196097514662));
#56048=CARTESIAN_POINT('Ctrl Pts',(117.38636,-6.86082391907642,-10.346574334626));
#56049=CARTESIAN_POINT('Ctrl Pts',(117.38636,-6.82340834383462,-10.3733382551376));
#56050=CARTESIAN_POINT('Ctrl Pts',(117.38636,-6.7881148669079,-10.3985842069889));
#56051=CARTESIAN_POINT('Ctrl Pts',(117.38636,-6.7526742587066,-10.4236549403665));
#56052=CARTESIAN_POINT('Ctrl Pts',(117.38636,-6.7171154240662,-10.4485305135992));
#56053=CARTESIAN_POINT('Ctrl Pts',(117.38636,-6.47938551746104,-10.6148370801999));
#56054=CARTESIAN_POINT('Ctrl Pts',(117.38636,-6.2361868719198,-10.7725611084642));
#56055=CARTESIAN_POINT('Ctrl Pts',(117.38636,-5.98806594605025,-10.9215634745735));
#56056=CARTESIAN_POINT('Ctrl Pts',(117.38636,-5.73703327091479,-11.0723144135959));
#56057=CARTESIAN_POINT('Ctrl Pts',(117.38636,-5.48096165954196,-11.2141381368804));
#56058=CARTESIAN_POINT('Ctrl Pts',(117.38636,-5.22037762132249,-11.3468546933849));
#56059=CARTESIAN_POINT('Ctrl Pts',(117.38636,-4.95798157512453,-11.4804941132424));
#56060=CARTESIAN_POINT('Ctrl Pts',(117.38636,-4.69100962319276,-11.6048996158117));
#56061=CARTESIAN_POINT('Ctrl Pts',(117.38636,-4.41996688550316,-11.7198460929511));
#56062=CARTESIAN_POINT('Ctrl Pts',(117.38636,-4.14963820346103,-11.8344897463297));
#56063=CARTESIAN_POINT('Ctrl Pts',(117.38636,-3.87525960444849,-11.9397244361644));
#56064=CARTESIAN_POINT('Ctrl Pts',(117.38636,-3.59730806781764,-12.0352811531028));
#56065=CARTESIAN_POINT('Ctrl Pts',(117.38636,-3.32284233014359,-12.1296394902508));
#56066=CARTESIAN_POINT('Ctrl Pts',(117.38636,-3.0448921588925,-12.2145612801996));
#56067=CARTESIAN_POINT('Ctrl Pts',(117.38636,-2.76390145338711,-12.2897393778152));
#56068=CARTESIAN_POINT('Ctrl Pts',(117.38636,-2.62739354564631,-12.3262615994132));
#56069=CARTESIAN_POINT('Ctrl Pts',(117.38636,-2.49016785801523,-12.3604834582857));
#56070=CARTESIAN_POINT('Ctrl Pts',(117.38636,-2.35227454062139,-12.3923653325402));
#56071=CARTESIAN_POINT('',(111.683757644765,-0.266838057499402,11.5945698937334));
#56072=CARTESIAN_POINT('Ctrl Pts',(111.683757644765,-0.266838057499279,
11.5945698937334));
#56073=CARTESIAN_POINT('Ctrl Pts',(111.731403025286,-2.17999073594025,11.550540494705));
#56074=CARTESIAN_POINT('Ctrl Pts',(111.826693786327,-5.98222730491411,10.4970119083172));
#56075=CARTESIAN_POINT('Ctrl Pts',(111.969629927889,-10.2510956213232,6.39473628056006));
#56076=CARTESIAN_POINT('Ctrl Pts',(112.070960292334,-11.5321871571861,2.39851641577062));
#56077=CARTESIAN_POINT('Ctrl Pts',(112.124645276257,-11.5984351167873,0.242765543188727));
#56078=CARTESIAN_POINT('Ctrl Pts',(112.13068487966,-11.5982247539793,0.000228379848985077));
#56079=CARTESIAN_POINT('',(111.124564900463,-1.48350560638763,12.5260977628875));
#56080=CARTESIAN_POINT('Ctrl Pts',(111.124564900463,-1.48350560638763,12.5260977628875));
#56081=CARTESIAN_POINT('Ctrl Pts',(111.125186002198,-1.48282544712551,12.5250728625007));
#56082=CARTESIAN_POINT('Ctrl Pts',(111.125806921632,-1.48214462968221,12.5240482877431));
#56083=CARTESIAN_POINT('Ctrl Pts',(111.227713712044,-1.37026603047416,12.3558966615763));
#56084=CARTESIAN_POINT('Ctrl Pts',(111.325614137126,-1.23992587748691,12.195106414339));
#56085=CARTESIAN_POINT('Ctrl Pts',(111.462555136982,-0.999462399074982,
11.9695764102533));
#56086=CARTESIAN_POINT('Ctrl Pts',(111.509793721761,-0.901990255586121,
11.89160363544));
#56087=CARTESIAN_POINT('Ctrl Pts',(111.612711002011,-0.636927615232599,
11.7200941523355));
#56088=CARTESIAN_POINT('Ctrl Pts',(111.660213206423,-0.459521768746652,
11.6391913870854));
#56089=CARTESIAN_POINT('Ctrl Pts',(111.683757644765,-0.266838057499457,
11.5945698937334));
#56090=CARTESIAN_POINT('',(111.958879057757,-1.68935314531936,-12.5));
#56091=CARTESIAN_POINT('Ctrl Pts',(111.958879057757,-1.68955541748203,-12.5010268514762));
#56092=CARTESIAN_POINT('Ctrl Pts',(111.957514912052,-1.74859600312425,-12.4930639346948));
#56093=CARTESIAN_POINT('Ctrl Pts',(111.956150766346,-1.80757882738274,-12.4846753467372));
#56094=CARTESIAN_POINT('Ctrl Pts',(111.954786620641,-1.86649787319551,-12.4758604898197));
#56095=CARTESIAN_POINT('Ctrl Pts',(111.90714124012,-3.92435748925813,-12.167984864517));
#56096=CARTESIAN_POINT('Ctrl Pts',(111.859495859599,-5.90441452319975,-11.3401087063937));
#56097=CARTESIAN_POINT('Ctrl Pts',(111.811850479079,-7.56900845551407,-10.091622733907));
#56098=CARTESIAN_POINT('Ctrl Pts',(111.764205098558,-9.23360238782844,-8.84313676142033));
#56099=CARTESIAN_POINT('Ctrl Pts',(111.716559718037,-10.5827332185155,-7.17404097457016));
#56100=CARTESIAN_POINT('Ctrl Pts',(111.668914337517,-11.4544119717758,-5.2846582934502));
#56101=CARTESIAN_POINT('Ctrl Pts',(111.621268956996,-12.326090725036,-3.3952756123304));
#56102=CARTESIAN_POINT('Ctrl Pts',(111.573623576475,-12.7203174008696,-1.28560603694085));
#56103=CARTESIAN_POINT('Ctrl Pts',(111.525978195955,-12.5898622105802,0.791041652371061));
#56104=CARTESIAN_POINT('Ctrl Pts',(111.478332815434,-12.4594070202909,2.86768934168309));
#56105=CARTESIAN_POINT('Ctrl Pts',(111.430687434913,-11.8042699638786,4.91131514491748));
#56106=CARTESIAN_POINT('Ctrl Pts',(111.383042054393,-10.7028950384141,6.67673663054116));
#56107=CARTESIAN_POINT('Ctrl Pts',(111.335396673872,-9.60152011294972,8.44215811616485));
#56108=CARTESIAN_POINT('Ctrl Pts',(111.287751293351,-8.05390731843317,9.92937528417784));
#56109=CARTESIAN_POINT('Ctrl Pts',(111.240105912831,-6.24626896752157,10.9594393521967));
#56110=CARTESIAN_POINT('Ctrl Pts',(111.201592242041,-4.78508243501816,11.792081425234));
#56111=CARTESIAN_POINT('Ctrl Pts',(111.163078571252,-3.15399164476227,12.326013405269));
#56112=CARTESIAN_POINT('Ctrl Pts',(111.124564900463,-1.48342384617797,12.525386988334));
#56113=CARTESIAN_POINT('',(112.036457811713,1.68935314531921,-12.5));
#56114=CARTESIAN_POINT('Ctrl Pts',(112.036457811713,1.68935476636984,-12.4990499102299));
#56115=CARTESIAN_POINT('Ctrl Pts',(112.036959716875,1.68016666683514,-12.4990469281187));
#56116=CARTESIAN_POINT('Ctrl Pts',(112.037455888181,1.67097827090242,-12.4990440417202));
#56117=CARTESIAN_POINT('Ctrl Pts',(112.03794632125,1.66178956373823,-12.4990412518299));
#56118=CARTESIAN_POINT('Ctrl Pts',(112.051134336919,1.41470016127385,-12.4989662301422));
#56119=CARTESIAN_POINT('Ctrl Pts',(112.060155252986,1.16771479025901,-12.4989633235238));
#56120=CARTESIAN_POINT('Ctrl Pts',(112.064958360416,0.920535224591733,-12.4990345406596));
#56121=CARTESIAN_POINT('Ctrl Pts',(112.067089749543,0.810848767133786,-12.4990661434149));
#56122=CARTESIAN_POINT('Ctrl Pts',(112.068390584884,0.701123401188886,-12.4991120949476));
#56123=CARTESIAN_POINT('Ctrl Pts',(112.068856435388,0.591330175829491,-12.499171086687));
#56124=CARTESIAN_POINT('Ctrl Pts',(112.069609416395,0.41386506032584,-12.4992664384341));
#56125=CARTESIAN_POINT('Ctrl Pts',(112.068179861252,0.236483378848915,-12.4993959394646));
#56126=CARTESIAN_POINT('Ctrl Pts',(112.064568253644,0.0590651986240468,
-12.4995480142417));
#56127=CARTESIAN_POINT('Ctrl Pts',(112.06429895486,0.0458360482258664,-12.4995593536664));
#56128=CARTESIAN_POINT('Ctrl Pts',(112.064017534671,0.0326072159344261,
-12.4995708149892));
#56129=CARTESIAN_POINT('Ctrl Pts',(112.063723996146,0.0193786521511954,
-12.4995823918539));
#56130=CARTESIAN_POINT('Ctrl Pts',(112.0636433441,0.0157439989356551,-12.4995855726896));
#56131=CARTESIAN_POINT('Ctrl Pts',(112.063561777294,0.0121093694575251,
-12.4995887622436));
#56132=CARTESIAN_POINT('Ctrl Pts',(112.063479295797,0.00847476268296781,
-12.4995919603811));
#56133=CARTESIAN_POINT('Ctrl Pts',(112.063430842536,0.00633963470445853,
-12.4995938391078));
#56134=CARTESIAN_POINT('Ctrl Pts',(112.063382073633,0.00420451497177115,
-12.4995957207963));
#56135=CARTESIAN_POINT('Ctrl Pts',(112.063332989103,0.00206940332587123,
-12.4995976054189));
#56136=CARTESIAN_POINT('Ctrl Pts',(112.063290610866,0.000226006437914865,
-12.4995992325505));
#56137=CARTESIAN_POINT('Ctrl Pts',(112.06324799736,-0.00161738424863261,
-12.499600861869));
#56138=CARTESIAN_POINT('Ctrl Pts',(112.063205148597,-0.00346076885055268,
-12.4996024933568));
#56139=CARTESIAN_POINT('Ctrl Pts',(112.063152964918,-0.00570574826303019,
-12.4996044802761));
#56140=CARTESIAN_POINT('Ctrl Pts',(112.063100432316,-0.00795071835605086,
-12.4996064704126));
#56141=CARTESIAN_POINT('Ctrl Pts',(112.06304755081,-0.0101956793305864,
-12.4996084637338));
#56142=CARTESIAN_POINT('Ctrl Pts',(112.062947782304,-0.0144311185522634,
-12.4996122244186));
#56143=CARTESIAN_POINT('Ctrl Pts',(112.062846771942,-0.0186665236572616,
-12.4996159964381));
#56144=CARTESIAN_POINT('Ctrl Pts',(112.062744519841,-0.0229018962879318,
-12.4996197795738));
#56145=CARTESIAN_POINT('Ctrl Pts',(112.06216208786,-0.0470267451542903,
-12.4996413284631));
#56146=CARTESIAN_POINT('Ctrl Pts',(112.061539374057,-0.0711502837398535,
-12.4996632379714));
#56147=CARTESIAN_POINT('Ctrl Pts',(112.060876403028,-0.095272811780564,
-12.49968546635));
#56148=CARTESIAN_POINT('Ctrl Pts',(112.060028749769,-0.126115093862099,
-12.499713886834));
#56149=CARTESIAN_POINT('Ctrl Pts',(112.059115308853,-0.156954914672159,
-12.4997428280354));
#56150=CARTESIAN_POINT('Ctrl Pts',(112.058136142119,-0.187792898288806,
-12.4997721971628));
#56151=CARTESIAN_POINT('Ctrl Pts',(112.053314345881,-0.33965107353463,-12.4999168221212));
#56152=CARTESIAN_POINT('Ctrl Pts',(112.046900761756,-0.491400509089169,
-12.5000720390346));
#56153=CARTESIAN_POINT('Ctrl Pts',(112.03890688688,-0.643114186770904,-12.5002246390813));
#56154=CARTESIAN_POINT('Ctrl Pts',(112.026216652062,-0.883958861557406,
-12.5004668908622));
#56155=CARTESIAN_POINT('Ctrl Pts',(112.009565615222,-1.1242936415883,-12.500703677216));
#56156=CARTESIAN_POINT('Ctrl Pts',(111.989043361922,-1.36439140510506,-12.5008640626113));
#56157=CARTESIAN_POINT('Ctrl Pts',(111.979775372988,-1.4728211853372,-12.5009364937449));
#56158=CARTESIAN_POINT('Ctrl Pts',(111.969717854519,-1.58120197427212,-12.5009931418907));
#56159=CARTESIAN_POINT('Ctrl Pts',(111.958879057757,-1.68955541748221,-12.5010268514762));
#56160=CARTESIAN_POINT('',(113.773164772043,-1.68935314531927,-12.5));
#56161=CARTESIAN_POINT('Ctrl Pts',(113.773164772043,-1.68901173527894,-12.4997638206505));
#56162=CARTESIAN_POINT('Ctrl Pts',(113.738783287824,-3.17726068106174,-12.2972111654493));
#56163=CARTESIAN_POINT('Ctrl Pts',(113.704401803605,-4.63022107289222,-11.8298957681816));
#56164=CARTESIAN_POINT('Ctrl Pts',(113.670020319386,-5.95395763049549,-11.1212072985898));
#56165=CARTESIAN_POINT('Ctrl Pts',(113.622374938865,-7.78837325939539,-10.1391167178218));
#56166=CARTESIAN_POINT('Ctrl Pts',(113.574729558344,-9.37462705959716,-8.6934925839394));
#56167=CARTESIAN_POINT('Ctrl Pts',(113.527084177824,-10.5223094586549,-6.95786367206226));
#56168=CARTESIAN_POINT('Ctrl Pts',(113.479438797303,-11.6699918577127,-5.22223476018512));
#56169=CARTESIAN_POINT('Ctrl Pts',(113.431793416782,-12.3791028556264,-3.19660107031332));
#56170=CARTESIAN_POINT('Ctrl Pts',(113.384148036262,-12.5645226998369,-1.12411413582959));
#56171=CARTESIAN_POINT('Ctrl Pts',(113.336502655741,-12.7499425440475,0.94837279865413));
#56172=CARTESIAN_POINT('Ctrl Pts',(113.28885727522,-12.4116712345548,3.06771297774975));
#56173=CARTESIAN_POINT('Ctrl Pts',(113.2412118947,-11.5903139457204,4.97950658623459));
#56174=CARTESIAN_POINT('Ctrl Pts',(113.193566514179,-10.768956656886,6.89130019471944));
#56175=CARTESIAN_POINT('Ctrl Pts',(113.145921133658,-9.46451338870981,8.5955472325935));
#56176=CARTESIAN_POINT('Ctrl Pts',(113.098275753138,-7.83356592756815,9.88767455482333));
#56177=CARTESIAN_POINT('Ctrl Pts',(113.050630372617,-6.20261846642654,11.1798018770531));
#56178=CARTESIAN_POINT('Ctrl Pts',(113.002984992096,-4.24516681231946,12.0598094836387));
#56179=CARTESIAN_POINT('Ctrl Pts',(112.955339611575,-2.19617816272136,12.4220636309878));
#56180=CARTESIAN_POINT('Ctrl Pts',(112.907694231055,-0.14718951312322,12.7843177783369));
#56181=CARTESIAN_POINT('Ctrl Pts',(112.860048850534,1.99333613196602,12.6288184664494));
#56182=CARTESIAN_POINT('Ctrl Pts',(112.812403470013,3.96845601763776,11.974231479739));
#56183=CARTESIAN_POINT('Ctrl Pts',(112.764758089493,5.94357590330954,11.3196444930286));
#56184=CARTESIAN_POINT('Ctrl Pts',(112.717112708972,7.75329002956387,10.1659698314953));
#56185=CARTESIAN_POINT('Ctrl Pts',(112.669467328451,9.18036504385502,8.65169129805265));
#56186=CARTESIAN_POINT('Ctrl Pts',(112.621821947931,10.6074400581462,7.13741276460996));
#56187=CARTESIAN_POINT('Ctrl Pts',(112.57417656741,11.6518759604741,5.26253035925789));
#56188=CARTESIAN_POINT('Ctrl Pts',(112.526531186889,12.1883019673065,3.25210017371475));
#56189=CARTESIAN_POINT('Ctrl Pts',(112.478885806369,12.7247279741389,1.24166998817161));
#56190=CARTESIAN_POINT('Ctrl Pts',(112.431240425848,12.7531440854758,-0.90430797756259));
#56191=CARTESIAN_POINT('Ctrl Pts',(112.383595045327,12.2701383463594,-2.92823708869029));
#56192=CARTESIAN_POINT('Ctrl Pts',(112.335949664806,11.7871326072431,-4.95216619981793));
#56193=CARTESIAN_POINT('Ctrl Pts',(112.288304284286,10.7927050176734,-6.85404645633905));
#56194=CARTESIAN_POINT('Ctrl Pts',(112.240658903765,9.40622600807702,-8.40557984913739));
#56195=CARTESIAN_POINT('Ctrl Pts',(112.193013523244,8.01974699848061,-9.95711324193578));
#56196=CARTESIAN_POINT('Ctrl Pts',(112.145368142724,6.24121656885751,-11.1582997710113));
#56197=CARTESIAN_POINT('Ctrl Pts',(112.097722762203,4.28412025495413,-11.864955489308));
#56198=CARTESIAN_POINT('Ctrl Pts',(112.07730111204,3.44527426775002,-12.1678405897586));
#56199=CARTESIAN_POINT('Ctrl Pts',(112.056879461876,2.57362339298663,-12.3798739146441));
#56200=CARTESIAN_POINT('Ctrl Pts',(112.036457811713,1.68935476637002,-12.4990499102299));
#56201=CARTESIAN_POINT('',(113.850743525999,1.68935314531929,-12.5));
#56202=CARTESIAN_POINT('Ctrl Pts',(113.850743525998,1.68901803546276,-12.4998490738946));
#56203=CARTESIAN_POINT('Ctrl Pts',(113.851245431161,1.67983313575413,-12.4998578124018));
#56204=CARTESIAN_POINT('Ctrl Pts',(113.851741602467,1.67064795642428,-12.4998665822449));
#56205=CARTESIAN_POINT('Ctrl Pts',(113.852232035536,1.66146248209855,-12.4998753809702));
#56206=CARTESIAN_POINT('Ctrl Pts',(113.865298014292,1.41674567995777,-12.5001097941157));
#56207=CARTESIAN_POINT('Ctrl Pts',(113.874273658148,1.17214237386868,-12.5003668415169));
#56208=CARTESIAN_POINT('Ctrl Pts',(113.879109652811,0.927352163801529,-12.500585695352));
#56209=CARTESIAN_POINT('Ctrl Pts',(113.881320847749,0.815425060722326,-12.5006857633889));
#56210=CARTESIAN_POINT('Ctrl Pts',(113.882666584728,0.703458199116043,-12.5007775539845));
#56211=CARTESIAN_POINT('Ctrl Pts',(113.883142149674,0.591419750083688,-12.5008534506478));
#56212=CARTESIAN_POINT('Ctrl Pts',(113.88389513068,0.414024790970592,-12.5009736208714));
#56213=CARTESIAN_POINT('Ctrl Pts',(113.882465575537,0.236710970496718,-12.5010539805042));
#56214=CARTESIAN_POINT('Ctrl Pts',(113.878853967929,0.0593541582956196,
-12.5010583969255));
#56215=CARTESIAN_POINT('Ctrl Pts',(113.878745629308,0.0540339257122809,
-12.5010585294064));
#56216=CARTESIAN_POINT('Ctrl Pts',(113.878635328905,0.0487137387383808,
-12.501058593009));
#56217=CARTESIAN_POINT('Ctrl Pts',(113.87852306692,0.0433935940314725,-12.5010585866647));
#56218=CARTESIAN_POINT('Ctrl Pts',(113.87835627776,0.0354893826665526,-12.5010585772388));
#56219=CARTESIAN_POINT('Ctrl Pts',(113.878185158713,0.0275852645996462,
-12.5010584134173));
#56220=CARTESIAN_POINT('Ctrl Pts',(113.878009710432,0.0196812288965393,
-12.5010580987177));
#56221=CARTESIAN_POINT('Ctrl Pts',(113.877929058385,0.016047812504426,-12.501057954053));
#56222=CARTESIAN_POINT('Ctrl Pts',(113.877847491578,0.0124144169823269,
-12.5010577775052));
#56223=CARTESIAN_POINT('Ctrl Pts',(113.877765010083,0.00878104134032691,
-12.501057569414));
#56224=CARTESIAN_POINT('Ctrl Pts',(113.877716556822,0.00664663658689854,
-12.5010574471721));
#56225=CARTESIAN_POINT('Ctrl Pts',(113.87766778792,0.00451223907795595,
-12.5010573140449));
#56226=CARTESIAN_POINT('Ctrl Pts',(113.877618703389,0.00237784854568333,
-12.5010571701012));
#56227=CARTESIAN_POINT('Ctrl Pts',(113.877576325151,0.000535074307108699,
-12.5010570458241));
#56228=CARTESIAN_POINT('Ctrl Pts',(113.877533711646,-0.00130769448144772,
-12.5010569134842));
#56229=CARTESIAN_POINT('Ctrl Pts',(113.877490862883,-0.003150457944898,
-12.5010567731257));
#56230=CARTESIAN_POINT('Ctrl Pts',(113.877438679203,-0.00539468091234346,
-12.501056602189));
#56231=CARTESIAN_POINT('Ctrl Pts',(113.877386146601,-0.00763889568166643,
-12.5010564193593));
#56232=CARTESIAN_POINT('Ctrl Pts',(113.877333265096,-0.00988310241490448,
-12.5010562247161));
#56233=CARTESIAN_POINT('Ctrl Pts',(113.87723349659,-0.0141171186989501,
-12.501055857494));
#56234=CARTESIAN_POINT('Ctrl Pts',(113.877132486228,-0.0183511048866481,
-12.501055448223));
#56235=CARTESIAN_POINT('Ctrl Pts',(113.877030234127,-0.0225850627128733,
-12.501054997436));
#56236=CARTESIAN_POINT('Ctrl Pts',(113.876447802145,-0.0467018526614194,
-12.5010524297353));
#56237=CARTESIAN_POINT('Ctrl Pts',(113.875825088342,-0.0708174645771705,
-12.5010485152761));
#56238=CARTESIAN_POINT('Ctrl Pts',(113.875162117312,-0.0949322080277007,
-12.5010433511533));
#56239=CARTESIAN_POINT('Ctrl Pts',(113.874314464092,-0.125764535557451,
-12.5010367484736));
#56240=CARTESIAN_POINT('Ctrl Pts',(113.87340102322,-0.156594634349324,-12.5010281033168));
#56241=CARTESIAN_POINT('Ctrl Pts',(113.872421856537,-0.187423148993577,
-12.5010176130637));
#56242=CARTESIAN_POINT('Ctrl Pts',(113.867600060503,-0.339234696795374,
-12.5009659549938));
#56243=CARTESIAN_POINT('Ctrl Pts',(113.861186476698,-0.490943663131368,
-12.5008698967933));
#56244=CARTESIAN_POINT('Ctrl Pts',(113.853192602255,-0.642625450334506,
-12.5007507198107));
#56245=CARTESIAN_POINT('Ctrl Pts',(113.840649972264,-0.88061874718513,-12.5005637275323));
#56246=CARTESIAN_POINT('Ctrl Pts',(113.824238143371,-1.11813508366469,-12.5003220898495));
#56247=CARTESIAN_POINT('Ctrl Pts',(113.804043611354,-1.3554470748682,-12.5000866508592));
#56248=CARTESIAN_POINT('Ctrl Pts',(113.794578642875,-1.46667275290384,-12.4999763030373));
#56249=CARTESIAN_POINT('Ctrl Pts',(113.784282727988,-1.57785288254529,-12.4998670128323));
#56250=CARTESIAN_POINT('Ctrl Pts',(113.773164772043,-1.68901173527787,-12.4997638206507));
#56251=CARTESIAN_POINT('Ctrl Pts',(115.587450486329,-1.68938454186076,-12.4990815932618));
#56252=CARTESIAN_POINT('Ctrl Pts',(115.567697044117,-2.54471940650875,-12.3838651769404));
#56253=CARTESIAN_POINT('Ctrl Pts',(115.547943601905,-3.38823356963067,-12.1817460641902));
#56254=CARTESIAN_POINT('Ctrl Pts',(115.528190159693,-4.20164592391042,-11.8944119192506));
#56255=CARTESIAN_POINT('Ctrl Pts',(115.480544779172,-6.16359973044633,-11.2013608284406));
#56256=CARTESIAN_POINT('Ctrl Pts',(115.432899398651,-7.95042834650364,-10.0125488741543));
#56257=CARTESIAN_POINT('Ctrl Pts',(115.385254018131,-9.34764570429239,-8.4706778377342));
#56258=CARTESIAN_POINT('Ctrl Pts',(115.33760863761,-10.7448630620811,-6.92880680131414));
#56259=CARTESIAN_POINT('Ctrl Pts',(115.289963257089,-11.7524691616013,-5.03387668276034));
#56260=CARTESIAN_POINT('Ctrl Pts',(115.242317876569,-12.2495137367818,-3.01334970010246));
#56261=CARTESIAN_POINT('Ctrl Pts',(115.194672496048,-12.7465583119623,-0.99282271744458));
#56262=CARTESIAN_POINT('Ctrl Pts',(115.147027115527,-12.7330413628031,1.15330112931739));
#56263=CARTESIAN_POINT('Ctrl Pts',(115.099381735007,-12.2105854182327,3.16740698507967));
#56264=CARTESIAN_POINT('Ctrl Pts',(115.051736354486,-11.6881294736624,5.18151284084189));
#56265=CARTESIAN_POINT('Ctrl Pts',(115.004090973965,-10.656734533681,7.06360070560443));
#56266=CARTESIAN_POINT('Ctrl Pts',(114.956445593445,-9.24020643457968,8.58774989558119));
#56267=CARTESIAN_POINT('Ctrl Pts',(114.908800212924,-7.82367833547828,10.111899085558));
#56268=CARTESIAN_POINT('Ctrl Pts',(114.861154832403,-6.02201707725687,11.278109600749));
#56269=CARTESIAN_POINT('Ctrl Pts',(114.813509451882,-4.05148915570895,11.9463927134979));
#56270=CARTESIAN_POINT('Ctrl Pts',(114.765864071362,-2.08096123416109,12.6146758262467));
#56271=CARTESIAN_POINT('Ctrl Pts',(114.718218690841,0.058433350713282,12.7850315365535));
#56272=CARTESIAN_POINT('Ctrl Pts',(114.67057331032,2.10988751401252,12.4370108110418));
#56273=CARTESIAN_POINT('Ctrl Pts',(114.6229279298,4.16134167731182,12.0889900855301));
#56274=CARTESIAN_POINT('Ctrl Pts',(114.575282549279,6.12485541903599,11.2225929241999));
#56275=CARTESIAN_POINT('Ctrl Pts',(114.527637168758,7.76473391175164,9.94181927604152));
#56276=CARTESIAN_POINT('Ctrl Pts',(114.479991788238,9.4046124044673,8.66104562788315));
#56277=CARTESIAN_POINT('Ctrl Pts',(114.432346407717,10.7208556481745,6.96589549289665));
#56278=CARTESIAN_POINT('Ctrl Pts',(114.384701027196,11.5554653978966,5.05985006458397));
#56279=CARTESIAN_POINT('Ctrl Pts',(114.337055646676,12.3900751476188,3.15380463627128));
#56280=CARTESIAN_POINT('Ctrl Pts',(114.289410266155,12.7430514033559,1.03686391463243));
#56281=CARTESIAN_POINT('Ctrl Pts',(114.241764885634,12.5720238593694,-1.03686031681585));
#56282=CARTESIAN_POINT('Ctrl Pts',(114.194119505113,12.4009963153829,-3.11058454826412));
#56283=CARTESIAN_POINT('Ctrl Pts',(114.146474124593,11.7059649716726,-5.14109228952181));
#56284=CARTESIAN_POINT('Ctrl Pts',(114.098828744072,10.570359492693,-6.88464693599394));
#56285=CARTESIAN_POINT('Ctrl Pts',(114.051183363551,9.43475401371345,-8.62820158246606));
#56286=CARTESIAN_POINT('Ctrl Pts',(114.003537983031,7.85857439946455,-10.0848031341526));
#56287=CARTESIAN_POINT('Ctrl Pts',(113.95589260251,6.03102094707087,-11.0796051181335));
#56288=CARTESIAN_POINT('Ctrl Pts',(113.92084291034,4.68660549206775,-11.8114180017347));
#56289=CARTESIAN_POINT('Ctrl Pts',(113.885793218169,3.20615621736254,-12.2933227819493));
#56290=CARTESIAN_POINT('Ctrl Pts',(113.850743525998,1.68901803546259,-12.4998490738946));
#56291=CARTESIAN_POINT('Ctrl Pts',(110.227483930805,1.91900181571061,-12.4668097796068));
#56292=CARTESIAN_POINT('Ctrl Pts',(110.259102396748,3.28412020033192,-12.2566786630614));
#56293=CARTESIAN_POINT('Ctrl Pts',(110.353957794575,7.2847919271857,-10.9560812916465));
#56294=CARTESIAN_POINT('Ctrl Pts',(110.480431658344,11.2946802597942,-6.74182720966569));
#56295=CARTESIAN_POINT('Ctrl Pts',(110.638523988057,13.1491225142247,0.0172659150134116));
#56296=CARTESIAN_POINT('Ctrl Pts',(110.796616317769,11.5505961778161,7.1230034539131));
#56297=CARTESIAN_POINT('Ctrl Pts',(110.954708647481,5.90917860665286,11.7527359321285));
#56298=CARTESIAN_POINT('Ctrl Pts',(111.049564045308,1.78853735160741,12.562354535742));
#56299=CARTESIAN_POINT('Ctrl Pts',(111.08118251125,0.408063986721388,12.6070376311147));
#56300=CARTESIAN_POINT('Ctrl Pts',(110.423013221971,1.86747807250454,-12.1320853929883));
#56301=CARTESIAN_POINT('Ctrl Pts',(110.454631687913,3.19594406392888,-11.9275961375395));
#56302=CARTESIAN_POINT('Ctrl Pts',(110.54948708574,7.08920078939042,-10.6619188190556));
#56303=CARTESIAN_POINT('Ctrl Pts',(110.67596094951,10.9914266617329,-6.56081426270191));
#56304=CARTESIAN_POINT('Ctrl Pts',(110.834053279222,12.7960785482098,0.0168023382913589));
#56305=CARTESIAN_POINT('Ctrl Pts',(110.992145608934,11.2404714314658,6.93175621391007));
#56306=CARTESIAN_POINT('Ctrl Pts',(111.150237938646,5.75052164312344,11.4371838866961));
#56307=CARTESIAN_POINT('Ctrl Pts',(111.245093336474,1.74051648030636,12.2250648448911));
#56308=CARTESIAN_POINT('Ctrl Pts',(111.276711802416,0.397107778190796,12.2685482330447));
#56309=CARTESIAN_POINT('Ctrl Pts',(110.618542513136,1.81595432929846,-11.7973610063697));
#56310=CARTESIAN_POINT('Ctrl Pts',(110.650160979079,3.10776792752583,-11.5985136120176));
#56311=CARTESIAN_POINT('Ctrl Pts',(110.745016376906,6.89360965159514,-10.3677563464648));
#56312=CARTESIAN_POINT('Ctrl Pts',(110.871490240676,10.6881730636716,-6.37980131573813));
#56313=CARTESIAN_POINT('Ctrl Pts',(111.029582570388,12.4430345821949,0.0163387615693034));
#56314=CARTESIAN_POINT('Ctrl Pts',(111.1876749001,10.9303466851155,6.74050897390706));
#56315=CARTESIAN_POINT('Ctrl Pts',(111.345767229812,5.59186467959401,11.1216318412638));
#56316=CARTESIAN_POINT('Ctrl Pts',(111.440622627639,1.6924956090053,11.8877751540402));
#56317=CARTESIAN_POINT('Ctrl Pts',(111.472241093582,0.386151569660204,11.9300588349748));
#56318=CARTESIAN_POINT('Ctrl Pts',(110.814071804302,1.76443058609239,-11.4626366197512));
#56319=CARTESIAN_POINT('Ctrl Pts',(110.845690270244,3.01959179112279,-11.2694310864958));
#56320=CARTESIAN_POINT('Ctrl Pts',(110.940545668071,6.69801851379986,-10.0735938738739));
#56321=CARTESIAN_POINT('Ctrl Pts',(111.067019531841,10.3849194656103,-6.19878836877434));
#56322=CARTESIAN_POINT('Ctrl Pts',(111.225111861553,12.0899906161801,0.0158751848472512));
#56323=CARTESIAN_POINT('Ctrl Pts',(111.383204191265,10.6202219387652,6.54926173390403));
#56324=CARTESIAN_POINT('Ctrl Pts',(111.541296520977,5.43320771606459,10.8060797958314));
#56325=CARTESIAN_POINT('Ctrl Pts',(111.636151918805,1.64447473770424,11.5504854631893));
#56326=CARTESIAN_POINT('Ctrl Pts',(111.667770384747,0.375195361129611,11.5915694369049));
#56327=CARTESIAN_POINT('',(110.231099956476,2.07496815725958,-12.4418013645918));
#56328=CARTESIAN_POINT('',(110.814071804302,1.7644305860926,-11.4626366197512));
#56329=CARTESIAN_POINT('Ctrl Pts',(110.231099956476,2.07498074443087,-12.4418052243385));
#56330=CARTESIAN_POINT('Ctrl Pts',(110.231972064293,2.07467345273846,-12.4403226893382));
#56331=CARTESIAN_POINT('Ctrl Pts',(110.232844150751,2.07436555040161,-12.438840267401));
#56332=CARTESIAN_POINT('Ctrl Pts',(110.233716214951,2.07405703700522,-12.4373579600969));
#56333=CARTESIAN_POINT('Ctrl Pts',(110.294415797386,2.05258311988967,-12.3341827185608));
#56334=CARTESIAN_POINT('Ctrl Pts',(110.355166952545,2.02809901882949,-12.2312926779149));
#56335=CARTESIAN_POINT('Ctrl Pts',(110.415658732524,2.00040603564854,-12.1292271991975));
#56336=CARTESIAN_POINT('Ctrl Pts',(110.452538273774,1.98352267536519,-12.067001752469));
#56337=CARTESIAN_POINT('Ctrl Pts',(110.489321408438,1.96544758855314,-12.0050823006931));
#56338=CARTESIAN_POINT('Ctrl Pts',(110.525937674498,1.94614368122397,-11.9435859633641));
#56339=CARTESIAN_POINT('Ctrl Pts',(110.583400229787,1.91584971732351,-11.847078671276));
#56340=CARTESIAN_POINT('Ctrl Pts',(110.640785053146,1.88235189016964,-11.7510557289317));
#56341=CARTESIAN_POINT('Ctrl Pts',(110.69768363355,1.84542156071811,-11.6561947635924));
#56342=CARTESIAN_POINT('Ctrl Pts',(110.736753032922,1.82006335705024,-11.5910584998511));
#56343=CARTESIAN_POINT('Ctrl Pts',(110.775593174595,1.79308780999508,-11.5264694206628));
#56344=CARTESIAN_POINT('Ctrl Pts',(110.814071804302,1.76443058609264,-11.4626366197512));
#56345=CARTESIAN_POINT('',(111.05480378529,1.55646560811612,12.5172412639667));
#56346=CARTESIAN_POINT('Ctrl Pts',(111.05480378529,1.55655218426862,12.5176530308837));
#56347=CARTESIAN_POINT('Ctrl Pts',(111.031978228001,2.54616542269904,12.3953416596267));
#56348=CARTESIAN_POINT('Ctrl Pts',(111.009152670712,3.52132431918197,12.1566148832709));
#56349=CARTESIAN_POINT('Ctrl Pts',(110.986327113423,4.45387699804358,11.8039175907423));
#56350=CARTESIAN_POINT('Ctrl Pts',(110.923090181538,7.03746212088551,10.8267894364854));
#56351=CARTESIAN_POINT('Ctrl Pts',(110.859853249654,9.29402914935078,8.97489644519926));
#56352=CARTESIAN_POINT('Ctrl Pts',(110.796616317769,10.7420179308651,6.62780244177627));
#56353=CARTESIAN_POINT('Ctrl Pts',(110.733379385884,12.1900067123795,4.28070843835325));
#56354=CARTESIAN_POINT('Ctrl Pts',(110.670142453999,12.829417246943,1.43841342279337));
#56355=CARTESIAN_POINT('Ctrl Pts',(110.606905522114,12.5480361572827,-1.31144308230768));
#56356=CARTESIAN_POINT('Ctrl Pts',(110.575287056172,12.4073456124525,-2.68637133485819));
#56357=CARTESIAN_POINT('Ctrl Pts',(110.543668590229,12.0364571615664,-4.038189959794));
#56358=CARTESIAN_POINT('Ctrl Pts',(110.512050124287,11.4550408332583,-5.29059021658293));
#56359=CARTESIAN_POINT('Ctrl Pts',(110.448813192402,10.2922081766421,-7.79539073016086));
#56360=CARTESIAN_POINT('Ctrl Pts',(110.385576260517,8.28726401033785,-9.90251777115129));
#56361=CARTESIAN_POINT('Ctrl Pts',(110.322339328632,5.84087296519027,-11.1829367276658));
#56362=CARTESIAN_POINT('Ctrl Pts',(110.29192620458,4.66430743428013,-11.7987404898432));
#56363=CARTESIAN_POINT('Ctrl Pts',(110.261513080528,3.38563409942451,-12.2233245355487));
#56364=CARTESIAN_POINT('Ctrl Pts',(110.231099956476,2.07498074443113,-12.4418052243385));
#56365=CARTESIAN_POINT('',(111.667770384747,0.375195361129818,11.5915694369049));
#56366=CARTESIAN_POINT('Ctrl Pts',(111.667770384747,0.375195361129768,11.5915694369049));
#56367=CARTESIAN_POINT('Ctrl Pts',(111.648728343226,0.485214774885859,11.6162974530754));
#56368=CARTESIAN_POINT('Ctrl Pts',(111.621953768639,0.590095044314391,11.6533229147721));
#56369=CARTESIAN_POINT('Ctrl Pts',(111.542930074451,0.829633389147557,11.7663849110434));
#56370=CARTESIAN_POINT('Ctrl Pts',(111.485269589771,0.956968090875436,11.8514792232639));
#56371=CARTESIAN_POINT('Ctrl Pts',(111.313120815466,1.26580623366652,12.1112516087257));
#56372=CARTESIAN_POINT('Ctrl Pts',(111.185217860899,1.42619077431694,12.3099604514317));
#56373=CARTESIAN_POINT('Ctrl Pts',(111.05480378529,1.55646560811609,12.5172412639668));
#56374=CARTESIAN_POINT('Ctrl Pts',(110.814071804302,1.76443058609239,-11.4626366197512));
#56375=CARTESIAN_POINT('Ctrl Pts',(110.845690270244,3.01959179112279,-11.2694310864958));
#56376=CARTESIAN_POINT('Ctrl Pts',(110.940545668071,6.69801851379986,-10.0735938738739));
#56377=CARTESIAN_POINT('Ctrl Pts',(111.067019531841,10.3849194656103,-6.19878836877434));
#56378=CARTESIAN_POINT('Ctrl Pts',(111.225111861553,12.0899906161801,0.0158751848472512));
#56379=CARTESIAN_POINT('Ctrl Pts',(111.383204191265,10.6202219387652,6.54926173390403));
#56380=CARTESIAN_POINT('Ctrl Pts',(111.541296520977,5.43320771606459,10.8060797958314));
#56381=CARTESIAN_POINT('Ctrl Pts',(111.636151918805,1.64447473770424,11.5504854631893));
#56382=CARTESIAN_POINT('Ctrl Pts',(111.667770384747,0.375195361129611,11.5915694369049));
#56383=CARTESIAN_POINT('Ctrl Pts',(109.326702434851,-2.19316391405416,12.421511425575));
#56384=CARTESIAN_POINT('Ctrl Pts',(109.386775022159,-4.77735704569893,11.965241739134));
#56385=CARTESIAN_POINT('Ctrl Pts',(109.47688390312,-8.4223533736891,10.0292554895209));
#56386=CARTESIAN_POINT('Ctrl Pts',(109.597029077735,-11.4845940933567,5.68566566705009));
#56387=CARTESIAN_POINT('Ctrl Pts',(109.71717425235,-13.0841517589515,0.621609920093159));
#56388=CARTESIAN_POINT('Ctrl Pts',(109.867355720619,-11.971562716397,-6.17807840082615));
#56389=CARTESIAN_POINT('Ctrl Pts',(110.017537188888,-7.07598515172816,-11.0249828325528));
#56390=CARTESIAN_POINT('Ctrl Pts',(110.107646069849,-3.28369789911874,-12.2491959409189));
#56391=CARTESIAN_POINT('Ctrl Pts',(110.137682363503,-1.98801473901782,-12.4559909861499));
#56392=CARTESIAN_POINT('Ctrl Pts',(109.522231726017,-2.13427912645707,12.0880032654038));
#56393=CARTESIAN_POINT('Ctrl Pts',(109.582304313324,-4.6490886326046,11.6439840739673));
#56394=CARTESIAN_POINT('Ctrl Pts',(109.672413194286,-8.1962195738854,9.75997758672801));
#56395=CARTESIAN_POINT('Ctrl Pts',(109.792558368901,-11.1762414529122,5.53300985641644));
#56396=CARTESIAN_POINT('Ctrl Pts',(109.912703543516,-12.732852208436,0.604920165224213));
#56397=CARTESIAN_POINT('Ctrl Pts',(110.062885011785,-11.6501353377852,-6.01220168178129));
#56398=CARTESIAN_POINT('Ctrl Pts',(110.213066480053,-6.88600031747581,-10.7289704058498));
#56399=CARTESIAN_POINT('Ctrl Pts',(110.303175361015,-3.19553310118293,-11.920314320811));
#56400=CARTESIAN_POINT('Ctrl Pts',(110.333211654668,-1.93463805116661,-12.1215570759298));
#56401=CARTESIAN_POINT('Ctrl Pts',(109.717761017183,-2.07539433885998,11.7544951052327));
#56402=CARTESIAN_POINT('Ctrl Pts',(109.77783360449,-4.52082021951027,11.3227264088006));
#56403=CARTESIAN_POINT('Ctrl Pts',(109.867942485451,-7.97008577408171,9.49069968393512));
#56404=CARTESIAN_POINT('Ctrl Pts',(109.988087660066,-10.8678888124676,5.38035404578278));
#56405=CARTESIAN_POINT('Ctrl Pts',(110.108232834681,-12.3815526579205,0.58823041035528));
#56406=CARTESIAN_POINT('Ctrl Pts',(110.25841430295,-11.3287079591734,-5.84632496273644));
#56407=CARTESIAN_POINT('Ctrl Pts',(110.408595771219,-6.69601548322346,-10.4329579791468));
#56408=CARTESIAN_POINT('Ctrl Pts',(110.49870465218,-3.10736830324712,-11.5914327007031));
#56409=CARTESIAN_POINT('Ctrl Pts',(110.528740945834,-1.8812613633154,-11.7871231657096));
#56410=CARTESIAN_POINT('Ctrl Pts',(109.913290308348,-2.01650955126289,11.4209869450615));
#56411=CARTESIAN_POINT('Ctrl Pts',(109.973362895656,-4.39255180641593,11.0014687436339));
#56412=CARTESIAN_POINT('Ctrl Pts',(110.063471776617,-7.74395197427801,9.22142178114223));
#56413=CARTESIAN_POINT('Ctrl Pts',(110.183616951232,-10.5595361720231,5.22769823514912));
#56414=CARTESIAN_POINT('Ctrl Pts',(110.303762125847,-12.0302531074049,0.571540655486336));
#56415=CARTESIAN_POINT('Ctrl Pts',(110.453943594116,-11.0072805805616,-5.68044824369158));
#56416=CARTESIAN_POINT('Ctrl Pts',(110.604125062384,-6.50603064897112,-10.1369455524438));
#56417=CARTESIAN_POINT('Ctrl Pts',(110.694233943346,-3.01920350531131,-11.2625510805952));
#56418=CARTESIAN_POINT('Ctrl Pts',(110.724270236999,-1.82788467546419,-11.4526892554894));
#56419=CARTESIAN_POINT('',(109.326702434851,-2.19316391405513,12.4215114255748));
#56420=CARTESIAN_POINT('',(109.916925613585,-2.16013089941446,11.3946911745123));
#56421=CARTESIAN_POINT('Ctrl Pts',(109.326702434851,-2.19316391405513,12.4215114255748));
#56422=CARTESIAN_POINT('Ctrl Pts',(109.327624760155,-2.19323679357333,12.4198905709872));
#56423=CARTESIAN_POINT('Ctrl Pts',(109.32854712709,-2.1933090913526,12.4182697125788));
#56424=CARTESIAN_POINT('Ctrl Pts',(109.329470288881,-2.19338086437603,12.4166475270919));
#56425=CARTESIAN_POINT('Ctrl Pts',(109.398328572974,-2.19873438667771,12.2956493335014));
#56426=CARTESIAN_POINT('Ctrl Pts',(109.467540319419,-2.20085626981063,12.1744176340077));
#56427=CARTESIAN_POINT('Ctrl Pts',(109.536874740044,-2.19969030210839,12.0534059975458));
#56428=CARTESIAN_POINT('Ctrl Pts',(109.566227462976,-2.19919668974957,12.002175728299));
#56429=CARTESIAN_POINT('Ctrl Pts',(109.59560217221,-2.1981144327467,11.9509847056692));
#56430=CARTESIAN_POINT('Ctrl Pts',(109.6249813567,-2.19644190302192,11.8998664254177));
#56431=CARTESIAN_POINT('Ctrl Pts',(109.690063492132,-2.19273683741327,11.7866268343208));
#56432=CARTESIAN_POINT('Ctrl Pts',(109.755392190482,-2.18612067777798,11.6733542830029));
#56433=CARTESIAN_POINT('Ctrl Pts',(109.820754601349,-2.17648427702135,11.5604583010507));
#56434=CARTESIAN_POINT('Ctrl Pts',(109.852811866484,-2.17175806435727,11.5050879990986));
#56435=CARTESIAN_POINT('Ctrl Pts',(109.884877241005,-2.16630611914395,11.4498080248238));
#56436=CARTESIAN_POINT('Ctrl Pts',(109.916925613585,-2.16011982372873,11.394665082805));
#56437=CARTESIAN_POINT('',(110.134936209547,-2.10638458259796,-12.4365211389598));
#56438=CARTESIAN_POINT('Ctrl Pts',(110.134936209547,-2.10638646513139,-12.4365237339679));
#56439=CARTESIAN_POINT('Ctrl Pts',(110.105815300545,-3.36065871434644,-12.224149455599));
#56440=CARTESIAN_POINT('Ctrl Pts',(110.076694391543,-4.58342315705692,-11.8229864006375));
#56441=CARTESIAN_POINT('Ctrl Pts',(110.047573482542,-5.71689598821299,-11.2459505852671));
#56442=CARTESIAN_POINT('Ctrl Pts',(109.987500895234,-8.05510066466195,-10.0556019462074));
#56443=CARTESIAN_POINT('Ctrl Pts',(109.927428307927,-10.0133316905295,-8.11684017351675));
#56444=CARTESIAN_POINT('Ctrl Pts',(109.867355720619,-11.2149650119742,-5.78752162298753));
#56445=CARTESIAN_POINT('Ctrl Pts',(109.807283133311,-12.4165983334188,-3.45820307245836));
#56446=CARTESIAN_POINT('Ctrl Pts',(109.747210546004,-12.8616339504406,-0.73832774409066));
#56447=CARTESIAN_POINT('Ctrl Pts',(109.687137958696,-12.476793267583,1.85631594768421));
#56448=CARTESIAN_POINT('Ctrl Pts',(109.657101665043,-12.2843729261541,3.15363779357164));
#56449=CARTESIAN_POINT('Ctrl Pts',(109.627065371389,-11.8844835097554,4.41965173031087));
#56450=CARTESIAN_POINT('Ctrl Pts',(109.597029077735,-11.3017587115976,5.59560742648933));
#56451=CARTESIAN_POINT('Ctrl Pts',(109.566992784081,-10.7190339134398,6.77156312266779));
#56452=CARTESIAN_POINT('Ctrl Pts',(109.536956490428,-9.9534737335229,7.85746057828549));
#56453=CARTESIAN_POINT('Ctrl Pts',(109.506920196774,-9.03810068824607,8.7965017986543));
#56454=CARTESIAN_POINT('Ctrl Pts',(109.446847609466,-7.20735459769238,10.6745842393919));
#56455=CARTESIAN_POINT('Ctrl Pts',(109.386775022159,-4.77735704569893,11.965241739134));
#56456=CARTESIAN_POINT('Ctrl Pts',(109.326702434851,-2.19316391405416,12.421511425575));
#56457=CARTESIAN_POINT('',(110.724270236999,-1.82788467546431,-11.4526892554894));
#56458=CARTESIAN_POINT('Ctrl Pts',(110.724270236999,-1.82788467546435,-11.4526892554894));
#56459=CARTESIAN_POINT('Ctrl Pts',(110.667526075141,-1.86589045855304,-11.5451485282515));
#56460=CARTESIAN_POINT('Ctrl Pts',(110.610252804328,-1.90043345022693,-11.6392079111746));
#56461=CARTESIAN_POINT('Ctrl Pts',(110.552831053726,-1.93172806060983,-11.7341940513259));
#56462=CARTESIAN_POINT('Ctrl Pts',(110.511546885066,-1.95422775732101,-11.8024856618947));
#56463=CARTESIAN_POINT('Ctrl Pts',(110.470185965843,-1.97504883978107,-11.8712554904881));
#56464=CARTESIAN_POINT('Ctrl Pts',(110.428889752719,-1.99428382657138,-11.9402424301157));
#56465=CARTESIAN_POINT('Ctrl Pts',(110.368519311111,-2.02240322442872,-12.0410936146522));
#56466=CARTESIAN_POINT('Ctrl Pts',(110.307888837394,-2.04731573305252,-12.1430752821224));
#56467=CARTESIAN_POINT('Ctrl Pts',(110.247288094794,-2.06919976167528,-12.2456458555069));
#56468=CARTESIAN_POINT('Ctrl Pts',(110.209803232032,-2.08273622631927,-12.3090913464659));
#56469=CARTESIAN_POINT('Ctrl Pts',(110.172329744684,-2.09511475306599,-12.3727616097936));
#56470=CARTESIAN_POINT('Ctrl Pts',(110.134936209547,-2.1063864651313,-12.4365237339679));
#56471=CARTESIAN_POINT('Ctrl Pts',(109.916925613585,-2.16011982372873,11.394665082805));
#56472=CARTESIAN_POINT('Ctrl Pts',(109.97578643248,-4.48246569417521,10.9533734556446));
#56473=CARTESIAN_POINT('Ctrl Pts',(110.064683545029,-7.7723495857832,9.18114161129006));
#56474=CARTESIAN_POINT('Ctrl Pts',(110.183616951232,-10.5595361720231,5.22769823514912));
#56475=CARTESIAN_POINT('Ctrl Pts',(110.303762125847,-12.0302531074049,0.571540655486336));
#56476=CARTESIAN_POINT('Ctrl Pts',(110.453943594116,-11.0072805805616,-5.68044824369158));
#56477=CARTESIAN_POINT('Ctrl Pts',(110.604125062384,-6.50603064897112,-10.1369455524438));
#56478=CARTESIAN_POINT('Ctrl Pts',(110.694233943346,-3.01920350531131,-11.2625510805952));
#56479=CARTESIAN_POINT('Ctrl Pts',(110.724270236999,-1.82788467546419,-11.4526892554894));
#56480=CARTESIAN_POINT('Ctrl Pts',(95.8594371265034,7.72546925504647,-9.97100992071173));
#56481=CARTESIAN_POINT('Ctrl Pts',(95.9065289275864,9.35161189059968,-8.71108589744992));
#56482=CARTESIAN_POINT('Ctrl Pts',(96.0007125297526,11.9743288123158,-5.38178778629994));
#56483=CARTESIAN_POINT('Ctrl Pts',(96.1419879330016,13.0987023614745,0.877951574918655));
#56484=CARTESIAN_POINT('Ctrl Pts',(96.283263336251,11.1494228248783,6.93064159208696));
#56485=CARTESIAN_POINT('Ctrl Pts',(96.4245387395001,6.58412487715065,11.3576480982333));
#56486=CARTESIAN_POINT('Ctrl Pts',(96.5658141427494,0.473894921020247,13.1194575864302));
#56487=CARTESIAN_POINT('Ctrl Pts',(96.7070895459985,-5.74751161001273,11.803044595664));
#56488=CARTESIAN_POINT('Ctrl Pts',(96.8483649492477,-10.6203344167321,7.71711632322287));
#56489=CARTESIAN_POINT('Ctrl Pts',(96.9896403524969,-13.0012049341669,1.82047628794835));
#56490=CARTESIAN_POINT('Ctrl Pts',(97.130915755746,-12.3314833773792,-4.50333217630157));
#56491=CARTESIAN_POINT('Ctrl Pts',(97.2721911589953,-8.76830984429102,-9.77047550087133));
#56492=CARTESIAN_POINT('Ctrl Pts',(97.4134665622445,-3.14774639686187,-12.7450839923031));
#56493=CARTESIAN_POINT('Ctrl Pts',(97.5547419654936,3.21140238251377,-12.7291930343172));
#56494=CARTESIAN_POINT('Ctrl Pts',(97.6960173687429,8.81702974551029,-9.72653341454518));
#56495=CARTESIAN_POINT('Ctrl Pts',(97.837292771992,12.3538351844813,-4.44164615268785));
#56496=CARTESIAN_POINT('Ctrl Pts',(97.9785681752412,12.9919449574235,1.8854258374657));
#56497=CARTESIAN_POINT('Ctrl Pts',(98.1198435784903,10.5816334489112,7.77010284454564));
#56498=CARTESIAN_POINT('Ctrl Pts',(98.2611189817397,5.68845452531083,11.8316080695515));
#56499=CARTESIAN_POINT('Ctrl Pts',(98.4023943849887,-0.539459568553354,
13.1169526921166));
#56500=CARTESIAN_POINT('Ctrl Pts',(98.5436697882381,-6.64079523061034,11.3245442816751));
#56501=CARTESIAN_POINT('Ctrl Pts',(98.6849451914871,-11.1839391316803,6.8749523638787));
#56502=CARTESIAN_POINT('Ctrl Pts',(98.8262205947364,-13.1028910201469,0.812226210291635));
#56503=CARTESIAN_POINT('Ctrl Pts',(98.9674959979855,-11.9473893053074,-5.44108015819797));
#56504=CARTESIAN_POINT('Ctrl Pts',(99.1087714012348,-7.98856013847796,-10.4176951105853));
#56505=CARTESIAN_POINT('Ctrl Pts',(99.2500468044839,-2.15530055285767,-12.9499090355197));
#56506=CARTESIAN_POINT('Ctrl Pts',(99.3913222077332,4.18367731586822,-12.4435649481564));
#56507=CARTESIAN_POINT('Ctrl Pts',(99.5325976109823,9.54099993169075,-9.01747108702972));
#56508=CARTESIAN_POINT('Ctrl Pts',(99.6738730142315,12.6596286918811,-3.4755238289693));
#56509=CARTESIAN_POINT('Ctrl Pts',(99.8151484174807,12.8078106257487,2.88191802051974));
#56510=CARTESIAN_POINT('Ctrl Pts',(99.9564238207299,9.95077642323533,8.56314854926595));
#56511=CARTESIAN_POINT('Ctrl Pts',(100.097699223979,4.75889868263185,12.2351276180707));
#56512=CARTESIAN_POINT('Ctrl Pts',(100.238974627228,-1.5496038684364,13.0362645091662));
#56513=CARTESIAN_POINT('Ctrl Pts',(100.380250030477,-7.49450840213069,10.7785809971637));
#56514=CARTESIAN_POINT('Ctrl Pts',(100.521525433727,-11.6809064867182,5.99181843437947));
#56515=CARTESIAN_POINT('Ctrl Pts',(100.662800836976,-13.1265044699315,-0.20086040648071));
#56516=CARTESIAN_POINT('Ctrl Pts',(100.804076240225,-11.4921082058848,-6.34640949563288));
#56517=CARTESIAN_POINT('Ctrl Pts',(100.945351643474,-7.16121134306135,-11.0028412967757));
#56518=CARTESIAN_POINT('Ctrl Pts',(101.086627046723,-1.15001263060479,-13.0775737601236));
#56519=CARTESIAN_POINT('Ctrl Pts',(101.227902449973,5.13102427789648,-12.0837930453008));
#56520=CARTESIAN_POINT('Ctrl Pts',(101.369177853222,10.2081210746434,-8.25467919591338));
#56521=CARTESIAN_POINT('Ctrl Pts',(101.510453256471,12.8899911560635,-2.48869292975802));
#56522=CARTESIAN_POINT('Ctrl Pts',(101.65172865972,12.5473623163237,3.86123858430473));
#56523=CARTESIAN_POINT('Ctrl Pts',(101.793004062969,9.26062875768555,9.30517165421206));
#56524=CARTESIAN_POINT('Ctrl Pts',(101.934279466218,3.80098744854767,12.5657454581098));
#56525=CARTESIAN_POINT('Ctrl Pts',(102.075554869468,-2.55051501846751,12.8779011349908));
#56526=CARTESIAN_POINT('Ctrl Pts',(102.216830272717,-8.30356634394493,10.1683946851865));
#56527=CARTESIAN_POINT('Ctrl Pts',(102.358105675966,-12.1082744048711,5.07298289356143));
#56528=CARTESIAN_POINT('Ctrl Pts',(102.499381079215,-13.0719050413637,-1.21275021813858));
#56529=CARTESIAN_POINT('Ctrl Pts',(102.640656482464,-10.9683526040717,-7.21392442813049));
#56530=CARTESIAN_POINT('Ctrl Pts',(102.781931885714,-6.29119323282064,-11.5224282253931));
#56531=CARTESIAN_POINT('Ctrl Pts',(102.923207288963,-0.13787248061121,-13.1273171547394));
#56532=CARTESIAN_POINT('Ctrl Pts',(103.064482692212,6.04779857842274,-11.6520211490045));
#56533=CARTESIAN_POINT('Ctrl Pts',(103.205758095461,10.8144182157478,-7.44270267825699));
#56534=CARTESIAN_POINT('Ctrl Pts',(103.347033498711,13.0435499812424,-1.48703341887253));
#56535=CARTESIAN_POINT('Ctrl Pts',(103.48830890196,12.2121518853349,4.81755236936213));
#56536=CARTESIAN_POINT('Ctrl Pts',(103.629584305209,8.51530262230923,9.99175088523157));
#56537=CARTESIAN_POINT('Ctrl Pts',(103.770859708458,2.8204284357127,12.8214916425883));
#56538=CARTESIAN_POINT('Ctrl Pts',(103.912135111707,-3.53622919650101,12.6428061589234));
#56539=CARTESIAN_POINT('Ctrl Pts',(104.053410514956,-9.06314837034476,9.49762107680137));
#56540=CARTESIAN_POINT('Ctrl Pts',(104.194685918206,-12.4634964600336,4.12392052468528));
#56541=CARTESIAN_POINT('Ctrl Pts',(104.335961321455,-12.9394180592167,-2.21741398690574));
#56542=CARTESIAN_POINT('Ctrl Pts',(104.477236724704,-10.3792432419859,-8.03845596033345));
#56543=CARTESIAN_POINT('Ctrl Pts',(104.618512127953,-5.3836897176547,-11.9733599933665));
#56544=CARTESIAN_POINT('Ctrl Pts',(104.759787531202,0.875089167220108,-13.0988428279727));
#56545=CARTESIAN_POINT('Ctrl Pts',(104.901062934452,6.92853771680435,-11.1508219275598));
#56546=CARTESIAN_POINT('Ctrl Pts',(105.042338337701,11.3562787952667,-6.58637960659581));
#56547=CARTESIAN_POINT('Ctrl Pts',(105.18361374095,13.1193902093838,-0.47651358412637));
#56548=CARTESIAN_POINT('Ctrl Pts',(105.324889144199,11.8041766362049,5.74516129508806));
#56549=CARTESIAN_POINT('Ctrl Pts',(105.466164547448,7.71923898892298,10.6187953056317));
#56550=CARTESIAN_POINT('Ctrl Pts',(105.607439950697,1.82306414753622,13.0008423923777));
#56551=CARTESIAN_POINT('Ctrl Pts',(105.748715353947,-4.50087301923505,12.332380250059));
#56552=CARTESIAN_POINT('Ctrl Pts',(105.889990757196,-9.76872882267729,8.77025715351674));
#56553=CARTESIAN_POINT('Ctrl Pts',(106.031266160445,-12.7444556205367,3.15028569732799));
#56554=CARTESIAN_POINT('Ctrl Pts',(106.172541563694,-12.7298339305292,-3.20886445301767));
#56555=CARTESIAN_POINT('Ctrl Pts',(106.313816966943,-9.72828818742371,-8.81509345370888));
#56556=CARTESIAN_POINT('Ctrl Pts',(106.455092370193,-4.44411238783274,-12.3529450963602));
#56557=CARTESIAN_POINT('Ctrl Pts',(106.596367773442,1.88284570183887,-12.9923301796687));
#56558=CARTESIAN_POINT('Ctrl Pts',(106.737643176691,7.76797513005415,-10.5831614434048));
#56559=CARTESIAN_POINT('Ctrl Pts',(106.87891857994,11.8305132965046,-5.69085458103121));
#56560=CARTESIAN_POINT('Ctrl Pts',(107.020193983189,13.116978503713,0.536933086160893));
#56561=CARTESIAN_POINT('Ctrl Pts',(107.161469386439,11.3260374316532,6.63834908837963));
#56562=CARTESIAN_POINT('Ctrl Pts',(107.302744789688,6.87682287379193,11.1829109557715));
#56563=CARTESIAN_POINT('Ctrl Pts',(107.396928391854,2.83606438077655,12.4616371835023));
#56564=CARTESIAN_POINT('Ctrl Pts',(107.444020192937,0.782909338906897,12.5893195613048));
#56565=CARTESIAN_POINT('Ctrl Pts',(96.0549664176689,7.51804626524795,-9.70329586726262));
#56566=CARTESIAN_POINT('Ctrl Pts',(96.102058218752,9.10052820445122,-8.47719984838426));
#56567=CARTESIAN_POINT('Ctrl Pts',(96.1962418209181,11.6528271661266,-5.23729086627577));
#56568=CARTESIAN_POINT('Ctrl Pts',(96.3375172241673,12.7470121383177,0.854379241050541));
#56569=CARTESIAN_POINT('Ctrl Pts',(96.4787926274164,10.850069278768,6.74455912216921));
#56570=CARTESIAN_POINT('Ctrl Pts',(96.6200680306657,6.40734611819909,11.0527038614704));
#56571=CARTESIAN_POINT('Ctrl Pts',(96.7613434339148,0.461171201835904,12.767210101226));
#56572=CARTESIAN_POINT('Ctrl Pts',(96.9026188371641,-5.59319528272015,11.4861418007744));
#56573=CARTESIAN_POINT('Ctrl Pts',(97.0438942404132,-10.3351864930717,7.50991760330816));
#56574=CARTESIAN_POINT('Ctrl Pts',(97.1851696436624,-12.6521324429824,1.77159788043193));
#56575=CARTESIAN_POINT('Ctrl Pts',(97.3264450469117,-12.0003924020166,-4.38242112310514));
#56576=CARTESIAN_POINT('Ctrl Pts',(97.4677204501608,-8.53288737565654,-9.50814564449139));
#56577=CARTESIAN_POINT('Ctrl Pts',(97.6089958534101,-3.06323179364365,-12.4028881541422));
#56578=CARTESIAN_POINT('Ctrl Pts',(97.7502712566591,3.12517866436332,-12.387423856325));
#56579=CARTESIAN_POINT('Ctrl Pts',(97.8915466599084,8.58029918448171,-9.4653833698534));
#56580=CARTESIAN_POINT('Ctrl Pts',(98.0328220631576,12.0221440800517,-4.32239132243712));
#56581=CARTESIAN_POINT('Ctrl Pts',(98.1740974664068,12.6431210895909,1.83480358380842));
#56582=CARTESIAN_POINT('Ctrl Pts',(98.3153728696559,10.2975246168824,7.56148147672324));
#56583=CARTESIAN_POINT('Ctrl Pts',(98.4566482729052,5.53572383594821,11.5139383670531));
#56584=CARTESIAN_POINT('Ctrl Pts',(98.5979236761543,-0.524975488312981,
12.7647724614247));
#56585=CARTESIAN_POINT('Ctrl Pts',(98.7391990794036,-6.46249491565236,11.0204888572779));
#56586=CARTESIAN_POINT('Ctrl Pts',(98.8804744826528,-10.8836588489127,6.69036510749853));
#56587=CARTESIAN_POINT('Ctrl Pts',(99.0217498859019,-12.7510883346818,0.790418552611623));
#56588=CARTESIAN_POINT('Ctrl Pts',(99.1630252891511,-11.626610964448,-5.2949912829611));
#56589=CARTESIAN_POINT('Ctrl Pts',(99.3043006924003,-7.77407335801136,-10.1379878985948));
#56590=CARTESIAN_POINT('Ctrl Pts',(99.4455760956495,-2.09743236778966,-12.6022138003064));
#56591=CARTESIAN_POINT('Ctrl Pts',(99.5868514988987,4.07134875321906,-12.1094646676313));
#56592=CARTESIAN_POINT('Ctrl Pts',(99.7281269021479,9.28483132028813,-8.77535882801427));
#56593=CARTESIAN_POINT('Ctrl Pts',(99.8694023053971,12.3197272637194,-3.38220865031525));
#56594=CARTESIAN_POINT('Ctrl Pts',(100.010677708646,12.4639306250573,2.80454070757788));
#56595=CARTESIAN_POINT('Ctrl Pts',(100.151953111896,9.68360562384654,8.33323450578991));
#56596=CARTESIAN_POINT('Ctrl Pts',(100.293228515145,4.63112586258534,11.9066237217606));
#56597=CARTESIAN_POINT('Ctrl Pts',(100.434503918394,-1.50799817992959,12.6862506949854));
#56598=CARTESIAN_POINT('Ctrl Pts',(100.575779321643,-7.29328653605122,10.4891842728473));
#56599=CARTESIAN_POINT('Ctrl Pts',(100.717054724892,-11.3672830074131,5.83094265415717));
#56600=CARTESIAN_POINT('Ctrl Pts',(100.858330128141,-12.7740677812503,-0.195467456917545));
#56601=CARTESIAN_POINT('Ctrl Pts',(100.999605531391,-11.1835538172183,-6.1760132143701));
#56602=CARTESIAN_POINT('Ctrl Pts',(101.14088093464,-6.96893825021501,-10.7074233535142));
#56603=CARTESIAN_POINT('Ctrl Pts',(101.282156337889,-1.11913566374736,-12.7264508238872));
#56604=CARTESIAN_POINT('Ctrl Pts',(101.423431741138,4.99326016787109,-11.7593523674837));
#56605=CARTESIAN_POINT('Ctrl Pts',(101.564707144387,9.93404076655794,-8.03304732060357));
#56606=CARTESIAN_POINT('Ctrl Pts',(101.705982547637,12.5439046704665,-2.42187341224537));
#56607=CARTESIAN_POINT('Ctrl Pts',(101.847257950886,12.2104751551927,3.75756725703116));
#56608=CARTESIAN_POINT('Ctrl Pts',(101.988533354135,9.01198789964593,9.0553348531861));
#56609=CARTESIAN_POINT('Ctrl Pts',(102.129808757384,3.6989338185692,12.2283647235653));
#56610=CARTESIAN_POINT('Ctrl Pts',(102.271084160633,-2.48203562476454,12.5321392572893));
#56611=CARTESIAN_POINT('Ctrl Pts',(102.412359563882,-8.08062188579097,9.89538100052581));
#56612=CARTESIAN_POINT('Ctrl Pts',(102.553634967132,-11.7831764211184,4.93677715068152));
#56613=CARTESIAN_POINT('Ctrl Pts',(102.694910370381,-12.7209343059263,-1.18018879464178));
#56614=CARTESIAN_POINT('Ctrl Pts',(102.83618577363,-10.6738606560499,-7.02023602893248));
#56615=CARTESIAN_POINT('Ctrl Pts',(102.977461176879,-6.12227946633329,-11.2130597672002));
#56616=CARTESIAN_POINT('Ctrl Pts',(103.118736580128,-0.134170709081827,
-12.7748586460875));
#56617=CARTESIAN_POINT('Ctrl Pts',(103.260011983378,5.88541977379334,-11.3391732191078));
#56618=CARTESIAN_POINT('Ctrl Pts',(103.401287386627,10.5240592892947,-7.24287175656932));
#56619=CARTESIAN_POINT('Ctrl Pts',(103.542562789876,12.6933405576622,-1.44710769947736));
#56620=CARTESIAN_POINT('Ctrl Pts',(103.683838193125,11.8842648700219,4.68820474231524));
#56621=CARTESIAN_POINT('Ctrl Pts',(103.825113596374,8.28667320568124,9.72347995261696));
#56622=CARTESIAN_POINT('Ctrl Pts',(103.966388999624,2.7447020714836,12.4772443169718));
#56623=CARTESIAN_POINT('Ctrl Pts',(104.107664402873,-3.44128412477325,12.3033564030119));
#56624=CARTESIAN_POINT('Ctrl Pts',(104.248939806122,-8.81980971091815,9.24261715475003));
#56625=CARTESIAN_POINT('Ctrl Pts',(104.390215209371,-12.1288610335325,4.01319638655437));
#56626=CARTESIAN_POINT('Ctrl Pts',(104.53149061262,-12.5920044987599,-2.15787810324605));
#56627=CARTESIAN_POINT('Ctrl Pts',(104.672766015869,-10.1005684335019,-7.82262951489559));
#56628=CARTESIAN_POINT('Ctrl Pts',(104.814041419119,-5.23914173221625,-11.6518843592313));
#56629=CARTESIAN_POINT('Ctrl Pts',(104.955316822368,0.851593686827586,-12.747148833397));
#56630=CARTESIAN_POINT('Ctrl Pts',(105.096592225617,6.74251173434216,-10.8514308166036));
#56631=CARTESIAN_POINT('Ctrl Pts',(105.237867628866,11.0513713232499,-6.40954030986884));
#56632=CARTESIAN_POINT('Ctrl Pts',(105.379143032115,12.7671445332022,-0.46371955582386));
#56633=CARTESIAN_POINT('Ctrl Pts',(105.520418435365,11.4872434468854,5.59090807196851));
#56634=CARTESIAN_POINT('Ctrl Pts',(105.661693838614,7.51198327704425,10.333688705937));
#56635=CARTESIAN_POINT('Ctrl Pts',(105.802969241863,1.77411625795274,12.6517796351653));
#56636=CARTESIAN_POINT('Ctrl Pts',(105.944244645112,-4.38002799254061,12.0012651943452));
#56637=CARTESIAN_POINT('Ctrl Pts',(106.085520048361,-9.50644586328202,8.53478240110655));
#56638=CARTESIAN_POINT('Ctrl Pts',(106.226795451611,-12.4022766536811,3.0657029158183));
#56639=CARTESIAN_POINT('Ctrl Pts',(106.36807085486,-12.3880475449599,-3.12270887634921));
#56640=CARTESIAN_POINT('Ctrl Pts',(106.509346258109,-9.46709102841112,-8.5784148806465));
#56641=CARTESIAN_POINT('Ctrl Pts',(106.650621661358,-4.32479134103899,-12.0212778901215));
#56642=CARTESIAN_POINT('Ctrl Pts',(106.791897064607,1.83229272286617,-12.6434959689111));
#56643=CARTESIAN_POINT('Ctrl Pts',(106.933172467857,7.559410889752,-10.2990115858828));
#56644=CARTESIAN_POINT('Ctrl Pts',(107.074447871106,11.5128729878322,-5.53805945199291));
#56645=CARTESIAN_POINT('Ctrl Pts',(107.215723274355,12.7647975799994,0.522516840056443));
#56646=CARTESIAN_POINT('Ctrl Pts',(107.356998677604,11.0219419173116,6.46011445048516));
#56647=CARTESIAN_POINT('Ctrl Pts',(107.498274080853,6.69218539563937,10.8826582787472));
#56648=CARTESIAN_POINT('Ctrl Pts',(107.592457683019,2.7599182032822,12.1270516771658));
#56649=CARTESIAN_POINT('Ctrl Pts',(107.639549484103,0.761888816986977,12.2513058799703));
#56650=CARTESIAN_POINT('Ctrl Pts',(96.2504957088345,7.31062327544942,-9.43558181381351));
#56651=CARTESIAN_POINT('Ctrl Pts',(96.2975875099175,8.84944451830277,-8.24331379931861));
#56652=CARTESIAN_POINT('Ctrl Pts',(96.3917711120837,11.3313255199374,-5.09279394625159));
#56653=CARTESIAN_POINT('Ctrl Pts',(96.5330465153328,12.3953219151609,0.830806907182416));
#56654=CARTESIAN_POINT('Ctrl Pts',(96.674321918582,10.5507157326577,6.55847665225147));
#56655=CARTESIAN_POINT('Ctrl Pts',(96.8155973218312,6.23056735924752,10.7477596247075));
#56656=CARTESIAN_POINT('Ctrl Pts',(96.9568727250804,0.448447482651565,12.4149626160218));
#56657=CARTESIAN_POINT('Ctrl Pts',(97.0981481283296,-5.43887895542757,11.1692390058848));
#56658=CARTESIAN_POINT('Ctrl Pts',(97.2394235315788,-10.0500385694113,7.30271888339345));
#56659=CARTESIAN_POINT('Ctrl Pts',(97.3806989348279,-12.3030599517979,1.72271947291551));
#56660=CARTESIAN_POINT('Ctrl Pts',(97.5219743380772,-11.669301426654,-4.26151006990871));
#56661=CARTESIAN_POINT('Ctrl Pts',(97.6632497413264,-8.29746490702205,-9.24581578811144));
#56662=CARTESIAN_POINT('Ctrl Pts',(97.8045251445756,-2.97871719042544,-12.0606923159813));
#56663=CARTESIAN_POINT('Ctrl Pts',(97.9458005478247,3.03895494621288,-12.0456546783329));
#56664=CARTESIAN_POINT('Ctrl Pts',(98.087075951074,8.3435686234531,-9.20423332516161));
#56665=CARTESIAN_POINT('Ctrl Pts',(98.2283513543231,11.6904529756221,-4.2031364921864));
#56666=CARTESIAN_POINT('Ctrl Pts',(98.3696267575724,12.2942972217584,1.78418133015115));
#56667=CARTESIAN_POINT('Ctrl Pts',(98.5109021608215,10.0134157848537,7.35286010890084));
#56668=CARTESIAN_POINT('Ctrl Pts',(98.6521775640708,5.38299314658557,11.1962686645548));
#56669=CARTESIAN_POINT('Ctrl Pts',(98.7934529673199,-0.510491408072604,
12.4125922307329));
#56670=CARTESIAN_POINT('Ctrl Pts',(98.9347283705691,-6.28419460069438,10.7164334328806));
#56671=CARTESIAN_POINT('Ctrl Pts',(99.0760037738183,-10.5833785661451,6.50577785111838));
#56672=CARTESIAN_POINT('Ctrl Pts',(99.2172791770675,-12.3992856492167,0.768610894931606));
#56673=CARTESIAN_POINT('Ctrl Pts',(99.3585545803167,-11.3058326235886,-5.14890240772422));
#56674=CARTESIAN_POINT('Ctrl Pts',(99.4998299835658,-7.55958657754477,-9.85828068660432));
#56675=CARTESIAN_POINT('Ctrl Pts',(99.641105386815,-2.03956418272164,-12.2545185650931));
#56676=CARTESIAN_POINT('Ctrl Pts',(99.7823807900642,3.95902019056991,-11.7753643871063));
#56677=CARTESIAN_POINT('Ctrl Pts',(99.9236561933134,9.02866270888552,-8.53324656899885));
#56678=CARTESIAN_POINT('Ctrl Pts',(100.064931596563,11.9798258355578,-3.28889347166121));
#56679=CARTESIAN_POINT('Ctrl Pts',(100.206206999812,12.120050624366,2.72716339463603));
#56680=CARTESIAN_POINT('Ctrl Pts',(100.347482403061,9.41643482445774,8.10332046231385));
#56681=CARTESIAN_POINT('Ctrl Pts',(100.48875780631,4.50335304253882,11.5781198254505));
#56682=CARTESIAN_POINT('Ctrl Pts',(100.630033209559,-1.46639249142279,12.3362368808045));
#56683=CARTESIAN_POINT('Ctrl Pts',(100.771308612809,-7.09206466997174,10.1997875485309));
#56684=CARTESIAN_POINT('Ctrl Pts',(100.912584016058,-11.053659528108,5.67006687393485));
#56685=CARTESIAN_POINT('Ctrl Pts',(101.053859419307,-12.4216310925691,-0.190074507354378));
#56686=CARTESIAN_POINT('Ctrl Pts',(101.195134822556,-10.8749994285517,-6.00561693310731));
#56687=CARTESIAN_POINT('Ctrl Pts',(101.336410225805,-6.77666515736867,-10.4120054102527));
#56688=CARTESIAN_POINT('Ctrl Pts',(101.477685629055,-1.08825869688992,-12.3753278876509));
#56689=CARTESIAN_POINT('Ctrl Pts',(101.618961032304,4.85549605784568,-11.4349116896665));
#56690=CARTESIAN_POINT('Ctrl Pts',(101.760236435553,9.65996045847248,-7.81141544529376));
#56691=CARTESIAN_POINT('Ctrl Pts',(101.901511838802,12.1978181848694,-2.35505389473272));
#56692=CARTESIAN_POINT('Ctrl Pts',(102.042787242051,11.8735879940617,3.65389592975758));
#56693=CARTESIAN_POINT('Ctrl Pts',(102.1840626453,8.76334704160629,8.80549805216015));
#56694=CARTESIAN_POINT('Ctrl Pts',(102.32533804855,3.59688018859073,11.8909839890208));
#56695=CARTESIAN_POINT('Ctrl Pts',(102.466613451799,-2.41355623106157,12.1863773795878));
#56696=CARTESIAN_POINT('Ctrl Pts',(102.607888855048,-7.85767742763701,9.62236731586513));
#56697=CARTESIAN_POINT('Ctrl Pts',(102.749164258297,-11.4580784373656,4.80057140780163));
#56698=CARTESIAN_POINT('Ctrl Pts',(102.890439661546,-12.369963570489,-1.14762737114499));
#56699=CARTESIAN_POINT('Ctrl Pts',(103.031715064796,-10.3793687080281,-6.82654762973446));
#56700=CARTESIAN_POINT('Ctrl Pts',(103.172990468045,-5.95336569984595,-10.9036913090074));
#56701=CARTESIAN_POINT('Ctrl Pts',(103.314265871294,-0.130468937552451,
-12.4224001374356));
#56702=CARTESIAN_POINT('Ctrl Pts',(103.455541274543,5.72304096916393,-11.026325289211));
#56703=CARTESIAN_POINT('Ctrl Pts',(103.596816677792,10.2337003628415,-7.04304083488165));
#56704=CARTESIAN_POINT('Ctrl Pts',(103.738092081042,12.3431311340821,-1.40718198008219));
#56705=CARTESIAN_POINT('Ctrl Pts',(103.879367484291,11.5563778547088,4.55885711526834));
#56706=CARTESIAN_POINT('Ctrl Pts',(104.02064288754,8.05804378905324,9.45520902000235));
#56707=CARTESIAN_POINT('Ctrl Pts',(104.161918290789,2.66897570725448,12.1329969913553));
#56708=CARTESIAN_POINT('Ctrl Pts',(104.303193694038,-3.34633905304549,11.9639066471004));
#56709=CARTESIAN_POINT('Ctrl Pts',(104.444469097287,-8.57647105149153,8.98761323269872));
#56710=CARTESIAN_POINT('Ctrl Pts',(104.585744500537,-11.7942256070314,3.90247224842346));
#56711=CARTESIAN_POINT('Ctrl Pts',(104.727019903786,-12.244590938303,-2.09834221958635));
#56712=CARTESIAN_POINT('Ctrl Pts',(104.868295307035,-9.82189362501795,-7.60680306945773));
#56713=CARTESIAN_POINT('Ctrl Pts',(105.009570710284,-5.0945937467778,-11.3304087250961));
#56714=CARTESIAN_POINT('Ctrl Pts',(105.150846113533,0.828098206435065,-12.3954548388212));
#56715=CARTESIAN_POINT('Ctrl Pts',(105.292121516783,6.55648575187998,-10.5520397056476));
#56716=CARTESIAN_POINT('Ctrl Pts',(105.433396920032,10.746463851233,-6.23270101314186));
#56717=CARTESIAN_POINT('Ctrl Pts',(105.574672323281,12.4148988570206,-0.450925527521354));
#56718=CARTESIAN_POINT('Ctrl Pts',(105.71594772653,11.1703102575659,5.43665484884896));
#56719=CARTESIAN_POINT('Ctrl Pts',(105.857223129779,7.30472756516552,10.0485821062422));
#56720=CARTESIAN_POINT('Ctrl Pts',(105.998498533029,1.72516836836926,12.3027168779528));
#56721=CARTESIAN_POINT('Ctrl Pts',(106.139773936278,-4.25918296584617,11.6701501386315));
#56722=CARTESIAN_POINT('Ctrl Pts',(106.281049339527,-9.24416290388675,8.29930764869637));
#56723=CARTESIAN_POINT('Ctrl Pts',(106.422324742776,-12.0600976868255,2.98112013430862));
#56724=CARTESIAN_POINT('Ctrl Pts',(106.563600146025,-12.0462611593905,-3.03655329968074));
#56725=CARTESIAN_POINT('Ctrl Pts',(106.704875549275,-9.20589386939853,-8.34173630758412));
#56726=CARTESIAN_POINT('Ctrl Pts',(106.846150952524,-4.20547029424524,-11.6896106838828));
#56727=CARTESIAN_POINT('Ctrl Pts',(106.987426355773,1.78173974389346,-12.2946617581534));
#56728=CARTESIAN_POINT('Ctrl Pts',(107.128701759022,7.35084664944984,-10.0148617283609));
#56729=CARTESIAN_POINT('Ctrl Pts',(107.269977162271,11.1952326791597,-5.38526432295461));
#56730=CARTESIAN_POINT('Ctrl Pts',(107.41125256552,12.4126166562858,0.508100593951989));
#56731=CARTESIAN_POINT('Ctrl Pts',(107.55252796877,10.7178464029699,6.2818798125907));
#56732=CARTESIAN_POINT('Ctrl Pts',(107.693803372019,6.5075479174868,10.5824056017229));
#56733=CARTESIAN_POINT('Ctrl Pts',(107.787986974185,2.68377202578785,11.7924661708293));
#56734=CARTESIAN_POINT('Ctrl Pts',(107.835078775268,0.740868295067057,11.9132921986358));
#56735=CARTESIAN_POINT('Ctrl Pts',(96.446025,7.1032002856509,-9.1678677603644));
#56736=CARTESIAN_POINT('Ctrl Pts',(96.4931168010831,8.59836083215431,-8.00942775025295));
#56737=CARTESIAN_POINT('Ctrl Pts',(96.5873004032492,11.0098238737483,-4.94829702622741));
#56738=CARTESIAN_POINT('Ctrl Pts',(96.7285758064984,12.0436316920041,0.807234573314296));
#56739=CARTESIAN_POINT('Ctrl Pts',(96.8698512097476,10.2513621865474,6.37239418233372));
#56740=CARTESIAN_POINT('Ctrl Pts',(97.0111266129968,6.05378860029595,10.4428153879447));
#56741=CARTESIAN_POINT('Ctrl Pts',(97.152402016246,0.435723763467222,12.0627151308176));
#56742=CARTESIAN_POINT('Ctrl Pts',(97.2936774194952,-5.28456262813498,10.8523362109951));
#56743=CARTESIAN_POINT('Ctrl Pts',(97.4349528227444,-9.76489064575089,7.09552016347875));
#56744=CARTESIAN_POINT('Ctrl Pts',(97.5762282259935,-11.9539874606134,1.6738410653991));
#56745=CARTESIAN_POINT('Ctrl Pts',(97.7175036292427,-11.3382104512914,-4.14059901671228));
#56746=CARTESIAN_POINT('Ctrl Pts',(97.8587790324919,-8.06204243838756,-8.9834859317315));
#56747=CARTESIAN_POINT('Ctrl Pts',(98.0000544357412,-2.89420258720722,-11.7184964778204));
#56748=CARTESIAN_POINT('Ctrl Pts',(98.1413298389903,2.95273122806244,-11.7038855003407));
#56749=CARTESIAN_POINT('Ctrl Pts',(98.2826052422396,8.10683806242452,-8.94308328046984));
#56750=CARTESIAN_POINT('Ctrl Pts',(98.4238806454887,11.3587618711925,-4.08388166193566));
#56751=CARTESIAN_POINT('Ctrl Pts',(98.5651560487379,11.9454733539258,1.73355907649387));
#56752=CARTESIAN_POINT('Ctrl Pts',(98.706431451987,9.7293069528249,7.14423874107845));
#56753=CARTESIAN_POINT('Ctrl Pts',(98.8477068552363,5.23026245722293,10.8785989620564));
#56754=CARTESIAN_POINT('Ctrl Pts',(98.9889822584854,-0.496007327832227,
12.0604120000411));
#56755=CARTESIAN_POINT('Ctrl Pts',(99.1302576617347,-6.10589428573641,10.4123780084834));
#56756=CARTESIAN_POINT('Ctrl Pts',(99.2715330649838,-10.2830982833774,6.32119059473821));
#56757=CARTESIAN_POINT('Ctrl Pts',(99.412808468233,-12.0474829637517,0.746803237251589));
#56758=CARTESIAN_POINT('Ctrl Pts',(99.5540838714822,-10.9850542827293,-5.00281353248734));
#56759=CARTESIAN_POINT('Ctrl Pts',(99.6953592747313,-7.34509979707817,-9.57857347461386));
#56760=CARTESIAN_POINT('Ctrl Pts',(99.8366346779806,-1.98169599765362,-11.9068233298798));
#56761=CARTESIAN_POINT('Ctrl Pts',(99.9779100812298,3.84669162792076,-11.4412641065812));
#56762=CARTESIAN_POINT('Ctrl Pts',(100.119185484479,8.77249409748291,-8.29113430998339));
#56763=CARTESIAN_POINT('Ctrl Pts',(100.260460887728,11.6399244073961,-3.19557829300717));
#56764=CARTESIAN_POINT('Ctrl Pts',(100.401736290977,11.7761706236747,2.64978608169418));
#56765=CARTESIAN_POINT('Ctrl Pts',(100.543011694227,9.14926402506894,7.8734064188378));
#56766=CARTESIAN_POINT('Ctrl Pts',(100.684287097476,4.37558022249231,11.2496159291403));
#56767=CARTESIAN_POINT('Ctrl Pts',(100.825562500725,-1.42478680291599,11.9862230666236));
#56768=CARTESIAN_POINT('Ctrl Pts',(100.966837903974,-6.89084280389226,9.91039082421449));
#56769=CARTESIAN_POINT('Ctrl Pts',(101.108113307223,-10.7400360488029,5.50919109371254));
#56770=CARTESIAN_POINT('Ctrl Pts',(101.249388710472,-12.0691944038879,-0.18468155779121));
#56771=CARTESIAN_POINT('Ctrl Pts',(101.390664113722,-10.5664450398852,-5.83522065184453));
#56772=CARTESIAN_POINT('Ctrl Pts',(101.531939516971,-6.58439206452233,-10.1165874669912));
#56773=CARTESIAN_POINT('Ctrl Pts',(101.67321492022,-1.05738173003248,-12.0242049514145));
#56774=CARTESIAN_POINT('Ctrl Pts',(101.814490323469,4.71773194782029,-11.1104710118493));
#56775=CARTESIAN_POINT('Ctrl Pts',(101.955765726718,9.38588015038702,-7.58978356998396));
#56776=CARTESIAN_POINT('Ctrl Pts',(102.097041129968,11.8517316992723,-2.28823437722007));
#56777=CARTESIAN_POINT('Ctrl Pts',(102.238316533217,11.5367008329307,3.55022460248401));
#56778=CARTESIAN_POINT('Ctrl Pts',(102.379591936466,8.51470618356667,8.55566125113419));
#56779=CARTESIAN_POINT('Ctrl Pts',(102.520867339715,3.49482655861225,11.5536032544763));
#56780=CARTESIAN_POINT('Ctrl Pts',(102.662142742964,-2.34507683735861,11.8406155018864));
#56781=CARTESIAN_POINT('Ctrl Pts',(102.803418146214,-7.63473296948303,9.34935363120446));
#56782=CARTESIAN_POINT('Ctrl Pts',(102.944693549463,-11.1329804536129,4.66436566492173));
#56783=CARTESIAN_POINT('Ctrl Pts',(103.085968952712,-12.0189928350517,-1.1150659476482));
#56784=CARTESIAN_POINT('Ctrl Pts',(103.227244355961,-10.0848767600063,-6.63285923053644));
#56785=CARTESIAN_POINT('Ctrl Pts',(103.36851975921,-5.7844519333586,-10.5943228508145));
#56786=CARTESIAN_POINT('Ctrl Pts',(103.50979516246,-0.126767166023071,-12.0699416287838));
#56787=CARTESIAN_POINT('Ctrl Pts',(103.651070565709,5.56066216453452,-10.7134773593142));
#56788=CARTESIAN_POINT('Ctrl Pts',(103.792345968958,9.94334143638835,-6.84320991319397));
#56789=CARTESIAN_POINT('Ctrl Pts',(103.933621372207,11.992921710502,-1.36725626068703));
#56790=CARTESIAN_POINT('Ctrl Pts',(104.074896775456,11.2284908393957,4.42950948822145));
#56791=CARTESIAN_POINT('Ctrl Pts',(104.216172178705,7.82941437242525,9.18693808738774));
#56792=CARTESIAN_POINT('Ctrl Pts',(104.357447581955,2.59324934302537,11.7887496657387));
#56793=CARTESIAN_POINT('Ctrl Pts',(104.498722985204,-3.25139398131772,11.6244568911889));
#56794=CARTESIAN_POINT('Ctrl Pts',(104.639998388453,-8.33313239206491,8.73260931064738));
#56795=CARTESIAN_POINT('Ctrl Pts',(104.781273791702,-11.4595901805303,3.79174811029255));
#56796=CARTESIAN_POINT('Ctrl Pts',(104.922549194952,-11.8971773778461,-2.03880633592666));
#56797=CARTESIAN_POINT('Ctrl Pts',(105.063824598201,-9.54321881653396,-7.39097662401987));
#56798=CARTESIAN_POINT('Ctrl Pts',(105.20510000145,-4.95004576133935,-11.0089330909609));
#56799=CARTESIAN_POINT('Ctrl Pts',(105.346375404699,0.80460272604254,-12.0437608442455));
#56800=CARTESIAN_POINT('Ctrl Pts',(105.487650807948,6.3704597694178,-10.2526485946914));
#56801=CARTESIAN_POINT('Ctrl Pts',(105.628926211197,10.4415563792162,-6.05586171641488));
#56802=CARTESIAN_POINT('Ctrl Pts',(105.770201614447,12.062653180839,-0.438131499218847));
#56803=CARTESIAN_POINT('Ctrl Pts',(105.911477017696,10.8533770682464,5.28240162572942));
#56804=CARTESIAN_POINT('Ctrl Pts',(106.052752420945,7.09747185328678,9.76347550654746));
#56805=CARTESIAN_POINT('Ctrl Pts',(106.194027824194,1.67622047878578,11.9536541207404));
#56806=CARTESIAN_POINT('Ctrl Pts',(106.335303227443,-4.13833793915172,11.3390350829177));
#56807=CARTESIAN_POINT('Ctrl Pts',(106.476578630693,-8.98187994449148,8.0638328962862));
#56808=CARTESIAN_POINT('Ctrl Pts',(106.617854033942,-11.7179187199699,2.89653735279891));
#56809=CARTESIAN_POINT('Ctrl Pts',(106.759129437191,-11.7044747738212,-2.95039772301226));
#56810=CARTESIAN_POINT('Ctrl Pts',(106.90040484044,-8.94469671038593,-8.10505773452174));
#56811=CARTESIAN_POINT('Ctrl Pts',(107.041680243689,-4.08614924745149,-11.3579434776441));
#56812=CARTESIAN_POINT('Ctrl Pts',(107.182955646938,1.73118676492076,-11.9458275473958));
#56813=CARTESIAN_POINT('Ctrl Pts',(107.324231050188,7.14228240914768,-9.73071187083892));
#56814=CARTESIAN_POINT('Ctrl Pts',(107.465506453437,10.8775923704873,-5.2324691939163));
#56815=CARTESIAN_POINT('Ctrl Pts',(107.606781856686,12.0604357325722,0.493684347847536));
#56816=CARTESIAN_POINT('Ctrl Pts',(107.748057259935,10.4137508886283,6.10364517469624));
#56817=CARTESIAN_POINT('Ctrl Pts',(107.889332663184,6.32291043933424,10.2821529246985));
#56818=CARTESIAN_POINT('Ctrl Pts',(107.983516265351,2.6076258482935,11.4578806644928));
#56819=CARTESIAN_POINT('Ctrl Pts',(108.030608066434,0.719847773147138,11.5752785173012));
#56820=CARTESIAN_POINT('',(97.5221720974271,1.68935314531923,-12.5));
#56821=CARTESIAN_POINT('',(97.4445933434715,-1.68935314531933,-12.5));
#56822=CARTESIAN_POINT('Ctrl Pts',(97.5221720974271,1.68964825725037,-12.4999689146901));
#56823=CARTESIAN_POINT('Ctrl Pts',(97.5226740025917,1.68046138054838,-12.4999601656737));
#56824=CARTESIAN_POINT('Ctrl Pts',(97.5231701738963,1.67127418506373,-12.4999514312872));
#56825=CARTESIAN_POINT('Ctrl Pts',(97.5236606069647,1.66208665598902,-12.499942714296));
#56826=CARTESIAN_POINT('Ctrl Pts',(97.5368990767983,1.41408374930089,-12.4997074128196));
#56827=CARTESIAN_POINT('Ctrl Pts',(97.5459385014033,1.16616936498662,-12.4994871938956));
#56828=CARTESIAN_POINT('Ctrl Pts',(97.5507275875153,0.918043487166526,-12.4993243210419));
#56829=CARTESIAN_POINT('Ctrl Pts',(97.5528264032038,0.809302388574192,-12.499252942058));
#56830=CARTESIAN_POINT('Ctrl Pts',(97.554108886876,0.700520005736422,-12.4991923547014));
#56831=CARTESIAN_POINT('Ctrl Pts',(97.5545707211021,0.591668272259118,-12.4991447798153));
#56832=CARTESIAN_POINT('Ctrl Pts',(97.5553237021087,0.414194877627063,-12.4990672130529));
#56833=CARTESIAN_POINT('Ctrl Pts',(97.5538941469657,0.236797874895364,-12.4990245774829));
#56834=CARTESIAN_POINT('Ctrl Pts',(97.550282539358,0.0593580377332334,-12.4990206764826));
#56835=CARTESIAN_POINT('Ctrl Pts',(97.5500132405737,0.0461272724853178,
-12.4990203856053));
#56836=CARTESIAN_POINT('Ctrl Pts',(97.5497318203845,0.0328967901787399,
-12.4990203069961));
#56837=CARTESIAN_POINT('Ctrl Pts',(97.5494382818607,0.019666541528909,-12.499020440678));
#56838=CARTESIAN_POINT('Ctrl Pts',(97.5493576298141,0.0160314253716483,
-12.4990204774082));
#56839=CARTESIAN_POINT('Ctrl Pts',(97.5492760630078,0.0123963303202657,
-12.4990205301634));
#56840=CARTESIAN_POINT('Ctrl Pts',(97.5491935815112,0.00876125536962051,
-12.4990205989413));
#56841=CARTESIAN_POINT('Ctrl Pts',(97.5491451282504,0.00662585237640505,
-12.4990206393444));
#56842=CARTESIAN_POINT('Ctrl Pts',(97.5490963593478,0.00449045672313693,
-12.4990206852768));
#56843=CARTESIAN_POINT('Ctrl Pts',(97.5490472748175,0.00235506818888803,
-12.4990207367377));
#56844=CARTESIAN_POINT('Ctrl Pts',(97.54900489658,0.00051143228506254,-12.4990207811677));
#56845=CARTESIAN_POINT('Ctrl Pts',(97.5489622830749,-0.0013321980916125,
-12.4990208297187));
#56846=CARTESIAN_POINT('Ctrl Pts',(97.5489194343114,-0.00317582307487278,
-12.4990208823902));
#56847=CARTESIAN_POINT('Ctrl Pts',(97.5488672506322,-0.00542109520812969,
-12.4990209465366));
#56848=CARTESIAN_POINT('Ctrl Pts',(97.5488147180309,-0.00766635902086035,
-12.4990210167944));
#56849=CARTESIAN_POINT('Ctrl Pts',(97.5487618365246,-0.00991161475866892,
-12.4990210931625));
#56850=CARTESIAN_POINT('Ctrl Pts',(97.5486620680182,-0.0141476100486029,
-12.499021237242));
#56851=CARTESIAN_POINT('Ctrl Pts',(97.5485610576552,-0.0183835747721428,
-12.4990214030707));
#56852=CARTESIAN_POINT('Ctrl Pts',(97.5484588055552,-0.0226195105238446,
-12.4990215906396));
#56853=CARTESIAN_POINT('Ctrl Pts',(97.5478763735732,-0.0467475671134927,
-12.4990226590391));
#56854=CARTESIAN_POINT('Ctrl Pts',(97.54725365977,-0.0708744282519931,-12.4990244329689));
#56855=CARTESIAN_POINT('Ctrl Pts',(97.5465906887396,-0.0950003918469058,
-12.4990269093195));
#56856=CARTESIAN_POINT('Ctrl Pts',(97.5457430355439,-0.12584706418141,-12.4990300755009));
#56857=CARTESIAN_POINT('Ctrl Pts',(97.5448295947004,-0.156691459857992,
-12.4990343900702));
#56858=CARTESIAN_POINT('Ctrl Pts',(97.5438504280495,-0.187534199123077,
-12.4990398408432));
#56859=CARTESIAN_POINT('Ctrl Pts',(97.5390286321437,-0.33941579535519,-12.499066682561));
#56860=CARTESIAN_POINT('Ctrl Pts',(97.53261504854,-0.491193024837094,-12.4991213508053));
#56861=CARTESIAN_POINT('Ctrl Pts',(97.5246211743698,-0.642938406805146,
-12.4992001598446));
#56862=CARTESIAN_POINT('Ctrl Pts',(97.5119506489805,-0.883459294926447,
-12.4993250744869));
#56863=CARTESIAN_POINT('Ctrl Pts',(97.4953316149638,-1.12348158708097,-12.4995120880141));
#56864=CARTESIAN_POINT('Ctrl Pts',(97.4748532411262,-1.36327506627391,-12.4997267108814));
#56865=CARTESIAN_POINT('Ctrl Pts',(97.4655588277245,-1.47210888991352,-12.4998241206498));
#56866=CARTESIAN_POINT('Ctrl Pts',(97.4554694162836,-1.58089492867098,-12.4999269917156));
#56867=CARTESIAN_POINT('Ctrl Pts',(97.4445933434715,-1.68965488935079,-12.5000313373793));
#56868=CARTESIAN_POINT('',(99.2588790577572,-1.68935314531934,-12.5));
#56869=CARTESIAN_POINT('Ctrl Pts',(99.2588790577572,-1.68959457872525,-12.5008760874903));
#56870=CARTESIAN_POINT('Ctrl Pts',(99.2559349733328,-1.81702349400399,-12.483721099136));
#56871=CARTESIAN_POINT('Ctrl Pts',(99.2529908889084,-1.94418354975578,-12.4645915828494));
#56872=CARTESIAN_POINT('Ctrl Pts',(99.2500468044839,-2.07101417234007,-12.4434827001368));
#56873=CARTESIAN_POINT('Ctrl Pts',(99.2029550034009,-4.0997204147311,-12.1058377272082));
#56874=CARTESIAN_POINT('Ctrl Pts',(99.1558632023178,-6.04414027660449,-11.2617664188968));
#56875=CARTESIAN_POINT('Ctrl Pts',(99.1087714012347,-7.67615506867945,-10.0102949393431));
#56876=CARTESIAN_POINT('Ctrl Pts',(99.0616796001517,-9.30816986075441,-8.75882345978953));
#56877=CARTESIAN_POINT('Ctrl Pts',(99.0145877990686,-10.6277795830309,-7.09995180899373));
#56878=CARTESIAN_POINT('Ctrl Pts',(98.9674959979855,-11.4801680633091,-5.22829825551425));
#56879=CARTESIAN_POINT('Ctrl Pts',(98.9204041969025,-12.3325565435872,-3.35664470203477));
#56880=CARTESIAN_POINT('Ctrl Pts',(98.8733123958194,-12.7177237818671,-1.27220924587156));
#56881=CARTESIAN_POINT('Ctrl Pts',(98.8262205947364,-12.5904820862625,0.78046284114121));
#56882=CARTESIAN_POINT('Ctrl Pts',(98.7791287936533,-12.463240390658,2.83313492815398));
#56883=CARTESIAN_POINT('Ctrl Pts',(98.7320369925702,-11.8235897611692,4.85404364601633));
#56884=CARTESIAN_POINT('Ctrl Pts',(98.6849451914871,-10.7465737962464,6.60609665791358));
#56885=CARTESIAN_POINT('Ctrl Pts',(98.6378533904041,-9.66955783132365,8.35814966981085));
#56886=CARTESIAN_POINT('Ctrl Pts',(98.5907615893211,-8.15517653096699,9.84134697574299));
#56887=CARTESIAN_POINT('Ctrl Pts',(98.543669788238,-6.38109660377915,10.8816803637826));
#56888=CARTESIAN_POINT('Ctrl Pts',(98.496577987155,-4.60701667659133,11.9220137518223));
#56889=CARTESIAN_POINT('Ctrl Pts',(98.4494861860718,-2.57323812257234,12.5194832219694));
#56890=CARTESIAN_POINT('Ctrl Pts',(98.4023943849888,-0.518363163252151,
12.6039938532821));
#56891=CARTESIAN_POINT('Ctrl Pts',(98.3553025839057,1.53651179606804,12.6885044845949));
#56892=CARTESIAN_POINT('Ctrl Pts',(98.3082107828227,3.61248316068944,12.2600562770732));
#56893=CARTESIAN_POINT('Ctrl Pts',(98.2611189817396,5.4659986636002,11.3689146358113));
#56894=CARTESIAN_POINT('Ctrl Pts',(98.2140271806566,7.31951416651096,10.4777729945495));
#56895=CARTESIAN_POINT('Ctrl Pts',(98.1669353795735,8.95057380771109,9.12393791954758));
#56896=CARTESIAN_POINT('Ctrl Pts',(98.1198435784904,10.1678222130632,7.46624088086662));
#56897=CARTESIAN_POINT('Ctrl Pts',(98.0727517774073,11.3850706184153,5.80854384218565));
#56898=CARTESIAN_POINT('Ctrl Pts',(98.0256599763243,12.1885077879194,3.84698483982568));
#56899=CARTESIAN_POINT('Ctrl Pts',(97.9785681752412,12.4838747438477,1.81169334028676));
#56900=CARTESIAN_POINT('Ctrl Pts',(97.9314763741582,12.7792416997761,-0.22359815925215));
#56901=CARTESIAN_POINT('Ctrl Pts',(97.8843845730751,12.5665384421287,-2.33262215597));
#56902=CARTESIAN_POINT('Ctrl Pts',(97.837292771992,11.8707192401432,-4.26794869797181));
#56903=CARTESIAN_POINT('Ctrl Pts',(97.790200970909,11.1749000381577,-6.20327523997362));
#56904=CARTESIAN_POINT('Ctrl Pts',(97.7431091698259,9.99596489183397,-7.96490432725939));
#56905=CARTESIAN_POINT('Ctrl Pts',(97.6960173687429,8.47222609150605,-9.34616214086427));
#56906=CARTESIAN_POINT('Ctrl Pts',(97.6489255676598,6.94848729117811,-10.7274199544692));
#56907=CARTESIAN_POINT('Ctrl Pts',(97.6018337665767,5.07994483684591,-11.7283064943932));
#56908=CARTESIAN_POINT('Ctrl Pts',(97.5547419654936,3.08581547978386,-12.2313982573528));
#56909=CARTESIAN_POINT('Ctrl Pts',(97.5438853428048,2.62608555813135,-12.3473818749403));
#56910=CARTESIAN_POINT('Ctrl Pts',(97.5330287201159,2.15968075993868,-12.4369079670506));
#56911=CARTESIAN_POINT('Ctrl Pts',(97.5221720974271,1.68964825725054,-12.49996891469));
#56912=CARTESIAN_POINT('',(99.3364578117128,1.68935314531923,-12.5));
#56913=CARTESIAN_POINT('Ctrl Pts',(99.3364578117128,1.68942947079535,-12.4991898294055));
#56914=CARTESIAN_POINT('Ctrl Pts',(99.3369597168759,1.68024149022573,-12.4991852446615));
#56915=CARTESIAN_POINT('Ctrl Pts',(99.3374558881813,1.67105320856025,-12.4991807450271));
#56916=CARTESIAN_POINT('Ctrl Pts',(99.3379463212505,1.66186461098037,-12.4991763316958));
#56917=CARTESIAN_POINT('Ctrl Pts',(99.3511455436766,1.4145681889693,-12.499057553938));
#56918=CARTESIAN_POINT('Ctrl Pts',(99.3601705813528,1.16737258467869,-12.4990036489936));
#56919=CARTESIAN_POINT('Ctrl Pts',(99.3649705958634,0.919979347945403,-12.4990246557219));
#56920=CARTESIAN_POINT('Ctrl Pts',(99.3670947285812,0.810501331341849,-12.4990339517519));
#56921=CARTESIAN_POINT('Ctrl Pts',(99.3683914769703,0.700983945056015,-12.4990576754726));
#56922=CARTESIAN_POINT('Ctrl Pts',(99.3688564353878,0.591398452065715,-12.499095244472));
#56923=CARTESIAN_POINT('Ctrl Pts',(99.3696094163945,0.413929259729071,-12.4991560859192));
#56924=CARTESIAN_POINT('Ctrl Pts',(99.3681798612514,0.236542179380863,-12.4992533708621));
#56925=CARTESIAN_POINT('Ctrl Pts',(99.3645682536437,0.059117500948294,-12.499378606766));
#56926=CARTESIAN_POINT('Ctrl Pts',(99.3642989548594,0.0458878660039798,
-12.4993879449556));
#56927=CARTESIAN_POINT('Ctrl Pts',(99.3640175346701,0.0326585430731007,
-12.4993974350326));
#56928=CARTESIAN_POINT('Ctrl Pts',(99.3637239961464,0.019429482677277,-12.4994070719177));
#56929=CARTESIAN_POINT('Ctrl Pts',(99.3636433440999,0.015794693005883,-12.4994097197286));
#56930=CARTESIAN_POINT('Ctrl Pts',(99.3635617772938,0.0121599266192257,
-12.4994123786186));
#56931=CARTESIAN_POINT('Ctrl Pts',(99.3634792957969,0.00852518249016221,
-12.4994150484795));
#56932=CARTESIAN_POINT('Ctrl Pts',(99.3634308425361,0.00638997384311283,
-12.4994166168733));
#56933=CARTESIAN_POINT('Ctrl Pts',(99.3633820736336,0.00425477328640055,
-12.4994181890527));
#56934=CARTESIAN_POINT('Ctrl Pts',(99.3633329891032,0.00211958059809694,
-12.4994197649956));
#56935=CARTESIAN_POINT('Ctrl Pts',(99.3632906108658,0.000276113782411228,
-12.4994211256215));
#56936=CARTESIAN_POINT('Ctrl Pts',(99.3632479973606,-0.00156734694744143,
-12.4994224890525));
#56937=CARTESIAN_POINT('Ctrl Pts',(99.3632051485971,-0.00341080172588726,
-12.4994238552745));
#56938=CARTESIAN_POINT('Ctrl Pts',(99.363152964918,-0.00565586657044135,
-12.4994255191379));
#56939=CARTESIAN_POINT('Ctrl Pts',(99.3631004323168,-0.00790092226674584,
-12.4994271871404));
#56940=CARTESIAN_POINT('Ctrl Pts',(99.3630475508104,-0.0101459690715854,
-12.499428859256));
#56941=CARTESIAN_POINT('Ctrl Pts',(99.3629477823041,-0.0143815701593871,
-12.4994320139407));
#56942=CARTESIAN_POINT('Ctrl Pts',(99.3628467719413,-0.0186171377382284,
-12.4994351832643));
#56943=CARTESIAN_POINT('Ctrl Pts',(99.3627445198409,-0.0228526734316162,
-12.4994383670504));
#56944=CARTESIAN_POINT('Ctrl Pts',(99.3621620878589,-0.0469784511889833,
-12.4994565020208));
#56945=CARTESIAN_POINT('Ctrl Pts',(99.3615393740557,-0.0711029382673367,
-12.499475106215));
#56946=CARTESIAN_POINT('Ctrl Pts',(99.3608764030252,-0.0952264338341105,
-12.4994941456146));
#56947=CARTESIAN_POINT('Ctrl Pts',(99.360028749832,-0.126069950534176,-12.4995184887716));
#56948=CARTESIAN_POINT('Ctrl Pts',(99.3591153089914,-0.156911037043278,
-12.4995435429306));
#56949=CARTESIAN_POINT('Ctrl Pts',(99.3581361423438,-0.187750316250194,
-12.4995692314194));
#56950=CARTESIAN_POINT('Ctrl Pts',(99.3533143464512,-0.33961487391151,-12.4996957314896));
#56951=CARTESIAN_POINT('Ctrl Pts',(99.346900762868,-0.491371413732186,-12.4998378380961));
#56952=CARTESIAN_POINT('Ctrl Pts',(99.3389068887258,-0.643092774867443,
-12.4999842439063));
#56953=CARTESIAN_POINT('Ctrl Pts',(99.3262196286907,-0.88389320872154,-12.500216607908));
#56954=CARTESIAN_POINT('Ctrl Pts',(99.3095734231148,-1.12418542037101,-12.5004609712747));
#56955=CARTESIAN_POINT('Ctrl Pts',(99.2890577945819,-1.36424153814148,-12.5006536540262));
#56956=CARTESIAN_POINT('Ctrl Pts',(99.2797858146812,-1.47273421704968,-12.5007407364471));
#56957=CARTESIAN_POINT('Ctrl Pts',(99.2697234810396,-1.58117802058591,-12.5008170568316));
#56958=CARTESIAN_POINT('Ctrl Pts',(99.2588790577572,-1.68959457872552,-12.5008760874902));
#56959=CARTESIAN_POINT('',(101.073164772043,-1.68935314531934,-12.5));
#56960=CARTESIAN_POINT('Ctrl Pts',(101.073164772043,-1.68928079698559,-12.5007909894091));
#56961=CARTESIAN_POINT('Ctrl Pts',(101.030560395853,-3.53307800378901,-12.2502869163015));
#56962=CARTESIAN_POINT('Ctrl Pts',(100.987956019664,-5.32172987995247,-11.5875155537485));
#56963=CARTESIAN_POINT('Ctrl Pts',(100.945351643474,-6.88116103478917,-10.5725580738099));
#56964=CARTESIAN_POINT('Ctrl Pts',(100.898259842391,-8.60484363066917,-9.45069736306145));
#56965=CARTESIAN_POINT('Ctrl Pts',(100.851168041308,-10.048475918277,-7.89855342934716));
#56966=CARTESIAN_POINT('Ctrl Pts',(100.804076240225,-11.042691439422,-6.09822328096466));
#56967=CARTESIAN_POINT('Ctrl Pts',(100.756984439142,-12.036906960567,-4.29789313258215));
#56968=CARTESIAN_POINT('Ctrl Pts',(100.709892638059,-12.5817057152493,-2.24937676953143));
#56969=CARTESIAN_POINT('Ctrl Pts',(100.662800836976,-12.6131720953882,-0.193005447862708));
#56970=CARTESIAN_POINT('Ctrl Pts',(100.615709035893,-12.6446384755271,1.86336587380602));
#56971=CARTESIAN_POINT('Ctrl Pts',(100.56861723481,-12.1627724811226,3.92759215409274));
#56972=CARTESIAN_POINT('Ctrl Pts',(100.521525433727,-11.2241064698225,5.75749905470014));
#56973=CARTESIAN_POINT('Ctrl Pts',(100.474433632644,-10.2854404585223,7.58740595530752));
#56974=CARTESIAN_POINT('Ctrl Pts',(100.42734183156,-8.88997443032653,9.18299347623558));
#56975=CARTESIAN_POINT('Ctrl Pts',(100.380250030477,-7.20142399394626,10.3570678220334));
#56976=CARTESIAN_POINT('Ctrl Pts',(100.333158229394,-5.51287355756596,11.5311421678312));
#56977=CARTESIAN_POINT('Ctrl Pts',(100.286066428311,-3.53123871300118,12.2837033384987));
#56978=CARTESIAN_POINT('Ctrl Pts',(100.238974627228,-1.48900419887407,12.5264611086499));
#56979=CARTESIAN_POINT('Ctrl Pts',(100.191882826145,0.553230315253027,12.7692188788011));
#56980=CARTESIAN_POINT('Ctrl Pts',(100.144791025062,2.65606449894247,12.5021732484359));
#56981=CARTESIAN_POINT('Ctrl Pts',(100.097699223979,4.57279454755443,11.7566539217858));
#56982=CARTESIAN_POINT('Ctrl Pts',(100.050607422896,6.48952459616636,11.0111345951358));
#56983=CARTESIAN_POINT('Ctrl Pts',(100.003515621813,8.22015050970083,9.78714157220086));
#56984=CARTESIAN_POINT('Ctrl Pts',(99.9564238207299,9.56163583355362,8.22827330594238));
#56985=CARTESIAN_POINT('Ctrl Pts',(99.9093320196468,10.9031211574064,6.66940503968388));
#56986=CARTESIAN_POINT('Ctrl Pts',(99.8622402185638,11.8554658915775,4.7756615301018));
#56987=CARTESIAN_POINT('Ctrl Pts',(99.8151484174807,12.3069412696852,2.76921613372925));
#56988=CARTESIAN_POINT('Ctrl Pts',(99.7680566163977,12.7584166477928,0.762770737356701));
#56989=CARTESIAN_POINT('Ctrl Pts',(99.7209648153146,12.7090226698369,-1.35637654580632));
#56990=CARTESIAN_POINT('Ctrl Pts',(99.6738730142315,12.1645542208273,-3.33960806373124));
#56991=CARTESIAN_POINT('Ctrl Pts',(99.6267812131484,11.6200857718176,-5.32283958165613));
#56992=CARTESIAN_POINT('Ctrl Pts',(99.5796894120654,10.5805428517542,-7.17015533434292));
#56993=CARTESIAN_POINT('Ctrl Pts',(99.5325976109823,9.16788428908538,-8.66482885420743));
#56994=CARTESIAN_POINT('Ctrl Pts',(99.4855058098992,7.75522572641657,-10.1595023740719));
#56995=CARTESIAN_POINT('Ctrl Pts',(99.4384140088162,5.96945152114239,-11.3015336611142));
#56996=CARTESIAN_POINT('Ctrl Pts',(99.3913222077331,4.02006810705099,-11.9569399858625));
#56997=CARTESIAN_POINT('Ctrl Pts',(99.3730340757264,3.26302377260614,-12.2114674643069));
#56998=CARTESIAN_POINT('Ctrl Pts',(99.3547459437195,2.481304513322,-12.3926039982175));
#56999=CARTESIAN_POINT('Ctrl Pts',(99.3364578117128,1.68942947079438,-12.4991898294056));
#57000=CARTESIAN_POINT('',(101.150743525999,1.68935314531923,-12.5));
#57001=CARTESIAN_POINT('Ctrl Pts',(101.150743525999,1.68914515608837,-12.4990650577849));
#57002=CARTESIAN_POINT('Ctrl Pts',(101.151245431163,1.67995781277747,-12.4990674945739));
#57003=CARTESIAN_POINT('Ctrl Pts',(101.151741602468,1.67077018456029,-12.4990700270579));
#57004=CARTESIAN_POINT('Ctrl Pts',(101.152232035536,1.66158225640466,-12.4990726548156));
#57005=CARTESIAN_POINT('Ctrl Pts',(101.165379558313,1.41527240811885,-12.4991430997065));
#57006=CARTESIAN_POINT('Ctrl Pts',(101.174385531785,1.16907402877139,-12.4992842339152));
#57007=CARTESIAN_POINT('Ctrl Pts',(101.179199712583,0.92268867358122,-12.4994739647979));
#57008=CARTESIAN_POINT('Ctrl Pts',(101.181357422249,0.812259073004665,-12.4995590019364));
#57009=CARTESIAN_POINT('Ctrl Pts',(101.182673075835,0.701791239333902,-12.4996535375347));
#57010=CARTESIAN_POINT('Ctrl Pts',(101.183142149673,0.591255341135298,-12.4997539904862));
#57011=CARTESIAN_POINT('Ctrl Pts',(101.18389513068,0.413817536922243,-12.4999152426352));
#57012=CARTESIAN_POINT('Ctrl Pts',(101.182465575537,0.236465021036391,-12.5000917228813));
#57013=CARTESIAN_POINT('Ctrl Pts',(101.17885396793,0.0590766675822643,-12.5002625611583));
#57014=CARTESIAN_POINT('Ctrl Pts',(101.178584669145,0.0458497412066224,
-12.5002752996796));
#57015=CARTESIAN_POINT('Ctrl Pts',(101.178303248956,0.0326231365233512,
-12.5002880031159));
#57016=CARTESIAN_POINT('Ctrl Pts',(101.178009710432,0.0193968034520138,
-12.5003006612721));
#57017=CARTESIAN_POINT('Ctrl Pts',(101.177929058386,0.0157627631540866,
-12.5003041392013));
#57018=CARTESIAN_POINT('Ctrl Pts',(101.17784749158,0.012128746826254,-12.5003076137077));
#57019=CARTESIAN_POINT('Ctrl Pts',(101.177765010083,0.0084947533778412,
-12.5003110845771));
#57020=CARTESIAN_POINT('Ctrl Pts',(101.177716556821,0.00635998568360754,
-12.5003131235185));
#57021=CARTESIAN_POINT('Ctrl Pts',(101.177667787917,0.00422522631192673,
-12.5003151612044));
#57022=CARTESIAN_POINT('Ctrl Pts',(101.177618703389,0.00209047518892369,
-12.500317197591));
#57023=CARTESIAN_POINT('Ctrl Pts',(101.177576325151,0.000247389521649039,
-12.5003189557515));
#57024=CARTESIAN_POINT('Ctrl Pts',(101.177533711646,-0.00159568988858964,
-12.5003207129434));
#57025=CARTESIAN_POINT('Ctrl Pts',(101.177490862883,-0.00343876317675105,
-12.5003224691385));
#57026=CARTESIAN_POINT('Ctrl Pts',(101.177438679203,-0.00568336343521118,
-12.5003246079335));
#57027=CARTESIAN_POINT('Ctrl Pts',(101.177386146602,-0.00792795429388963,
-12.5003267452498));
#57028=CARTESIAN_POINT('Ctrl Pts',(101.177333265096,-0.0101725359711127,
-12.5003288810365));
#57029=CARTESIAN_POINT('Ctrl Pts',(101.177233496591,-0.0144072595541474,
-12.5003329105027));
#57030=CARTESIAN_POINT('Ctrl Pts',(101.177132486228,-0.0186419487436732,
-12.5003369345226));
#57031=CARTESIAN_POINT('Ctrl Pts',(101.177030234127,-0.0228766052639706,
-12.5003409527519));
#57032=CARTESIAN_POINT('Ctrl Pts',(101.176447802145,-0.0469973749059116,
-12.5003638407438));
#57033=CARTESIAN_POINT('Ctrl Pts',(101.175825088342,-0.07111682585345,-12.5003865408022));
#57034=CARTESIAN_POINT('Ctrl Pts',(101.175162117311,-0.0952352608502072,
-12.5004089879631));
#57035=CARTESIAN_POINT('Ctrl Pts',(101.174314464106,-0.12607230773492,-12.5004376881733));
#57036=CARTESIAN_POINT('Ctrl Pts',(101.173401023251,-0.156906884656046,
-12.5004659744033));
#57037=CARTESIAN_POINT('Ctrl Pts',(101.172421856587,-0.187739621969185,
-12.5004937054932));
#57038=CARTESIAN_POINT('Ctrl Pts',(101.16760006063,-0.339571964404762,-12.5006302641222));
#57039=CARTESIAN_POINT('Ctrl Pts',(101.161186476945,-0.491295520700995,
-12.5007535749172));
#57040=CARTESIAN_POINT('Ctrl Pts',(101.153192602665,-0.642984018431462,
-12.500844739625));
#57041=CARTESIAN_POINT('Ctrl Pts',(101.145167090904,-0.795272856108191,
-12.5009362651368));
#57042=CARTESIAN_POINT('Ctrl Pts',(101.13555745464,-0.947357522802301,-12.5009956204214));
#57043=CARTESIAN_POINT('Ctrl Pts',(101.124386353216,-1.09931002772209,-12.5010000674675));
#57044=CARTESIAN_POINT('Ctrl Pts',(101.109916044249,-1.29613929377952,-12.5010058278782));
#57045=CARTESIAN_POINT('Ctrl Pts',(101.092825767703,-1.49274779624088,-12.5009197918223));
#57046=CARTESIAN_POINT('Ctrl Pts',(101.073164772043,-1.68928079698559,-12.5007909894091));
#57047=CARTESIAN_POINT('',(102.887450486329,-1.68935314531934,-12.5));
#57048=CARTESIAN_POINT('Ctrl Pts',(102.887450486329,-1.68904238362358,-12.4999128886012));
#57049=CARTESIAN_POINT('Ctrl Pts',(102.852277619457,-3.21148927825508,-12.2926905183232));
#57050=CARTESIAN_POINT('Ctrl Pts',(102.817104752585,-4.69695204398918,-11.8079445987757));
#57051=CARTESIAN_POINT('Ctrl Pts',(102.781931885714,-6.04516633599424,-11.071825747407));
#57052=CARTESIAN_POINT('Ctrl Pts',(102.734840084631,-7.85024635657098,-10.0862602929722));
#57053=CARTESIAN_POINT('Ctrl Pts',(102.687748283548,-9.40929948032132,-8.65009236055137));
#57054=CARTESIAN_POINT('Ctrl Pts',(102.640656482464,-10.5394181150785,-6.93181269267563));
#57055=CARTESIAN_POINT('Ctrl Pts',(102.593564681381,-11.6695367498357,-5.21353302479987));
#57056=CARTESIAN_POINT('Ctrl Pts',(102.546472880298,-12.3707208955997,-3.21314162146922));
#57057=CARTESIAN_POINT('Ctrl Pts',(102.499381079215,-12.5607078623996,-1.16532373452056));
#57058=CARTESIAN_POINT('Ctrl Pts',(102.452289278132,-12.7506948291995,0.882494152428101));
#57059=CARTESIAN_POINT('Ctrl Pts',(102.405197477049,-12.4294846170353,2.97773852299478));
#57060=CARTESIAN_POINT('Ctrl Pts',(102.358105675966,-11.6347615007988,4.8745960068823));
#57061=CARTESIAN_POINT('Ctrl Pts',(102.311013874883,-10.8400383845624,6.77145349076979));
#57062=CARTESIAN_POINT('Ctrl Pts',(102.2639220738,-9.57180236425365,8.46992408797814));
#57063=CARTESIAN_POINT('Ctrl Pts',(102.216830272717,-7.97884246651973,9.77074379488302));
#57064=CARTESIAN_POINT('Ctrl Pts',(102.169738471634,-6.3858825687858,11.0715635017879));
#57065=CARTESIAN_POINT('Ctrl Pts',(102.122646670551,-4.46819879362666,11.9747323183893));
#57066=CARTESIAN_POINT('Ctrl Pts',(102.075554869468,-2.45077316154458,12.3742907805432));
#57067=CARTESIAN_POINT('Ctrl Pts',(102.028463068385,-0.433347529462455,
12.7738492426971));
#57068=CARTESIAN_POINT('Ctrl Pts',(101.981371267302,1.68381995954259,12.6697973504035));
#57069=CARTESIAN_POINT('Ctrl Pts',(101.934279466219,3.65234392223479,12.0743424369403));
#57070=CARTESIAN_POINT('Ctrl Pts',(101.887187665135,5.62086788492697,11.4788875234772));
#57071=CARTESIAN_POINT('Ctrl Pts',(101.840095864052,7.44074832130627,10.3920295888446));
#57072=CARTESIAN_POINT('Ctrl Pts',(101.793004062969,8.89847746593561,8.94127844321045));
#57073=CARTESIAN_POINT('Ctrl Pts',(101.745912261886,10.3562066105649,7.49052729757627));
#57074=CARTESIAN_POINT('Ctrl Pts',(101.698820460803,11.4517844634443,5.6758829409405));
#57075=CARTESIAN_POINT('Ctrl Pts',(101.65172865972,12.0566781965073,3.71023884361215));
#57076=CARTESIAN_POINT('Ctrl Pts',(101.604636858637,12.6615719295703,1.74459474628381));
#57077=CARTESIAN_POINT('Ctrl Pts',(101.557545057554,12.7757815428169,-0.372049091737104));
#57078=CARTESIAN_POINT('Ctrl Pts',(101.510453256471,12.3859080025369,-2.39136872177345));
#57079=CARTESIAN_POINT('Ctrl Pts',(101.463361455388,11.9960344622568,-4.4106883518098));
#57080=CARTESIAN_POINT('Ctrl Pts',(101.416269654305,11.1020777684501,-6.33268377386159));
#57081=CARTESIAN_POINT('Ctrl Pts',(101.369177853222,9.80891662208894,-7.93186712645206));
#57082=CARTESIAN_POINT('Ctrl Pts',(101.322086052139,8.51575547572777,-9.53105047904253));
#57083=CARTESIAN_POINT('Ctrl Pts',(101.274994251056,6.82338987681213,-10.8074217621717));
#57084=CARTESIAN_POINT('Ctrl Pts',(101.227902449973,4.9303675926041,-11.6112375228734));
#57085=CARTESIAN_POINT('Ctrl Pts',(101.202182808648,3.89647521538113,-12.0502492527479));
#57086=CARTESIAN_POINT('Ctrl Pts',(101.176463167323,2.80272888387535,-12.3483022271529));
#57087=CARTESIAN_POINT('Ctrl Pts',(101.150743525999,1.68914515608859,-12.4990650577849));
#57088=CARTESIAN_POINT('',(102.965029240284,1.68935314531922,-12.5));
#57089=CARTESIAN_POINT('Ctrl Pts',(102.965029240284,1.68902555333161,-12.4996661638321));
#57090=CARTESIAN_POINT('Ctrl Pts',(102.965531145447,1.67984017954619,-12.4996740615437));
#57091=CARTESIAN_POINT('Ctrl Pts',(102.966027316753,1.67065452637564,-12.4996820065689));
#57092=CARTESIAN_POINT('Ctrl Pts',(102.966517749822,1.6614685785147,-12.4996899968223));
#57093=CARTESIAN_POINT('Ctrl Pts',(102.97959948863,1.41644397031431,-12.4999031276523));
#57094=CARTESIAN_POINT('Ctrl Pts',(102.988581019146,1.17153336884166,-12.5001505770197));
#57095=CARTESIAN_POINT('Ctrl Pts',(102.993412848414,0.926436831441823,-12.5003783882217));
#57096=CARTESIAN_POINT('Ctrl Pts',(102.995613656082,0.814799952495679,-12.5004821519544));
#57097=CARTESIAN_POINT('Ctrl Pts',(102.996953553553,0.703123817408969,-12.5005815543068));
#57098=CARTESIAN_POINT('Ctrl Pts',(102.997427863959,0.591377000343097,-12.5006697352989));
#57099=CARTESIAN_POINT('Ctrl Pts',(102.998180844966,0.413975809754343,-12.5008097250847));
#57100=CARTESIAN_POINT('Ctrl Pts',(102.996751289823,0.236657100233925,-12.5009214411543));
#57101=CARTESIAN_POINT('Ctrl Pts',(102.993139682215,0.059297357029078,-12.5009714974348));
#57102=CARTESIAN_POINT('Ctrl Pts',(102.992870383431,0.0460725639711593,
-12.5009752298711));
#57103=CARTESIAN_POINT('Ctrl Pts',(102.992588963242,0.0328480636202189,
-12.5009786160395));
#57104=CARTESIAN_POINT('Ctrl Pts',(102.992295424718,0.0196238049059938,
-12.5009816405923));
#57105=CARTESIAN_POINT('Ctrl Pts',(102.992214772671,0.0159903345173654,
-12.5009824716123));
#57106=CARTESIAN_POINT('Ctrl Pts',(102.992133205864,0.0123568858355826,
-12.5009832753311));
#57107=CARTESIAN_POINT('Ctrl Pts',(102.992050724368,0.00872345786128001,
-12.5009840514279));
#57108=CARTESIAN_POINT('Ctrl Pts',(102.992002271108,0.00658902237049392,
-12.5009845073413));
#57109=CARTESIAN_POINT('Ctrl Pts',(102.991953502206,0.00445459441415752,
-12.5009849537224));
#57110=CARTESIAN_POINT('Ctrl Pts',(102.991904417675,0.00232017372424163,
-12.5009853905061));
#57111=CARTESIAN_POINT('Ctrl Pts',(102.991862039437,0.00047737344895807,
-12.5009857676132));
#57112=CARTESIAN_POINT('Ctrl Pts',(102.991819425932,-0.00136542115994614,
-12.5009861375661));
#57113=CARTESIAN_POINT('Ctrl Pts',(102.991776577169,-0.00320821022753773,
-12.5009865003228));
#57114=CARTESIAN_POINT('Ctrl Pts',(102.991724393489,-0.00545246436304751,
-12.5009869421087));
#57115=CARTESIAN_POINT('Ctrl Pts',(102.991671860887,-0.00769670997883713,
-12.5009873732213));
#57116=CARTESIAN_POINT('Ctrl Pts',(102.991618979382,-0.00994094727719665,
-12.5009877935844));
#57117=CARTESIAN_POINT('Ctrl Pts',(102.991519210876,-0.0141750211869177,
-12.5009885866594));
#57118=CARTESIAN_POINT('Ctrl Pts',(102.991418200513,-0.0184090638530525,
-12.5009893414724));
#57119=CARTESIAN_POINT('Ctrl Pts',(102.991315948412,-0.0226430769711849,
-12.5009900575103));
#57120=CARTESIAN_POINT('Ctrl Pts',(102.990733516431,-0.0467601819948663,
-12.5009941360904));
#57121=CARTESIAN_POINT('Ctrl Pts',(102.990110802628,-0.070876071614745,
-12.5009969567622));
#57122=CARTESIAN_POINT('Ctrl Pts',(102.989447831597,-0.0949910545696576,
-12.5009984234356));
#57123=CARTESIAN_POINT('Ctrl Pts',(102.989115137014,-0.107092524834283,
-12.5009991594471));
#57124=CARTESIAN_POINT('Ctrl Pts',(102.988772307999,-0.119193642114226,
-12.5009995544426));
#57125=CARTESIAN_POINT('Ctrl Pts',(102.98841934829,-0.131294445324536,-12.5009995960793));
#57126=CARTESIAN_POINT('Ctrl Pts',(102.98787302245,-0.15002457604026,-12.5009996605264));
#57127=CARTESIAN_POINT('Ctrl Pts',(102.987302425348,-0.168753954322204,
-12.5009988784369));
#57128=CARTESIAN_POINT('Ctrl Pts',(102.986707570848,-0.187482725158803,
-12.5009972959589));
#57129=CARTESIAN_POINT('Ctrl Pts',(102.981885774851,-0.33929516374844,-12.5009844686436));
#57130=CARTESIAN_POINT('Ctrl Pts',(102.975472191106,-0.491003527350138,
-12.5009193887239));
#57131=CARTESIAN_POINT('Ctrl Pts',(102.967478316743,-0.642683527375726,
-12.5008245034654));
#57132=CARTESIAN_POINT('Ctrl Pts',(102.954945096181,-0.880495483007408,
-12.5006757373205));
#57133=CARTESIAN_POINT('Ctrl Pts',(102.938548479827,-1.11782828523526,-12.5004559196816));
#57134=CARTESIAN_POINT('Ctrl Pts',(102.91837476894,-1.35495512994139,-12.5002302445128));
#57135=CARTESIAN_POINT('Ctrl Pts',(102.908897314919,-1.46635549550954,-12.5001242240564));
#57136=CARTESIAN_POINT('Ctrl Pts',(102.898586237988,-1.57770974440371,-12.5000166025227));
#57137=CARTESIAN_POINT('Ctrl Pts',(102.887450486329,-1.68904238362393,-12.4999128886011));
#57138=CARTESIAN_POINT('',(104.701736200614,-1.68935314531934,-12.5));
#57139=CARTESIAN_POINT('Ctrl Pts',(104.701736200614,-1.68908803070059,-12.4991653468105));
#57140=CARTESIAN_POINT('Ctrl Pts',(104.673994843061,-2.89014759230633,-12.336307880009));
#57141=CARTESIAN_POINT('Ctrl Pts',(104.646253485507,-4.0681811144386,-12.0019612113943));
#57142=CARTESIAN_POINT('Ctrl Pts',(104.618512127953,-5.17315215756407,-11.5051231269621));
#57143=CARTESIAN_POINT('Ctrl Pts',(104.57142032687,-7.04887422576513,-10.6617253156888));
#57144=CARTESIAN_POINT('Ctrl Pts',(104.524328525787,-8.71405873387556,-9.35009063801111));
#57145=CARTESIAN_POINT('Ctrl Pts',(104.477236724704,-9.97334679080258,-7.72409963693427));
#57146=CARTESIAN_POINT('Ctrl Pts',(104.430144923621,-11.2326348477296,-6.09810863585747));
#57147=CARTESIAN_POINT('Ctrl Pts',(104.383053122538,-12.0860264534732,-4.15776131138159));
#57148=CARTESIAN_POINT('Ctrl Pts',(104.335961321455,-12.4334019898144,-2.13069856387849));
#57149=CARTESIAN_POINT('Ctrl Pts',(104.288869520372,-12.7807775261557,-0.103635816375385));
#57150=CARTESIAN_POINT('Ctrl Pts',(104.241777719289,-12.6221369930946,2.01014235415493));
#57151=CARTESIAN_POINT('Ctrl Pts',(104.194685918206,-11.9760920449493,3.9626481981061));
#57152=CARTESIAN_POINT('Ctrl Pts',(104.147594117122,-11.330047096804,5.9151540420573));
#57153=CARTESIAN_POINT('Ctrl Pts',(104.100502316039,-10.1965977335744,7.70638755942933));
#57154=CARTESIAN_POINT('Ctrl Pts',(104.053410514956,-8.70871985631894,9.12620183180236));
#57155=CARTESIAN_POINT('Ctrl Pts',(104.006318713873,-7.2208419790635,10.5460161041754));
#57156=CARTESIAN_POINT('Ctrl Pts',(103.95922691279,-5.37853558778224,11.5944111315494));
#57157=CARTESIAN_POINT('Ctrl Pts',(103.912135111707,-3.39793945343931,12.1483895591806));
#57158=CARTESIAN_POINT('Ctrl Pts',(103.865043310624,-1.41734331909643,12.7023679868117));
#57159=CARTESIAN_POINT('Ctrl Pts',(103.817951509541,0.701542558308156,12.7619298147));
#57160=CARTESIAN_POINT('Ctrl Pts',(103.770859708458,2.71013119477651,12.3200872690847));
#57161=CARTESIAN_POINT('Ctrl Pts',(103.723767907375,4.71871983124487,11.8782447234694));
#57162=CARTESIAN_POINT('Ctrl Pts',(103.676676106292,6.61701122677704,10.9349978043505));
#57163=CARTESIAN_POINT('Ctrl Pts',(103.629584305209,8.18229846838074,9.60100792547948));
#57164=CARTESIAN_POINT('Ctrl Pts',(103.582492504126,9.74758570998446,8.26701804660844));
#57165=CARTESIAN_POINT('Ctrl Pts',(103.535400703043,10.9798687976597,6.54228520798529));
#57166=CARTESIAN_POINT('Ctrl Pts',(103.48830890196,11.7345766908152,4.62915449063459));
#57167=CARTESIAN_POINT('Ctrl Pts',(103.441217100877,12.4892845839708,2.7160237732839));
#57168=CARTESIAN_POINT('Ctrl Pts',(103.394125299794,12.7664172826066,0.61449517720567));
#57169=CARTESIAN_POINT('Ctrl Pts',(103.34703349871,12.5334616710087,-1.4288806640642));
#57170=CARTESIAN_POINT('Ctrl Pts',(103.299941697627,12.3005060594108,-3.47225650533403));
#57171=CARTESIAN_POINT('Ctrl Pts',(103.252849896544,11.5574621375793,-5.4574795917955));
#57172=CARTESIAN_POINT('Ctrl Pts',(103.205758095461,10.3915035704427,-7.15164421348415));
#57173=CARTESIAN_POINT('Ctrl Pts',(103.158666294378,9.22554500330613,-8.84580883517282));
#57174=CARTESIAN_POINT('Ctrl Pts',(103.111574493295,7.63667179086451,-10.2489149920886));
#57175=CARTESIAN_POINT('Ctrl Pts',(103.064482692212,5.81129000813801,-11.196350738169));
#57176=CARTESIAN_POINT('Ctrl Pts',(103.031331541569,4.52627849726565,-11.8633157813431));
#57177=CARTESIAN_POINT('Ctrl Pts',(102.998180390927,3.12406000128176,-12.3044634049023));
#57178=CARTESIAN_POINT('Ctrl Pts',(102.965029240284,1.68902555333143,-12.4996661638321));
#57179=CARTESIAN_POINT('',(104.77931495457,1.68935314531922,-12.5));
#57180=CARTESIAN_POINT('Ctrl Pts',(104.77931495457,1.68919355642484,-12.5005864930275));
#57181=CARTESIAN_POINT('Ctrl Pts',(104.779816859733,1.68001010168838,-12.5005940984057));
#57182=CARTESIAN_POINT('Ctrl Pts',(104.780313031038,1.67082635357051,-12.5006016453638));
#57183=CARTESIAN_POINT('Ctrl Pts',(104.780803464108,1.66164229630986,-12.5006091300974));
#57184=CARTESIAN_POINT('Ctrl Pts',(104.793749705728,1.41920549540073,-12.5008067088801));
#57185=CARTESIAN_POINT('Ctrl Pts',(104.802680236919,1.17687017443894,-12.5009631542608));
#57186=CARTESIAN_POINT('Ctrl Pts',(104.807547086755,0.93433729498524,-12.5009942749996));
#57187=CARTESIAN_POINT('Ctrl Pts',(104.80821046687,0.901278644165153,-12.5009985169384));
#57188=CARTESIAN_POINT('Ctrl Pts',(104.808798346689,0.868216252236512,-12.5010003947653));
#57189=CARTESIAN_POINT('Ctrl Pts',(104.809310604728,0.835149297560743,-12.500999658972));
#57190=CARTESIAN_POINT('Ctrl Pts',(104.810567363188,0.754023825900984,-12.5009978537989));
#57191=CARTESIAN_POINT('Ctrl Pts',(104.811368952344,0.672870923199062,-12.5009803357246));
#57192=CARTESIAN_POINT('Ctrl Pts',(104.811713578245,0.59167861130207,-12.5009506355434));
#57193=CARTESIAN_POINT('Ctrl Pts',(104.812466559252,0.414279673417628,-12.5008857429387));
#57194=CARTESIAN_POINT('Ctrl Pts',(104.811037004109,0.23695338523688,-12.5007631174331));
#57195=CARTESIAN_POINT('Ctrl Pts',(104.807425396501,0.059578059847195,-12.5006153254265));
#57196=CARTESIAN_POINT('Ctrl Pts',(104.807156097717,0.0463521049043557,
-12.5006043053457));
#57197=CARTESIAN_POINT('Ctrl Pts',(104.806874677527,0.0331263982138967,
-12.5005931427019));
#57198=CARTESIAN_POINT('Ctrl Pts',(104.806581139004,0.0199008894796828,
-12.5005818495349));
#57199=CARTESIAN_POINT('Ctrl Pts',(104.806500486957,0.0162670756548309,
-12.5005787466474));
#57200=CARTESIAN_POINT('Ctrl Pts',(104.806418920151,0.0126332802390204,
-12.5005756339081));
#57201=CARTESIAN_POINT('Ctrl Pts',(104.806336438654,0.00899950219642152,
-12.500572511564));
#57202=CARTESIAN_POINT('Ctrl Pts',(104.806287985393,0.00686486105990187,
-12.5005706773617));
#57203=CARTESIAN_POINT('Ctrl Pts',(104.80623921649,0.0047302263253564,-12.5005688398452));
#57204=CARTESIAN_POINT('Ctrl Pts',(104.80619013196,0.00259559779005463,
-12.5005669990643));
#57205=CARTESIAN_POINT('Ctrl Pts',(104.806147753723,0.000752618029680907,
-12.5005654097846));
#57206=CARTESIAN_POINT('Ctrl Pts',(104.806105140217,-0.00109035690604705,
-12.5005638180718));
#57207=CARTESIAN_POINT('Ctrl Pts',(104.806062291454,-0.0029333271355872,
-12.500562223958));
#57208=CARTESIAN_POINT('Ctrl Pts',(104.806010107776,-0.00517780184503334,
-12.5005602825548));
#57209=CARTESIAN_POINT('Ctrl Pts',(104.805957575176,-0.00742226928008383,
-12.5005583375906));
#57210=CARTESIAN_POINT('Ctrl Pts',(104.805904693668,-0.00966672981599251,
-12.5005563891231));
#57211=CARTESIAN_POINT('Ctrl Pts',(104.805804925161,-0.0139012246850115,
-12.5005527130612));
#57212=CARTESIAN_POINT('Ctrl Pts',(104.805703914798,-0.0181356927295366,
-12.5005490245313));
#57213=CARTESIAN_POINT('Ctrl Pts',(104.805601662698,-0.0223701355818334,
-12.5005453239189));
#57214=CARTESIAN_POINT('Ctrl Pts',(104.805019230717,-0.0464896885183316,
-12.5005242450852));
#57215=CARTESIAN_POINT('Ctrl Pts',(104.804396516915,-0.0706081685829107,
-12.5005027746528));
#57216=CARTESIAN_POINT('Ctrl Pts',(104.803733545885,-0.0947258798446518,
-12.5004809824714));
#57217=CARTESIAN_POINT('Ctrl Pts',(104.802885892622,-0.125562003504238,
-12.5004531196947));
#57218=CARTESIAN_POINT('Ctrl Pts',(104.801972451701,-0.156396061231039,
-12.5004247318868));
#57219=CARTESIAN_POINT('Ctrl Pts',(104.800993284962,-0.187228686091773,
-12.5003959593782));
#57220=CARTESIAN_POINT('Ctrl Pts',(104.796171488701,-0.339060472613246,
-12.500254272402));
#57221=CARTESIAN_POINT('Ctrl Pts',(104.789757904542,-0.490793335817318,
-12.5001036262456));
#57222=CARTESIAN_POINT('Ctrl Pts',(104.781764029618,-0.642501306198806,
-12.4999584778234));
#57223=CARTESIAN_POINT('Ctrl Pts',(104.76917486863,-0.881418737418034,-12.4997298907024));
#57224=CARTESIAN_POINT('Ctrl Pts',(104.752687747525,-1.11986127288837,-12.4995172107899));
#57225=CARTESIAN_POINT('Ctrl Pts',(104.732390128302,-1.35809925406382,-12.4993555671229));
#57226=CARTESIAN_POINT('Ctrl Pts',(104.722987028528,-1.46846567106078,-12.499280683881));
#57227=CARTESIAN_POINT('Ctrl Pts',(104.712766154114,-1.57878753286359,-12.4992164728357));
#57228=CARTESIAN_POINT('Ctrl Pts',(104.701736200614,-1.68908803070068,-12.4991653468104));
#57229=CARTESIAN_POINT('',(106.5160219149,-1.68935314531935,-12.5));
#57230=CARTESIAN_POINT('Ctrl Pts',(106.5160219149,-1.68934693203252,-12.4990807809333));
#57231=CARTESIAN_POINT('Ctrl Pts',(106.495712066664,-2.56876383854141,-12.3805352414928));
#57232=CARTESIAN_POINT('Ctrl Pts',(106.475402218428,-3.43570307962652,-12.1701285355112));
#57233=CARTESIAN_POINT('Ctrl Pts',(106.455092370193,-4.27031533948596,-11.8698673364697));
#57234=CARTESIAN_POINT('Ctrl Pts',(106.40800056911,-6.2055043210297,-11.1736612154764));
#57235=CARTESIAN_POINT('Ctrl Pts',(106.360908768026,-7.96689625422667,-9.99437733459268));
#57236=CARTESIAN_POINT('Ctrl Pts',(106.313816966943,-9.34784984467607,-8.47036389403563));
#57237=CARTESIAN_POINT('Ctrl Pts',(106.26672516586,-10.7288034351255,-6.94635045347851));
#57238=CARTESIAN_POINT('Ctrl Pts',(106.219633364777,-11.7293186828274,-5.07760745324805));
#57239=CARTESIAN_POINT('Ctrl Pts',(106.172541563694,-12.2320132550129,-3.08337759474184));
#57240=CARTESIAN_POINT('Ctrl Pts',(106.125449762611,-12.7347078271983,-1.08914773623572));
#57241=CARTESIAN_POINT('Ctrl Pts',(106.078357961528,-12.7395817238675,1.03056898054615));
#57242=CARTESIAN_POINT('Ctrl Pts',(106.031266160445,-12.2460642058922,3.02708924830187));
#57243=CARTESIAN_POINT('Ctrl Pts',(105.984174359362,-11.7525466879169,5.02360951605759));
#57244=CARTESIAN_POINT('Ctrl Pts',(105.937082558279,-10.7606377552971,6.89693333478716));
#57245=CARTESIAN_POINT('Ctrl Pts',(105.889990757196,-9.38670732174682,8.42728242690899));
#57246=CARTESIAN_POINT('Ctrl Pts',(105.842898956113,-8.01277688819656,9.95763151903081));
#57247=CARTESIAN_POINT('Ctrl Pts',(105.79580715503,-6.25682495371582,11.1450058845449));
#57248=CARTESIAN_POINT('Ctrl Pts',(105.748715353947,-4.32485945868025,11.850103424355));
#57249=CARTESIAN_POINT('Ctrl Pts',(105.701623552864,-2.39289396364465,12.5552009641652));
#57250=CARTESIAN_POINT('Ctrl Pts',(105.654531751781,-0.284914908054215,
12.7780216782715));
#57251=CARTESIAN_POINT('Ctrl Pts',(105.607439950697,1.7517704266388,12.4924241875336));
#57252=CARTESIAN_POINT('Ctrl Pts',(105.560348149614,3.78845576133182,12.2068266967957));
#57253=CARTESIAN_POINT('Ctrl Pts',(105.513256348531,5.75384737512741,11.4128110012137));
#57254=CARTESIAN_POINT('Ctrl Pts',(105.466164547448,7.41736612323887,10.2035308183321));
#57255=CARTESIAN_POINT('Ctrl Pts',(105.419072746365,9.08088487135031,8.9942506354505));
#57256=CARTESIAN_POINT('Ctrl Pts',(105.371980945282,10.4425307537776,7.36970596526928));
#57257=CARTESIAN_POINT('Ctrl Pts',(105.324889144199,11.3425559571878,5.52048781697627));
#57258=CARTESIAN_POINT('Ctrl Pts',(105.277797343116,12.2425811605979,3.67126966868326));
#57259=CARTESIAN_POINT('Ctrl Pts',(105.230705542033,12.6809856849908,1.59737804227846));
#57260=CARTESIAN_POINT('Ctrl Pts',(105.18361374095,12.6063360448345,-0.457878774668838));
#57261=CARTESIAN_POINT('Ctrl Pts',(105.136521939867,12.5316864046781,-2.51313559161616));
#57262=CARTESIAN_POINT('Ctrl Pts',(105.089430138784,11.9439825999724,-4.54975759910599));
#57263=CARTESIAN_POINT('Ctrl Pts',(105.042338337701,10.9121738512091,-6.32880898967823));
#57264=CARTESIAN_POINT('Ctrl Pts',(104.995246536618,9.88036510244591,-8.10786038025044));
#57265=CARTESIAN_POINT('Ctrl Pts',(104.948154735535,8.40445140962515,-9.62934115390508));
#57266=CARTESIAN_POINT('Ctrl Pts',(104.901062934452,6.65758647161741,-10.7147516908012));
#57267=CARTESIAN_POINT('Ctrl Pts',(104.860480274491,5.15217737394656,-11.6501341931341));
#57268=CARTESIAN_POINT('Ctrl Pts',(104.81989761453,3.44554344694001,-12.2616644876296));
#57269=CARTESIAN_POINT('Ctrl Pts',(104.77931495457,1.6891935564243,-12.5005864930276));
#57270=CARTESIAN_POINT('',(106.593600668856,1.68935314531922,-12.5));
#57271=CARTESIAN_POINT('Ctrl Pts',(106.593600668856,1.68952807354336,-12.5009853194712));
#57272=CARTESIAN_POINT('Ctrl Pts',(106.594102574019,1.68034421904941,-12.5009832688272));
#57273=CARTESIAN_POINT('Ctrl Pts',(106.594598745324,1.67116003522182,-12.5009810445824));
#57274=CARTESIAN_POINT('Ctrl Pts',(106.595089178393,1.66197550718774,-12.500978651551));
#57275=CARTESIAN_POINT('Ctrl Pts',(106.608363594638,1.41338042703455,-12.50091388003));
#57276=CARTESIAN_POINT('Ctrl Pts',(106.617416131364,1.1648664983038,-12.5007274931519));
#57277=CARTESIAN_POINT('Ctrl Pts',(106.622195076342,0.916129042150179,-12.5005048281007));
#57278=CARTESIAN_POINT('Ctrl Pts',(106.624270835107,0.808088678176874,-12.5004081124168));
#57279=CARTESIAN_POINT('Ctrl Pts',(106.625540319729,0.70000547944534,-12.5003043542637));
#57280=CARTESIAN_POINT('Ctrl Pts',(106.625999292531,0.59185171030578,-12.5001993366535));
#57281=CARTESIAN_POINT('Ctrl Pts',(106.626752273537,0.41441693946698,-12.5000270469983));
#57282=CARTESIAN_POINT('Ctrl Pts',(106.625322718394,0.237052919580531,-12.4998518560448));
#57283=CARTESIAN_POINT('Ctrl Pts',(106.621711110787,0.0596396457159169,
-12.49969399153));
#57284=CARTESIAN_POINT('Ctrl Pts',(106.621441812002,0.0464108611478938,
-12.4996822203947));
#57285=CARTESIAN_POINT('Ctrl Pts',(106.621160391813,0.0331823237433037,
-12.4996705429826));
#57286=CARTESIAN_POINT('Ctrl Pts',(106.620866853289,0.0199539839213671,
-12.4996589661652));
#57287=CARTESIAN_POINT('Ctrl Pts',(106.620786201243,0.0163193922582425,
-12.4996557853424));
#57288=CARTESIAN_POINT('Ctrl Pts',(106.620704634438,0.0126848189755927,
-12.4996526121156));
#57289=CARTESIAN_POINT('Ctrl Pts',(106.62062215294,0.00905026296460605,
-12.4996494466242));
#57290=CARTESIAN_POINT('Ctrl Pts',(106.620573699678,0.00691516480986947,
-12.4996475870753));
#57291=CARTESIAN_POINT('Ctrl Pts',(106.620524930774,0.00478007305231262,
-12.4996457301962));
#57292=CARTESIAN_POINT('Ctrl Pts',(106.620475846246,0.00264498761126058,
-12.4996438760151));
#57293=CARTESIAN_POINT('Ctrl Pts',(106.620433468009,0.000801613303429549,
-12.4996422751659));
#57294=CARTESIAN_POINT('Ctrl Pts',(106.620390854503,-0.00104175618109215,
-12.499640676328));
#57295=CARTESIAN_POINT('Ctrl Pts',(106.62034800574,-0.00288512096233046,
-12.4996390795193));
#57296=CARTESIAN_POINT('Ctrl Pts',(106.620295822061,-0.00513007619243232,
-12.4996371348342));
#57297=CARTESIAN_POINT('Ctrl Pts',(106.620243289461,-0.00737502414715744,
-12.4996351931592));
#57298=CARTESIAN_POINT('Ctrl Pts',(106.620190407953,-0.0096199651517339,
-12.4996332545265));
#57299=CARTESIAN_POINT('Ctrl Pts',(106.620090639447,-0.0138553665431028,
-12.4996295970193));
#57300=CARTESIAN_POINT('Ctrl Pts',(106.619989629084,-0.0180907410943302,
-12.4996259503431));
#57301=CARTESIAN_POINT('Ctrl Pts',(106.619887376984,-0.0223260904432372,
-12.4996223147132));
#57302=CARTESIAN_POINT('Ctrl Pts',(106.619304945002,-0.0464508067240482,
-12.4996016060229));
#57303=CARTESIAN_POINT('Ctrl Pts',(106.618682231199,-0.07057444882255,-12.4995812561438));
#57304=CARTESIAN_POINT('Ctrl Pts',(106.618019260169,-0.0946973165648927,
-12.4995613035175));
#57305=CARTESIAN_POINT('Ctrl Pts',(106.617171606944,-0.125540031735592,
-12.4995357927375));
#57306=CARTESIAN_POINT('Ctrl Pts',(106.616258166066,-0.156380671725298,
-12.4995109322356));
#57307=CARTESIAN_POINT('Ctrl Pts',(106.615278999377,-0.187219860747437,
-12.499486796637));
#57308=CARTESIAN_POINT('Ctrl Pts',(106.610457203316,-0.339083973146112,
-12.4993679436004));
#57309=CARTESIAN_POINT('Ctrl Pts',(106.604043619468,-0.490848708425859,
-12.4992670176415));
#57310=CARTESIAN_POINT('Ctrl Pts',(106.596049744968,-0.642587048357201,
-12.4991906401119));
#57311=CARTESIAN_POINT('Ctrl Pts',(106.583417868099,-0.882363145197298,
-12.4990699487565));
#57312=CARTESIAN_POINT('Ctrl Pts',(106.566861534007,-1.12165729659649,-12.4990125535785));
#57313=CARTESIAN_POINT('Ctrl Pts',(106.546469098015,-1.36073855108457,-12.4990236220852));
#57314=CARTESIAN_POINT('Ctrl Pts',(106.537122978201,-1.47031261327066,-12.4990286949264));
#57315=CARTESIAN_POINT('Ctrl Pts',(106.526971081869,-1.57984130388627,-12.4990478927983));
#57316=CARTESIAN_POINT('Ctrl Pts',(106.5160219149,-1.68934693203216,-12.4990807809333));
#57317=CARTESIAN_POINT('',(107.444020192937,0.782909338907702,12.5893195613048));
#57318=CARTESIAN_POINT('Ctrl Pts',(107.444020192937,0.782909338906896,12.5893195613048));
#57319=CARTESIAN_POINT('Ctrl Pts',(107.396928391854,2.83606438077655,12.4616371835023));
#57320=CARTESIAN_POINT('Ctrl Pts',(107.349836590771,4.85644362728424,11.8222740696369));
#57321=CARTESIAN_POINT('Ctrl Pts',(107.302744789688,6.60816901018162,10.7451655348056));
#57322=CARTESIAN_POINT('Ctrl Pts',(107.255652988605,8.35989439307901,9.66805699997423));
#57323=CARTESIAN_POINT('Ctrl Pts',(107.208561187522,9.84296591236608,8.15320304417694));
#57324=CARTESIAN_POINT('Ctrl Pts',(107.161469386439,10.8829918506863,6.37887339924185));
#57325=CARTESIAN_POINT('Ctrl Pts',(107.114377585355,11.9230177890065,4.60454375430671));
#57326=CARTESIAN_POINT('Ctrl Pts',(107.067285784272,12.5199981463597,2.57073842023375));
#57327=CARTESIAN_POINT('Ctrl Pts',(107.020193983189,12.6040774571683,0.515871141998574));
#57328=CARTESIAN_POINT('Ctrl Pts',(106.973102182106,12.6881567679768,-1.53899613623655));
#57329=CARTESIAN_POINT('Ctrl Pts',(106.926010381023,12.2593350322407,-3.61492535863389));
#57330=CARTESIAN_POINT('Ctrl Pts',(106.87891857994,11.3678344699642,-5.46827444689482));
#57331=CARTESIAN_POINT('Ctrl Pts',(106.831826778857,10.4763339076878,-7.32162353515575));
#57332=CARTESIAN_POINT('Ctrl Pts',(106.784734977774,9.12215451887095,-8.95239248928027));
#57333=CARTESIAN_POINT('Ctrl Pts',(106.737643176691,7.46420991976001,-10.1693050890532));
#57334=CARTESIAN_POINT('Ctrl Pts',(106.690551375608,5.80626532064906,-11.3862176888261));
#57335=CARTESIAN_POINT('Ctrl Pts',(106.643459574525,3.84455551124398,-12.1892739342474));
#57336=CARTESIAN_POINT('Ctrl Pts',(106.596367773442,1.80920759159618,-12.4842378764066));
#57337=CARTESIAN_POINT('Ctrl Pts',(106.595445405246,1.76934204930534,-12.4900152166819));
#57338=CARTESIAN_POINT('Ctrl Pts',(106.594523037051,1.7294482568701,-12.4955976350495));
#57339=CARTESIAN_POINT('Ctrl Pts',(106.593600668856,1.68952807354336,-12.5009853194712));
#57340=CARTESIAN_POINT('Ctrl Pts',(108.008153428708,1.61683638546961,11.4839173606684));
#57341=CARTESIAN_POINT('Ctrl Pts',(107.966031738243,1.57797833705833,11.5652727241384));
#57342=CARTESIAN_POINT('Ctrl Pts',(107.924174837091,1.5363367640964,11.6463102940928));
#57343=CARTESIAN_POINT('Ctrl Pts',(107.883039431048,1.49176115295735,11.7261593831322));
#57344=CARTESIAN_POINT('Ctrl Pts',(107.843254818669,1.44864930403286,11.8033864087513));
#57345=CARTESIAN_POINT('Ctrl Pts',(107.804145094866,1.40279277474693,11.8795015989354));
#57346=CARTESIAN_POINT('Ctrl Pts',(107.766123435132,1.35410262839987,11.9537045620535));
#57347=CARTESIAN_POINT('Ctrl Pts',(107.751995478605,1.33601051259738,11.9812766418754));
#57348=CARTESIAN_POINT('Ctrl Pts',(107.738017750126,1.31752765476251,12.0085845828291));
#57349=CARTESIAN_POINT('Ctrl Pts',(107.72421144694,1.2986513057777,12.0355869118102));
#57350=CARTESIAN_POINT('Ctrl Pts',(107.693743691972,1.2569949718699,12.0951756613734));
#57351=CARTESIAN_POINT('Ctrl Pts',(107.663609982109,1.21276627861128,12.1542515643353));
#57352=CARTESIAN_POINT('Ctrl Pts',(107.634283495276,1.16587466320814,12.2119162262066));
#57353=CARTESIAN_POINT('Ctrl Pts',(107.60566926689,1.120121914161,12.2681803745155));
#57354=CARTESIAN_POINT('Ctrl Pts',(107.577823527304,1.07183375384895,12.3231008875987));
#57355=CARTESIAN_POINT('Ctrl Pts',(107.55118580849,1.02097382111972,12.3758332678361));
#57356=CARTESIAN_POINT('Ctrl Pts',(107.525353444986,0.971651569493986,12.4269713560586));
#57357=CARTESIAN_POINT('Ctrl Pts',(107.500657160734,0.919910564744948,12.4760514858375));
#57358=CARTESIAN_POINT('Ctrl Pts',(107.477497814894,0.865765955833377,12.5222957773865));
#57359=CARTESIAN_POINT('Ctrl Pts',(107.465939154467,0.838742776824957,12.5453759656779));
#57360=CARTESIAN_POINT('Ctrl Pts',(107.454763335443,0.811121652850066,12.5677496555355));
#57361=CARTESIAN_POINT('Ctrl Pts',(107.444020192937,0.782909338907791,12.5893195613048));
#57362=CARTESIAN_POINT('',(96.446025,7.1032002856509,-9.1678677603644));
#57363=CARTESIAN_POINT('Ctrl Pts',(96.446025,7.1032002856509,-9.1678677603644));
#57364=CARTESIAN_POINT('Ctrl Pts',(96.4931168010831,8.59836083215431,-8.00942775025295));
#57365=CARTESIAN_POINT('Ctrl Pts',(96.5873004032492,11.0098238737483,-4.94829702622741));
#57366=CARTESIAN_POINT('Ctrl Pts',(96.7285758064984,12.0436316920041,0.807234573314296));
#57367=CARTESIAN_POINT('Ctrl Pts',(96.8698512097476,10.2513621865474,6.37239418233372));
#57368=CARTESIAN_POINT('Ctrl Pts',(97.0111266129968,6.05378860029595,10.4428153879447));
#57369=CARTESIAN_POINT('Ctrl Pts',(97.152402016246,0.435723763467222,12.0627151308176));
#57370=CARTESIAN_POINT('Ctrl Pts',(97.2936774194952,-5.28456262813498,10.8523362109951));
#57371=CARTESIAN_POINT('Ctrl Pts',(97.4349528227444,-9.76489064575089,7.09552016347875));
#57372=CARTESIAN_POINT('Ctrl Pts',(97.5425267380375,-11.4317746886518,2.9671918442554));
#57373=CARTESIAN_POINT('Ctrl Pts',(97.6030088522475,-11.5978336888622,0.538110614070643));
#57374=CARTESIAN_POINT('Ctrl Pts',(97.6163991653745,-11.5973549676912,0.00026415572522899));
#57375=CARTESIAN_POINT('',(96.446025,5.49758084898117,11.3528330610334));
#57376=CARTESIAN_POINT('Ctrl Pts',(96.446025,5.4978005759398,11.3530041107288));
#57377=CARTESIAN_POINT('Ctrl Pts',(96.446025,5.75802350928769,11.2143077748595));
#57378=CARTESIAN_POINT('Ctrl Pts',(96.446025,6.01305469750609,11.0665970670471));
#57379=CARTESIAN_POINT('Ctrl Pts',(96.446025,6.26237325434567,10.910023872863));
#57380=CARTESIAN_POINT('Ctrl Pts',(96.446025,6.27759354024327,10.9004654636952));
#57381=CARTESIAN_POINT('Ctrl Pts',(96.446025,6.29279252804283,10.8908740118952));
#57382=CARTESIAN_POINT('Ctrl Pts',(96.446025,6.30797009589712,10.8812495466477));
#57383=CARTESIAN_POINT('Ctrl Pts',(96.446025,6.55734691236906,10.7231136366833));
#57384=CARTESIAN_POINT('Ctrl Pts',(96.446025,6.80094385595134,10.5560686290167));
#57385=CARTESIAN_POINT('Ctrl Pts',(96.446025,7.03838271553362,10.3805320487659));
#57386=CARTESIAN_POINT('Ctrl Pts',(96.446025,7.21294398807995,10.2514803472839));
#57387=CARTESIAN_POINT('Ctrl Pts',(96.446025,7.38417623425726,10.1178380533548));
#57388=CARTESIAN_POINT('Ctrl Pts',(96.446025,7.55191654776048,9.97975830214868));
#57389=CARTESIAN_POINT('Ctrl Pts',(96.446025,7.62992441658677,9.91554411955476));
#57390=CARTESIAN_POINT('Ctrl Pts',(96.446025,7.70717691379675,9.85037009448964));
#57391=CARTESIAN_POINT('Ctrl Pts',(96.446025,7.78365677159635,9.78425093759342));
#57392=CARTESIAN_POINT('Ctrl Pts',(96.446025,7.83453670777231,9.74026368945153));
#57393=CARTESIAN_POINT('Ctrl Pts',(96.446025,7.88507467175993,9.69585812919905));
#57394=CARTESIAN_POINT('Ctrl Pts',(96.446025,7.93526543264948,9.65103849064499));
#57395=CARTESIAN_POINT('Ctrl Pts',(96.446025,7.96671726405787,9.62295245069256));
#57396=CARTESIAN_POINT('Ctrl Pts',(96.446025,7.99802688312031,9.59470901524118));
#57397=CARTESIAN_POINT('Ctrl Pts',(96.446025,8.02918789242708,9.5663142635499));
#57398=CARTESIAN_POINT('Ctrl Pts',(96.446025,8.24626937643572,9.36850376343036));
#57399=CARTESIAN_POINT('Ctrl Pts',(96.446025,8.45622333104263,9.16327984499431));
#57400=CARTESIAN_POINT('Ctrl Pts',(96.446025,8.65868156283819,8.95105692458998));
#57401=CARTESIAN_POINT('Ctrl Pts',(96.446025,8.86053340792298,8.73946963731111));
#57402=CARTESIAN_POINT('Ctrl Pts',(96.446025,9.0549347499723,8.52092472280692));
#57403=CARTESIAN_POINT('Ctrl Pts',(96.446025,9.24148137322108,8.29579970571171));
#57404=CARTESIAN_POINT('Ctrl Pts',(96.446025,9.42654383520758,8.07246577882077));
#57405=CARTESIAN_POINT('Ctrl Pts',(96.446025,9.60387640350412,7.84265555342141));
#57406=CARTESIAN_POINT('Ctrl Pts',(96.446025,9.77304034211128,7.60671216649778));
#57407=CARTESIAN_POINT('Ctrl Pts',(96.446025,9.81546086641513,7.54754564281823));
#57408=CARTESIAN_POINT('Ctrl Pts',(96.446025,9.8573674867971,7.48799333868432));
#57409=CARTESIAN_POINT('Ctrl Pts',(96.446025,9.89875280632189,7.42806046573141));
#57410=CARTESIAN_POINT('Ctrl Pts',(96.446025,9.91788263026291,7.40035727723286));
#57411=CARTESIAN_POINT('Ctrl Pts',(96.446025,9.93689621068264,7.37257979211348));
#57412=CARTESIAN_POINT('Ctrl Pts',(96.446025,9.95579098474034,7.34473162572225));
#57413=CARTESIAN_POINT('Ctrl Pts',(96.446025,10.119018138577,7.10415838966613));
#57414=CARTESIAN_POINT('Ctrl Pts',(96.446025,10.27343184152,6.8582414172292));
#57415=CARTESIAN_POINT('Ctrl Pts',(96.446025,10.4186815916346,6.60737648542902));
#57416=CARTESIAN_POINT('Ctrl Pts',(96.446025,10.437263930765,6.57528240447552));
#57417=CARTESIAN_POINT('Ctrl Pts',(96.446025,10.4556962275322,6.54310729772208));
#57418=CARTESIAN_POINT('Ctrl Pts',(96.446025,10.4739776980424,6.51085195781411));
#57419=CARTESIAN_POINT('Ctrl Pts',(96.446025,10.6166099532034,6.25919540373678));
#57420=CARTESIAN_POINT('Ctrl Pts',(96.446025,10.7500650514451,6.00265698749348));
#57421=CARTESIAN_POINT('Ctrl Pts',(96.446025,10.8742414607825,5.74178192512992));
#57422=CARTESIAN_POINT('Ctrl Pts',(96.446025,10.9989235002189,5.47984461362972));
#57423=CARTESIAN_POINT('Ctrl Pts',(96.446025,11.1142513075349,5.21353465970876));
#57424=CARTESIAN_POINT('Ctrl Pts',(96.446025,11.2200732858474,4.94338427334107));
#57425=CARTESIAN_POINT('Ctrl Pts',(96.446025,11.3256004400896,4.67398653626053));
#57426=CARTESIAN_POINT('Ctrl Pts',(96.446025,11.4216747837927,4.40076911982243));
#57427=CARTESIAN_POINT('Ctrl Pts',(96.446025,11.5080953785583,4.12424946024983));
#57428=CARTESIAN_POINT('Ctrl Pts',(96.446025,11.5919051535307,3.85608363117774));
#57429=CARTESIAN_POINT('Ctrl Pts',(96.446025,11.6666355551521,3.58481151953519));
#57430=CARTESIAN_POINT('Ctrl Pts',(96.446025,11.7320558790342,3.31090391283863));
#57431=CARTESIAN_POINT('Ctrl Pts',(96.446025,11.7470314809477,3.24820273626922));
#57432=CARTESIAN_POINT('Ctrl Pts',(96.446025,11.7615190232195,3.18536347007864));
#57433=CARTESIAN_POINT('Ctrl Pts',(96.446025,11.7755153823783,3.12239179797609));
#57434=CARTESIAN_POINT('Ctrl Pts',(96.446025,11.7841026482886,3.08375642951829));
#57435=CARTESIAN_POINT('Ctrl Pts',(96.446025,11.7925058566515,3.04506702517162));
#57436=CARTESIAN_POINT('Ctrl Pts',(96.446025,11.8007185497336,3.00635254211889));
#57437=CARTESIAN_POINT('Ctrl Pts',(96.446025,11.8603768204461,2.72512455912071));
#57438=CARTESIAN_POINT('Ctrl Pts',(96.446025,11.9100466496312,2.44231213195589));
#57439=CARTESIAN_POINT('Ctrl Pts',(96.446025,11.9496224947969,2.15843752916402));
#57440=CARTESIAN_POINT('Ctrl Pts',(96.446025,11.9891050030404,1.87523242519441));
#57441=CARTESIAN_POINT('Ctrl Pts',(96.446025,12.0185411852995,1.59096953933644));
#57442=CARTESIAN_POINT('Ctrl Pts',(96.446025,12.0377756152134,1.30615747712036));
#57443=CARTESIAN_POINT('Ctrl Pts',(96.446025,12.0489742493925,1.14033472548109));
#57444=CARTESIAN_POINT('Ctrl Pts',(96.446025,12.0567137609233,0.974325676220046));
#57445=CARTESIAN_POINT('Ctrl Pts',(96.446025,12.0609553233804,0.808230381556516));
#57446=CARTESIAN_POINT('Ctrl Pts',(96.446025,12.0682685793829,0.521850675269838));
#57447=CARTESIAN_POINT('Ctrl Pts',(96.446025,12.0651858299839,0.23521395735393));
#57448=CARTESIAN_POINT('Ctrl Pts',(96.446025,12.0518194398101,-0.0511360161595567));
#57449=CARTESIAN_POINT('Ctrl Pts',(96.446025,12.0384958623745,-0.336568806627351));
#57450=CARTESIAN_POINT('Ctrl Pts',(96.446025,12.0149542352207,-0.62171729672152));
#57451=CARTESIAN_POINT('Ctrl Pts',(96.446025,11.981256120355,-0.906029323615214));
#57452=CARTESIAN_POINT('Ctrl Pts',(96.446025,11.9609240474986,-1.0775716448339));
#57453=CARTESIAN_POINT('Ctrl Pts',(96.446025,11.9368936343814,-1.24880915430181));
#57454=CARTESIAN_POINT('Ctrl Pts',(96.446025,11.9091700093926,-1.41961674289046));
#57455=CARTESIAN_POINT('Ctrl Pts',(96.446025,11.9018068261626,-1.46498193493737));
#57456=CARTESIAN_POINT('Ctrl Pts',(96.446025,11.8941830925326,-1.51031678185175));
#57457=CARTESIAN_POINT('Ctrl Pts',(96.446025,11.8862988316856,-1.55561889700612));
#57458=CARTESIAN_POINT('Ctrl Pts',(96.446025,11.8799799710488,-1.59192639085565));
#57459=CARTESIAN_POINT('Ctrl Pts',(96.446025,11.8734931827204,-1.6282157770847));
#57460=CARTESIAN_POINT('Ctrl Pts',(96.446025,11.8668430364879,-1.66446169168796));
#57461=CARTESIAN_POINT('Ctrl Pts',(96.446025,11.8155846022351,-1.94384033475061));
#57462=CARTESIAN_POINT('Ctrl Pts',(96.446025,11.754576219872,-2.22092831643957));
#57463=CARTESIAN_POINT('Ctrl Pts',(96.446025,11.6839893564517,-2.49521102281565));
#57464=CARTESIAN_POINT('Ctrl Pts',(96.446025,11.6133492547656,-2.76970059963333));
#57465=CARTESIAN_POINT('Ctrl Pts',(96.446025,11.5331160419521,-3.04138128031828));
#57466=CARTESIAN_POINT('Ctrl Pts',(96.446025,11.44341031998,-3.30972710363197));
#57467=CARTESIAN_POINT('Ctrl Pts',(96.446025,11.3545530114623,-3.57553498174052));
#57468=CARTESIAN_POINT('Ctrl Pts',(96.446025,11.2564012837368,-3.83807134091528));
#57469=CARTESIAN_POINT('Ctrl Pts',(96.446025,11.149025305932,-4.09680634848039));
#57470=CARTESIAN_POINT('Ctrl Pts',(96.446025,11.0425657924693,-4.35333302776457));
#57471=CARTESIAN_POINT('Ctrl Pts',(96.446025,10.9270386065772,-4.60612349036155));
#57472=CARTESIAN_POINT('Ctrl Pts',(96.446025,10.8024689941292,-4.85463493583518));
#57473=CARTESIAN_POINT('Ctrl Pts',(96.446025,10.6953943412341,-5.06824462957723));
#57474=CARTESIAN_POINT('Ctrl Pts',(96.446025,10.5816377838971,-5.27869247154203));
#57475=CARTESIAN_POINT('Ctrl Pts',(96.446025,10.4613871615161,-5.48570603579521));
#57476=CARTESIAN_POINT('Ctrl Pts',(96.446025,10.4087775142244,-5.57627447015598));
#57477=CARTESIAN_POINT('Ctrl Pts',(96.446025,10.3549246251689,-5.66618531594217));
#57478=CARTESIAN_POINT('Ctrl Pts',(96.446025,10.2998431779684,-5.75541454179228));
#57479=CARTESIAN_POINT('Ctrl Pts',(96.446025,10.2799271554621,-5.78767751527195));
#57480=CARTESIAN_POINT('Ctrl Pts',(96.446025,10.2598505107673,-5.81985136917303));
#57481=CARTESIAN_POINT('Ctrl Pts',(96.446025,10.2396139191792,-5.85193494173057));
#57482=CARTESIAN_POINT('Ctrl Pts',(96.446025,10.22069632276,-5.88192734804515));
#57483=CARTESIAN_POINT('Ctrl Pts',(96.446025,10.2016377782411,-5.91184258810781));
#57484=CARTESIAN_POINT('Ctrl Pts',(96.446025,10.1824512248116,-5.94166071224686));
#57485=CARTESIAN_POINT('Ctrl Pts',(96.446025,10.0316611993092,-6.17600586005514));
#57486=CARTESIAN_POINT('Ctrl Pts',(96.446025,9.872806361262,-6.40461413627334));
#57487=CARTESIAN_POINT('Ctrl Pts',(96.446025,9.70628844661517,-6.62713123184326));
#57488=CARTESIAN_POINT('Ctrl Pts',(96.446025,9.53861194535784,-6.85119654117794));
#57489=CARTESIAN_POINT('Ctrl Pts',(96.446025,9.36316496265846,-7.06908609777102));
#57490=CARTESIAN_POINT('Ctrl Pts',(96.446025,9.18031378687851,-7.28040897935406));
#57491=CARTESIAN_POINT('Ctrl Pts',(96.446025,8.99786583245493,-7.4912658540953));
#57492=CARTESIAN_POINT('Ctrl Pts',(96.446025,8.80804585445648,-7.69558542180113));
#57493=CARTESIAN_POINT('Ctrl Pts',(96.446025,8.61118064520521,-7.89294354453129));
#57494=CARTESIAN_POINT('Ctrl Pts',(96.446025,8.41581792234265,-8.08879541892925));
#57495=CARTESIAN_POINT('Ctrl Pts',(96.446025,8.213516645606,-8.27779209165663));
#57496=CARTESIAN_POINT('Ctrl Pts',(96.446025,8.0045663838185,-8.45947766735397));
#57497=CARTESIAN_POINT('Ctrl Pts',(96.446025,7.79927809976704,-8.63797909517099));
#57498=CARTESIAN_POINT('Ctrl Pts',(96.446025,7.58757139889719,-8.80942372620072));
#57499=CARTESIAN_POINT('Ctrl Pts',(96.446025,7.36969868465615,-8.97333427215897));
#57500=CARTESIAN_POINT('Ctrl Pts',(96.446025,7.28186302611182,-9.03941501474648));
#57501=CARTESIAN_POINT('Ctrl Pts',(96.446025,7.19302498107236,-9.1042706958156));
#57502=CARTESIAN_POINT('Ctrl Pts',(96.446025,7.10320028565113,-9.16786776036423));
#57503=CARTESIAN_POINT('Ctrl Pts',(97.4445933434715,-1.68965488935083,-12.5000313373793));
#57504=CARTESIAN_POINT('Ctrl Pts',(97.4342177497292,-2.13885530702409,-12.4397673843726));
#57505=CARTESIAN_POINT('Ctrl Pts',(97.4238421559868,-2.58473989646664,-12.3553149612025));
#57506=CARTESIAN_POINT('Ctrl Pts',(97.4134665622445,-3.02464884153746,-12.2466674174002));
#57507=CARTESIAN_POINT('Ctrl Pts',(97.3663747611614,-5.02126754600492,-11.7535478284925));
#57508=CARTESIAN_POINT('Ctrl Pts',(97.3192829600784,-6.89478869514797,-10.7620116646819));
#57509=CARTESIAN_POINT('Ctrl Pts',(97.2721911589953,-8.42541152523419,-9.388386362015));
#57510=CARTESIAN_POINT('Ctrl Pts',(97.2250993579122,-9.95603435532041,-8.01476105934808));
#57511=CARTESIAN_POINT('Ctrl Pts',(97.1780075568291,-11.1437588663498,-6.25904661782482));
#57512=CARTESIAN_POINT('Ctrl Pts',(97.1309157557461,-11.8492413813291,-4.32722131968821));
#57513=CARTESIAN_POINT('Ctrl Pts',(97.083823954663,-12.5547238963084,-2.3953960215516));
#57514=CARTESIAN_POINT('Ctrl Pts',(97.0367321535799,-12.7779644152377,-0.287459866801626));
#57515=CARTESIAN_POINT('Ctrl Pts',(96.9896403524969,-12.4927729217965,1.74928154978578));
#57516=CARTESIAN_POINT('Ctrl Pts',(96.9425485514138,-12.2075814283553,3.78602296637319));
#57517=CARTESIAN_POINT('Ctrl Pts',(96.8954567503308,-11.4139579225437,5.75156964479803));
#57518=CARTESIAN_POINT('Ctrl Pts',(96.8483649492477,-10.2050090351847,7.4153310294173));
#57519=CARTESIAN_POINT('Ctrl Pts',(96.8012731481646,-8.99606014782565,9.07909241403658));
#57520=CARTESIAN_POINT('Ctrl Pts',(96.7541813470815,-7.37178587891919,10.4410685048503));
#57521=CARTESIAN_POINT('Ctrl Pts',(96.7070895459985,-5.52274765596046,11.3414587153849));
#57522=CARTESIAN_POINT('Ctrl Pts',(96.6599977449154,-3.67370943300174,12.2418489259194));
#57523=CARTESIAN_POINT('Ctrl Pts',(96.6129059438324,-1.59990725599075,12.6806532561748));
#57524=CARTESIAN_POINT('Ctrl Pts',(96.5658141427493,0.455365491869809,12.606420506603));
#57525=CARTESIAN_POINT('Ctrl Pts',(96.5258844284996,2.19805639856598,12.5434776500929));
#57526=CARTESIAN_POINT('Ctrl Pts',(96.4859547142498,3.92742547663266,12.1116841397094));
#57527=CARTESIAN_POINT('Ctrl Pts',(96.446025,5.49780057593998,11.3530041107288));
#57528=CARTESIAN_POINT('Ctrl Pts',(107.482029246699,-0.87623857414724,12.583168122964));
#57529=CARTESIAN_POINT('Ctrl Pts',(107.513300150711,-2.23895227724843,12.4882745078976));
#57530=CARTESIAN_POINT('Ctrl Pts',(107.607112862745,-6.28931688652167,11.5416513005363));
#57531=CARTESIAN_POINT('Ctrl Pts',(107.73219647879,-10.6085644348937,7.75715356972124));
#57532=CARTESIAN_POINT('Ctrl Pts',(107.888550998846,-13.0749717130243,1.27479764955593));
#57533=CARTESIAN_POINT('Ctrl Pts',(108.013634614891,-12.3768301122727,-4.42234600477363));
#57534=CARTESIAN_POINT('Ctrl Pts',(108.169989134948,-8.39216919057065,-10.1004171650069));
#57535=CARTESIAN_POINT('Ctrl Pts',(108.263801846982,-4.56292341074069,-12.0725978039739));
#57536=CARTESIAN_POINT('Ctrl Pts',(108.326343655004,-1.86078767833722,-12.47563157783));
#57537=CARTESIAN_POINT('Ctrl Pts',(107.677558537865,-0.852712233050537,
12.2453196030831));
#57538=CARTESIAN_POINT('Ctrl Pts',(107.708829441876,-2.17883810682964,12.1529738096052));
#57539=CARTESIAN_POINT('Ctrl Pts',(107.80264215391,-6.12045349850929,11.2317667173564));
#57540=CARTESIAN_POINT('Ctrl Pts',(107.927725769955,-10.3237325263182,7.54887988010594));
#57541=CARTESIAN_POINT('Ctrl Pts',(108.084080290012,-12.7239186397789,1.24057029958798));
#57542=CARTESIAN_POINT('Ctrl Pts',(108.209163906057,-12.0445216114733,-4.30360936885544));
#57543=CARTESIAN_POINT('Ctrl Pts',(108.365518426114,-8.16684581318923,-9.82922862520268));
#57544=CARTESIAN_POINT('Ctrl Pts',(108.459331138147,-4.44041237809897,-11.7484577098948));
#57545=CARTESIAN_POINT('Ctrl Pts',(108.52187294617,-1.81082694056469,-12.1406703326204));
#57546=CARTESIAN_POINT('Ctrl Pts',(107.873087829031,-0.829185891953833,
11.9074710832022));
#57547=CARTESIAN_POINT('Ctrl Pts',(107.904358733042,-2.11872393641085,11.8176731113129));
#57548=CARTESIAN_POINT('Ctrl Pts',(107.998171445076,-5.95159011049691,10.9218821341765));
#57549=CARTESIAN_POINT('Ctrl Pts',(108.123255061121,-10.0389006177427,7.34060619049065));
#57550=CARTESIAN_POINT('Ctrl Pts',(108.279609581177,-12.3728655665335,1.20634294962002));
#57551=CARTESIAN_POINT('Ctrl Pts',(108.404693197223,-11.7122131106739,-4.18487273293724));
#57552=CARTESIAN_POINT('Ctrl Pts',(108.561047717279,-7.9415224358078,-9.55804008539851));
#57553=CARTESIAN_POINT('Ctrl Pts',(108.654860429313,-4.31790134545723,-11.4243176158158));
#57554=CARTESIAN_POINT('Ctrl Pts',(108.717402237336,-1.76086620279216,-11.8057090874109));
#57555=CARTESIAN_POINT('Ctrl Pts',(108.068617120196,-0.80565955085713,11.5696225633213));
#57556=CARTESIAN_POINT('Ctrl Pts',(108.099888024207,-2.05860976599205,11.4823724130206));
#57557=CARTESIAN_POINT('Ctrl Pts',(108.193700736241,-5.78272672248452,10.6119975509966));
#57558=CARTESIAN_POINT('Ctrl Pts',(108.318784352286,-9.75406870916728,7.13233250087535));
#57559=CARTESIAN_POINT('Ctrl Pts',(108.475138872343,-12.0218124932882,1.17211559965207));
#57560=CARTESIAN_POINT('Ctrl Pts',(108.600222488388,-11.3799046098746,-4.06613609701905));
#57561=CARTESIAN_POINT('Ctrl Pts',(108.756577008445,-7.71619905842638,-9.28685154559433));
#57562=CARTESIAN_POINT('Ctrl Pts',(108.850389720479,-4.1953903128155,-11.1001775217368));
#57563=CARTESIAN_POINT('Ctrl Pts',(108.912931528501,-1.71090546501964,-11.4707478422013));
#57564=CARTESIAN_POINT('',(108.902670614213,-2.11726001551285,-11.4025478033388));
#57565=CARTESIAN_POINT('',(108.326343655004,-1.8607876783373,-12.47563157783));
#57566=CARTESIAN_POINT('Ctrl Pts',(108.902670614213,-2.11721675886238,-11.4024697825115));
#57567=CARTESIAN_POINT('Ctrl Pts',(108.834581877771,-2.09803382047897,-11.5278634706509));
#57568=CARTESIAN_POINT('Ctrl Pts',(108.766763876508,-2.07538442706099,-11.6532854109009));
#57569=CARTESIAN_POINT('Ctrl Pts',(108.699537896827,-2.04914360253286,-11.7780872230819));
#57570=CARTESIAN_POINT('Ctrl Pts',(108.670954314328,-2.03798635683282,-11.8311512752736));
#57571=CARTESIAN_POINT('Ctrl Pts',(108.642477759625,-2.02618043104393,-11.8841030055665));
#57572=CARTESIAN_POINT('Ctrl Pts',(108.614132928961,-2.01371895975861,-11.936891665109));
#57573=CARTESIAN_POINT('Ctrl Pts',(108.550622506313,-1.98579734972971,-12.0551717888559));
#57574=CARTESIAN_POINT('Ctrl Pts',(108.487405157811,-1.95442030405157,-12.1733202167919));
#57575=CARTESIAN_POINT('Ctrl Pts',(108.424880007573,-1.9194031665709,-12.290556812487));
#57576=CARTESIAN_POINT('Ctrl Pts',(108.391821388282,-1.90088872538617,-12.3525427488559));
#57577=CARTESIAN_POINT('Ctrl Pts',(108.35895627321,-1.88135746538499,-12.4142734666444));
#57578=CARTESIAN_POINT('Ctrl Pts',(108.326343655004,-1.8607876783373,-12.47563157783));
#57579=CARTESIAN_POINT('',(108.090753740172,-1.68967307116025,11.4740625043632));
#57580=CARTESIAN_POINT('Ctrl Pts',(108.090753740172,-1.68975055635687,11.4740963971941));
#57581=CARTESIAN_POINT('Ctrl Pts',(108.114645770858,-2.63984049686771,11.3346921771064));
#57582=CARTESIAN_POINT('Ctrl Pts',(108.201079609567,-6.01700224455775,10.4067268014638));
#57583=CARTESIAN_POINT('Ctrl Pts',(108.318784352286,-9.75406870916728,7.13233250087535));
#57584=CARTESIAN_POINT('Ctrl Pts',(108.475138872343,-12.0218124932882,1.17211559965207));
#57585=CARTESIAN_POINT('Ctrl Pts',(108.600222488388,-11.3799046098746,-4.06613609701905));
#57586=CARTESIAN_POINT('Ctrl Pts',(108.753156703682,-7.79634378044959,-9.17264673778085));
#57587=CARTESIAN_POINT('Ctrl Pts',(108.843549110953,-4.45036163137592,-10.9662005008345));
#57588=CARTESIAN_POINT('Ctrl Pts',(108.902670614213,-2.1172167588623,-11.4024697825115));
#57589=CARTESIAN_POINT('',(107.482029246699,-0.87623857414724,12.583168122964));
#57590=CARTESIAN_POINT('Ctrl Pts',(107.482029246699,-0.87623857414724,12.583168122964));
#57591=CARTESIAN_POINT('Ctrl Pts',(107.482394382578,-0.877079479290065,
12.5825107576108));
#57592=CARTESIAN_POINT('Ctrl Pts',(107.482759857299,-0.877919727242279,
12.5818527375208));
#57593=CARTESIAN_POINT('Ctrl Pts',(107.483125668906,-0.87875931790496,12.5811940664401));
#57594=CARTESIAN_POINT('Ctrl Pts',(107.50706618734,-0.933706277910721,12.5380873775059));
#57595=CARTESIAN_POINT('Ctrl Pts',(107.532594415577,-0.986211055902737,
12.491930905356));
#57596=CARTESIAN_POINT('Ctrl Pts',(107.559298891057,-1.03624927992292,12.4435191439929));
#57597=CARTESIAN_POINT('Ctrl Pts',(107.586988876219,-1.08813412902446,12.3933207809964));
#57598=CARTESIAN_POINT('Ctrl Pts',(107.615943527723,-1.13736712243412,12.3406977585454));
#57599=CARTESIAN_POINT('Ctrl Pts',(107.645704126984,-1.18397787806622,12.2865272927665));
#57600=CARTESIAN_POINT('Ctrl Pts',(107.671575494813,-1.22449735797087,12.2394360351848));
#57601=CARTESIAN_POINT('Ctrl Pts',(107.698055925798,-1.2630362708689,12.19117525119));
#57602=CARTESIAN_POINT('Ctrl Pts',(107.724844064182,-1.29964537358992,12.1423150531443));
#57603=CARTESIAN_POINT('Ctrl Pts',(107.762653981563,-1.35131701756271,12.0733516923896));
#57604=CARTESIAN_POINT('Ctrl Pts',(107.801780392181,-1.40010211706753,12.0019112292348));
#57605=CARTESIAN_POINT('Ctrl Pts',(107.841816435641,-1.44606245484022,11.9287853832026));
#57606=CARTESIAN_POINT('Ctrl Pts',(107.883429900903,-1.49383363186028,11.8527783757514));
#57607=CARTESIAN_POINT('Ctrl Pts',(107.926026090234,-1.53855319806583,11.7749507224119));
#57608=CARTESIAN_POINT('Ctrl Pts',(107.969148132621,-1.58034682115879,11.6961777693696));
#57609=CARTESIAN_POINT('Ctrl Pts',(108.009349694466,-1.61930993214651,11.6227397880442));
#57610=CARTESIAN_POINT('Ctrl Pts',(108.050008293574,-1.65573088360539,11.5484801021652));
#57611=CARTESIAN_POINT('Ctrl Pts',(108.090753740172,-1.68975055635671,11.4740963971942));
#57612=CARTESIAN_POINT('Ctrl Pts',(108.326343655004,-1.86078767833722,-12.47563157783));
#57613=CARTESIAN_POINT('Ctrl Pts',(108.263801846982,-4.56292341074069,-12.0725978039739));
#57614=CARTESIAN_POINT('Ctrl Pts',(108.201260038959,-7.11575393062732,-10.7578107113292));
#57615=CARTESIAN_POINT('Ctrl Pts',(108.138718230937,-9.02927368304341,-8.80539603771879));
#57616=CARTESIAN_POINT('Ctrl Pts',(108.107447326925,-9.98603355925145,-7.82918870091359));
#57617=CARTESIAN_POINT('Ctrl Pts',(108.076176422914,-10.7829657435919,-6.69357446886696));
#57618=CARTESIAN_POINT('Ctrl Pts',(108.044905518903,-11.3724323332148,-5.46173634297509));
#57619=CARTESIAN_POINT('Ctrl Pts',(107.98236371088,-12.5513655124606,-2.99806009119129));
#57620=CARTESIAN_POINT('Ctrl Pts',(107.919821902858,-12.9004363128364,-0.149488264026472));
#57621=CARTESIAN_POINT('Ctrl Pts',(107.857280094835,-12.3590846387935,2.52866392373924));
#57622=CARTESIAN_POINT('Ctrl Pts',(107.826009190824,-12.088408801772,3.86774001762206));
#57623=CARTESIAN_POINT('Ctrl Pts',(107.794738286812,-11.5951273461459,5.16421120165511));
#57624=CARTESIAN_POINT('Ctrl Pts',(107.763467382801,-10.9063357466975,6.34390013524507));
#57625=CARTESIAN_POINT('Ctrl Pts',(107.700925574779,-9.52875254780069,8.703278002425));
#57626=CARTESIAN_POINT('Ctrl Pts',(107.638383766756,-7.36912877361468,10.5955268678326));
#57627=CARTESIAN_POINT('Ctrl Pts',(107.575841958733,-4.84909213365347,11.646997915129));
#57628=CARTESIAN_POINT('Ctrl Pts',(107.544571054722,-3.58907381367288,12.1727334387771));
#57629=CARTESIAN_POINT('Ctrl Pts',(107.513300150711,-2.23895227724849,12.4882745078976));
#57630=CARTESIAN_POINT('Ctrl Pts',(107.482029246699,-0.876238574147329,
12.583168122964));
#57631=CARTESIAN_POINT('Origin',(93.0806848796603,0.,0.));
#57632=CARTESIAN_POINT('Ctrl Pts',(110.814071804302,1.76443058609261,-11.4626366197512));
#57633=CARTESIAN_POINT('Ctrl Pts',(110.901035745034,1.69966359360912,-11.472606129062));
#57634=CARTESIAN_POINT('Ctrl Pts',(110.98193435915,1.62933547807125,-11.4828589976618));
#57635=CARTESIAN_POINT('Ctrl Pts',(111.100478831822,1.5107910053991,-11.4989048142971));
#57636=CARTESIAN_POINT('Ctrl Pts',(111.144081499747,1.46329723353908,-11.5050660129585));
#57637=CARTESIAN_POINT('Ctrl Pts',(111.185928218469,1.41338106757117,-11.5111948783535));
#57638=CARTESIAN_POINT('Ctrl Pts',(111.683757644765,-0.266838057499402,
11.5945698937334));
#57639=CARTESIAN_POINT('Ctrl Pts',(111.694737994272,-0.176976729613362,
11.5966379671848));
#57640=CARTESIAN_POINT('Ctrl Pts',(111.7,-0.0875694530144953,11.59764));
#57641=CARTESIAN_POINT('Ctrl Pts',(111.7,0.122714157654495,11.59764));
#57642=CARTESIAN_POINT('Ctrl Pts',(111.689602674459,0.249054699568216,11.5956523517617));
#57643=CARTESIAN_POINT('Ctrl Pts',(111.667770384747,0.375195361129816,11.5915694369049));
#57644=CARTESIAN_POINT('Origin',(93.0806848796603,0.,0.));
#57645=CARTESIAN_POINT('Origin',(96.446025,0.,0.));
#57646=CARTESIAN_POINT('Origin',(93.0806848796603,0.,0.));
#57647=CARTESIAN_POINT('Ctrl Pts',(109.916925613585,-2.16013264239418,11.3946952805621));
#57648=CARTESIAN_POINT('Ctrl Pts',(110.044752529268,-2.13546086335257,11.3993723968817));
#57649=CARTESIAN_POINT('Ctrl Pts',(110.171957681553,-2.09901013524074,11.4062154433825));
#57650=CARTESIAN_POINT('Ctrl Pts',(110.294852708433,-2.05139200834394,11.4147730769255));
#57651=CARTESIAN_POINT('Ctrl Pts',(111.113306560609,-1.49574126823374,-11.5007830876033));
#57652=CARTESIAN_POINT('Ctrl Pts',(111.094345708019,-1.51619244420004,-11.4981232976009));
#57653=CARTESIAN_POINT('Ctrl Pts',(111.075107334507,-1.5361625027139,-11.4954706061514));
#57654=CARTESIAN_POINT('Ctrl Pts',(110.957135649226,-1.6541341879949,-11.4795023202626));
#57655=CARTESIAN_POINT('Ctrl Pts',(110.845701752448,-1.74655296335327,-11.465670048636));
#57656=CARTESIAN_POINT('Ctrl Pts',(110.724270236999,-1.82788467546432,-11.4526892554894));
#57657=CARTESIAN_POINT('Origin',(93.0806848796603,0.,0.));
#57658=CARTESIAN_POINT('Ctrl Pts',(109.281532350295,-2.18912582690723,-11.3891607102353));
#57659=CARTESIAN_POINT('Ctrl Pts',(109.155412564872,-2.17653948181738,-11.3915799484745));
#57660=CARTESIAN_POINT('Ctrl Pts',(109.027830981515,-2.15266538708709,-11.3961649260526));
#57661=CARTESIAN_POINT('Ctrl Pts',(108.902670614213,-2.1173562772654,-11.4027214280068));
#57662=CARTESIAN_POINT('Ctrl Pts',(108.090753740172,-1.68938597696385,11.4739369263753));
#57663=CARTESIAN_POINT('Ctrl Pts',(108.20790113293,-1.78710759140999,11.4595487066952));
#57664=CARTESIAN_POINT('Ctrl Pts',(108.33848779035,-1.87501865749023,11.44530766719));
#57665=CARTESIAN_POINT('Ctrl Pts',(108.477958351107,-1.94818655881029,11.4328396604549));
#57666=CARTESIAN_POINT('Origin',(93.0806848796603,0.,0.));
#57667=CARTESIAN_POINT('',(109.009389146813,2.14465603270175,-11.397646135533));
#57668=CARTESIAN_POINT('Ctrl Pts',(109.009389146813,2.14459809538638,-11.3976292525624));
#57669=CARTESIAN_POINT('Ctrl Pts',(109.136652663705,2.17371164479049,-11.3921511955719));
#57670=CARTESIAN_POINT('Ctrl Pts',(109.265320582609,2.19108690692555,-11.3887853615113));
#57671=CARTESIAN_POINT('Ctrl Pts',(109.391405608182,2.19731819681761,-11.3875829881294));
#57672=CARTESIAN_POINT('',(109.808269534075,2.1782830168169,11.391215608372));
#57673=CARTESIAN_POINT('Ctrl Pts',(109.009389146813,2.14467064967058,-11.3976503949269));
#57674=CARTESIAN_POINT('Ctrl Pts',(109.036249487207,3.2052865345203,-11.1982841745728));
#57675=CARTESIAN_POINT('Ctrl Pts',(109.12332934527,6.55809015436484,-10.0745075843251));
#57676=CARTESIAN_POINT('Ctrl Pts',(109.240518962169,10.069373101794,-6.61415923889863));
#57677=CARTESIAN_POINT('Ctrl Pts',(109.391067756344,12.0167660168964,-0.799058821012281));
#57678=CARTESIAN_POINT('Ctrl Pts',(109.511506791684,11.2878420523094,4.21258051924178));
#57679=CARTESIAN_POINT('Ctrl Pts',(109.660610637206,7.77769110684894,9.17022383928472));
#57680=CARTESIAN_POINT('Ctrl Pts',(109.749494965058,4.49625225668538,10.9466376677334));
#57681=CARTESIAN_POINT('Ctrl Pts',(109.808269534075,2.17827022429556,11.3911929596074));
#57682=CARTESIAN_POINT('Ctrl Pts',(110.191221970063,2.0885909575843,11.4080253059632));
#57683=CARTESIAN_POINT('Ctrl Pts',(110.065692123374,2.13013522819152,11.4004193456324));
#57684=CARTESIAN_POINT('Ctrl Pts',(109.936720884488,2.16011691071928,11.3947132932223));
#57685=CARTESIAN_POINT('Ctrl Pts',(109.808269534075,2.1782951807231,11.3912371441928));
#57686=CARTESIAN_POINT('Origin',(117.38636,1.35008033100152E-15,0.));
#57687=CARTESIAN_POINT('',(117.38636,-12.6136400000002,-1.54472538515972E-15));
#57688=CARTESIAN_POINT('Origin',(117.38636,0.,0.));
#57689=CARTESIAN_POINT('Origin',(117.38636,0.,0.));
#57690=CARTESIAN_POINT('Origin',(96.446025,-1.35008033100152E-15,0.));
#57691=CARTESIAN_POINT('',(96.446025,1.68935314532052,-12.4999999999999));
#57692=CARTESIAN_POINT('',(96.4460250000001,-1.68935314532052,-12.4999999999999));
#57693=CARTESIAN_POINT('',(96.446025,-1.35,-12.5));
#57694=CARTESIAN_POINT('Origin',(96.446025,0.,0.));
#57695=CARTESIAN_POINT('',(96.4460250000001,-12.6136400000002,-1.54472538515972E-15));
#57696=CARTESIAN_POINT('Origin',(96.446025,0.,0.));
#57697=CARTESIAN_POINT('Origin',(96.446025,0.,0.));
#57698=CARTESIAN_POINT('Ctrl Pts',(108.413053017993,1.91273266775695,-12.4677731689061));
#57699=CARTESIAN_POINT('Ctrl Pts',(108.443162776828,3.21281350456061,-12.2683223885951));
#57700=CARTESIAN_POINT('Ctrl Pts',(108.533492053333,7.02671572005891,-11.0614285744525));
#57701=CARTESIAN_POINT('Ctrl Pts',(108.653931088672,10.9514907629236,-7.19358624186833));
#57702=CARTESIAN_POINT('Ctrl Pts',(108.804479882847,13.0694831449644,-0.86905959376855));
#57703=CARTESIAN_POINT('Ctrl Pts',(108.924918918187,12.2767025036725,4.58161954852267));
#57704=CARTESIAN_POINT('Ctrl Pts',(109.075467712362,8.42205173022918,10.0258252123201));
#57705=CARTESIAN_POINT('Ctrl Pts',(109.165796988867,4.77376444645626,11.9680846522454));
#57706=CARTESIAN_POINT('Ctrl Pts',(109.226016506537,2.18287265897621,12.4233240722559));
#57707=CARTESIAN_POINT('Ctrl Pts',(108.608582309158,1.86137724641834,-12.1330229160156));
#57708=CARTESIAN_POINT('Ctrl Pts',(108.638692067993,3.12655189885353,-11.9389272378743));
#57709=CARTESIAN_POINT('Ctrl Pts',(108.729021344498,6.83805373267649,-10.7644376072233));
#57710=CARTESIAN_POINT('Ctrl Pts',(108.849460379838,10.6574515425471,-7.0004439075451));
#57711=CARTESIAN_POINT('Ctrl Pts',(109.000009174013,12.7185774356084,-0.845726002849796));
#57712=CARTESIAN_POINT('Ctrl Pts',(109.120448209353,11.9470823532181,4.45860653876238));
#57713=CARTESIAN_POINT('Ctrl Pts',(109.270997003527,8.19592602932356,9.75663940986822));
#57714=CARTESIAN_POINT('Ctrl Pts',(109.361326280032,4.64559249192662,11.646750657018));
#57715=CARTESIAN_POINT('Ctrl Pts',(109.421545797702,2.12426418377211,12.0897672438963));
#57716=CARTESIAN_POINT('Ctrl Pts',(108.804111600324,1.81002182507974,-11.7982726631251));
#57717=CARTESIAN_POINT('Ctrl Pts',(108.834221359159,3.04029029314645,-11.6095320871536));
#57718=CARTESIAN_POINT('Ctrl Pts',(108.924550635664,6.64939174529407,-10.467446639994));
#57719=CARTESIAN_POINT('Ctrl Pts',(109.044989671003,10.3634123221706,-6.80730157322186));
#57720=CARTESIAN_POINT('Ctrl Pts',(109.195538465178,12.3676717262524,-0.822392411931035));
#57721=CARTESIAN_POINT('Ctrl Pts',(109.315977500518,11.6174622027638,4.33559352900208));
#57722=CARTESIAN_POINT('Ctrl Pts',(109.466526294693,7.96980032841795,9.48745360741635));
#57723=CARTESIAN_POINT('Ctrl Pts',(109.556855571198,4.51742053739697,11.3254166617906));
#57724=CARTESIAN_POINT('Ctrl Pts',(109.617075088868,2.06565570856801,11.7562104155366));
#57725=CARTESIAN_POINT('Ctrl Pts',(108.999640891489,1.75866640374113,-11.4635224102347));
#57726=CARTESIAN_POINT('Ctrl Pts',(109.029750650324,2.95402868743937,-11.2801369364328));
#57727=CARTESIAN_POINT('Ctrl Pts',(109.120079926829,6.46072975791164,-10.1704556727648));
#57728=CARTESIAN_POINT('Ctrl Pts',(109.240518962169,10.069373101794,-6.61415923889863));
#57729=CARTESIAN_POINT('Ctrl Pts',(109.391067756344,12.0167660168964,-0.799058821012281));
#57730=CARTESIAN_POINT('Ctrl Pts',(109.511506791684,11.2878420523094,4.21258051924178));
#57731=CARTESIAN_POINT('Ctrl Pts',(109.662055585858,7.74367462751234,9.21826780496448));
#57732=CARTESIAN_POINT('Ctrl Pts',(109.752384862363,4.38924858286732,11.0040826665632));
#57733=CARTESIAN_POINT('Ctrl Pts',(109.812604380033,2.00704723336391,11.4226535871769));
#57734=CARTESIAN_POINT('',(108.413053017993,1.91273266775704,-12.4677731689061));
#57735=CARTESIAN_POINT('Ctrl Pts',(108.413053017993,1.91273266775695,-12.4677731689061));
#57736=CARTESIAN_POINT('Ctrl Pts',(108.413855852925,1.9131888940879,-12.4663232667956));
#57737=CARTESIAN_POINT('Ctrl Pts',(108.414658783089,1.91364450647225,-12.4648732233092));
#57738=CARTESIAN_POINT('Ctrl Pts',(108.415461807794,1.91409950547309,-12.4634230398033));
#57739=CARTESIAN_POINT('Ctrl Pts',(108.479752286689,1.9505269073821,-12.3473207685653));
#57740=CARTESIAN_POINT('Ctrl Pts',(108.544861582718,1.98314984730452,-12.229936946399));
#57741=CARTESIAN_POINT('Ctrl Pts',(108.610394801366,2.01212814785511,-12.1120411801108));
#57742=CARTESIAN_POINT('Ctrl Pts',(108.644839096371,2.02735915822723,-12.0500751018714));
#57743=CARTESIAN_POINT('Ctrl Pts',(108.679400502512,2.04158417778305,-11.9879672915395));
#57744=CARTESIAN_POINT('Ctrl Pts',(108.714021681,2.05483173131018,-11.9258274377091));
#57745=CARTESIAN_POINT('Ctrl Pts',(108.782570306368,2.08106138678214,-11.8027928748588));
#57746=CARTESIAN_POINT('Ctrl Pts',(108.85175216169,2.10360807176127,-11.6789176806214));
#57747=CARTESIAN_POINT('Ctrl Pts',(108.921251264686,2.12256886627832,-11.5548280565426));
#57748=CARTESIAN_POINT('Ctrl Pts',(108.950581971157,2.13057089039742,-11.5024585124332));
#57749=CARTESIAN_POINT('Ctrl Pts',(108.979969182396,2.1379348534859,-11.4500505742848));
#57750=CARTESIAN_POINT('Ctrl Pts',(109.009389146813,2.1446706496705,-11.397650394927));
#57751=CARTESIAN_POINT('',(109.226016506537,2.1828726589771,12.4233240722558));
#57752=CARTESIAN_POINT('Ctrl Pts',(109.226016506537,2.18287265897622,12.4233240722559));
#57753=CARTESIAN_POINT('Ctrl Pts',(109.165796988867,4.77376444645624,11.9680846522455));
#57754=CARTESIAN_POINT('Ctrl Pts',(109.105577471197,7.20595596897156,10.6732450256285));
#57755=CARTESIAN_POINT('Ctrl Pts',(109.045357953527,9.04459334939484,8.7898436397436));
#57756=CARTESIAN_POINT('Ctrl Pts',(109.015248194692,9.96391203960649,7.84814294680113));
#57757=CARTESIAN_POINT('Ctrl Pts',(108.985138435857,10.7348421942951,6.75930181404173));
#57758=CARTESIAN_POINT('Ctrl Pts',(108.955028677022,11.3148606841952,5.57918446367781));
#57759=CARTESIAN_POINT('Ctrl Pts',(108.894809159352,12.4748976639954,3.21894976294992));
#57760=CARTESIAN_POINT('Ctrl Pts',(108.834589641682,12.8712879846414,0.493610191804197));
#57761=CARTESIAN_POINT('Ctrl Pts',(108.774370124012,12.4386201229791,-2.10137677140434));
#57762=CARTESIAN_POINT('Ctrl Pts',(108.744260365177,12.222286192148,-3.39887025300854));
#57763=CARTESIAN_POINT('Ctrl Pts',(108.714150606342,11.7986877157399,-4.66377558262845));
#57764=CARTESIAN_POINT('Ctrl Pts',(108.684040847507,11.1892241445624,-5.82936599675708));
#57765=CARTESIAN_POINT('Ctrl Pts',(108.623821329837,9.9702970022074,-8.16054682501441));
#57766=CARTESIAN_POINT('Ctrl Pts',(108.563601812167,8.00790948077504,-10.0944679913065));
#57767=CARTESIAN_POINT('Ctrl Pts',(108.503382294498,5.65871265563164,-11.2755056308006));
#57768=CARTESIAN_POINT('Ctrl Pts',(108.473272535663,4.48411424306014,-11.8660244505475));
#57769=CARTESIAN_POINT('Ctrl Pts',(108.443162776828,3.21281350456093,-12.268322388595));
#57770=CARTESIAN_POINT('Ctrl Pts',(108.413053017993,1.91273266775748,-12.467773168906));
#57771=CARTESIAN_POINT('Ctrl Pts',(109.808269534075,2.17827022429548,11.3911929596074));
#57772=CARTESIAN_POINT('Ctrl Pts',(109.743176121344,2.18748537356643,11.5047642900023));
#57773=CARTESIAN_POINT('Ctrl Pts',(109.678142238689,2.19372201690515,11.6188991359825));
#57774=CARTESIAN_POINT('Ctrl Pts',(109.613368850412,2.19706582260749,11.7331774438013));
#57775=CARTESIAN_POINT('Ctrl Pts',(109.581094983429,2.1987319009666,11.7901175391662));
#57776=CARTESIAN_POINT('Ctrl Pts',(109.548885787082,2.1996805463104,11.8470929825011));
#57777=CARTESIAN_POINT('Ctrl Pts',(109.516766120282,2.19992700252409,11.9040503705732));
#57778=CARTESIAN_POINT('Ctrl Pts',(109.447893339496,2.20045546768175,12.0261815784489));
#57779=CARTESIAN_POINT('Ctrl Pts',(109.379164341258,2.19775214763542,12.1487063361486));
#57780=CARTESIAN_POINT('Ctrl Pts',(109.310802500265,2.1918507117029,12.2711579454467));
#57781=CARTESIAN_POINT('Ctrl Pts',(109.28247214663,2.18940505247996,12.3219040538631));
#57782=CARTESIAN_POINT('Ctrl Pts',(109.254204849311,2.18641072181222,12.3726374129757));
#57783=CARTESIAN_POINT('Ctrl Pts',(109.226016506537,2.18287265897719,12.4233240722558));
#57784=CARTESIAN_POINT('Origin',(118.5,-2.7,-12.5));
#57785=CARTESIAN_POINT('',(108.090714382958,-1.68935314531923,-12.5));
#57786=CARTESIAN_POINT('Origin',(109.5,0.,-12.5));
#57787=CARTESIAN_POINT('',(106.9,-1.68935314531923,-12.5));
#57788=CARTESIAN_POINT('Origin',(118.5,-2.7,-12.5));
#57789=CARTESIAN_POINT('',(106.9,-1.68935314531923,-12.5));
#57790=CARTESIAN_POINT('',(106.9,1.68935314531923,-12.5));
#57791=CARTESIAN_POINT('Origin',(118.5,-2.7,-12.5));
#57792=CARTESIAN_POINT('',(106.9,1.68935314531923,-12.5));
#57793=CARTESIAN_POINT('',(106.9,-1.68935314531923,-12.5));
#57794=CARTESIAN_POINT('Origin',(118.5,-2.7,-12.5));
#57795=CARTESIAN_POINT('',(106.9,1.68935314531923,-12.5));
#57796=CARTESIAN_POINT('',(106.9,-1.68935314531923,-12.5));
#57797=CARTESIAN_POINT('Origin',(118.5,-2.7,-12.5));
#57798=CARTESIAN_POINT('',(106.9,1.68935314531923,-12.5));
#57799=CARTESIAN_POINT('',(106.9,-1.68935314531923,-12.5));
#57800=CARTESIAN_POINT('Origin',(118.5,-2.7,-12.5));
#57801=CARTESIAN_POINT('',(106.9,1.68935314531923,-12.5));
#57802=CARTESIAN_POINT('',(106.9,-1.68935314531923,-12.5));
#57803=CARTESIAN_POINT('Origin',(118.5,-2.7,-12.5));
#57804=CARTESIAN_POINT('',(106.9,1.68935314531923,-12.5));
#57805=CARTESIAN_POINT('',(106.9,-1.68935314531923,-12.5));
#57806=CARTESIAN_POINT('Origin',(118.5,-2.7,-12.5));
#57807=CARTESIAN_POINT('',(106.9,-1.68935314531923,-12.5));
#57808=CARTESIAN_POINT('',(106.9,1.68935314531923,-12.5));
#57809=CARTESIAN_POINT('Origin',(118.5,-2.7,-12.5));
#57810=CARTESIAN_POINT('',(106.9,-1.68935314531923,-12.5));
#57811=CARTESIAN_POINT('',(106.9,1.68935314531923,-12.5));
#57812=CARTESIAN_POINT('Origin',(118.5,-2.7,-12.5));
#57813=CARTESIAN_POINT('',(117.38636,1.68935314532054,-12.4999999999999));
#57814=CARTESIAN_POINT('',(106.9,1.68935314531923,-12.5));
#57815=CARTESIAN_POINT('',(117.38636,-1.68935314532053,-12.4999999999999));
#57816=CARTESIAN_POINT('Ctrl Pts',(117.38636,-1.68935314532052,-12.5));
#57817=CARTESIAN_POINT('Ctrl Pts',(117.61261618375,-5.55111512312578E-16,
-12.5));
#57818=CARTESIAN_POINT('Ctrl Pts',(117.38636,1.68935314532052,-12.5));
#57819=CARTESIAN_POINT('',(106.9,-1.68935314531923,-12.5));
#57820=CARTESIAN_POINT('Origin',(118.5,-2.7,-12.5));
#57821=CARTESIAN_POINT('Origin',(109.5,0.,-12.5));
#57822=CARTESIAN_POINT('',(106.9,1.68935314531923,-12.5));
#57823=CARTESIAN_POINT('',(106.9,-1.68935314531923,-12.5));
#57824=CARTESIAN_POINT('Origin',(106.9,0.,0.));
#57825=CARTESIAN_POINT('Origin',(106.9,0.,0.));
#57826=CARTESIAN_POINT('Ctrl Pts',(110.869631627566,-1.72165885261004,12.4955914163688));
#57827=CARTESIAN_POINT('Ctrl Pts',(110.935695199159,-1.66910328566579,12.5028325908013));
#57828=CARTESIAN_POINT('Ctrl Pts',(110.997867695831,-1.61340214138951,12.5101653135727));
#57829=CARTESIAN_POINT('Ctrl Pts',(111.078972847973,-1.53229698924803,12.5202449280198));
#57830=CARTESIAN_POINT('Ctrl Pts',(111.101974334193,-1.50824419914058,12.5231678926488));
#57831=CARTESIAN_POINT('Ctrl Pts',(111.124564900463,-1.48350560638761,12.5260977628875));
#57832=CARTESIAN_POINT('Origin',(106.9,0.,0.));
#57833=CARTESIAN_POINT('Origin',(106.9,0.,0.));
#57834=CARTESIAN_POINT('Origin',(117.38636,0.,0.));
#57835=CARTESIAN_POINT('Origin',(106.9,0.,0.));
#57836=CARTESIAN_POINT('Origin',(117.38636,0.,0.));
#57837=CARTESIAN_POINT('Origin',(106.9,0.,0.));
#57838=CARTESIAN_POINT('Ctrl Pts',(111.05480378529,1.55646560811611,12.5172412639667));
#57839=CARTESIAN_POINT('Ctrl Pts',(110.974324957434,1.63685850952933,12.5072447492757));
#57840=CARTESIAN_POINT('Ctrl Pts',(110.885269102117,1.71321337314212,12.4969493815617));
#57841=CARTESIAN_POINT('Ctrl Pts',(110.7891485355,1.78272152996985,12.4870259868466));
#57842=CARTESIAN_POINT('Ctrl Pts',(110.231099956476,2.07496815725955,-12.4418013645918));
#57843=CARTESIAN_POINT('Ctrl Pts',(110.146193941075,2.10488417498088,-12.4368121526325));
#57844=CARTESIAN_POINT('Ctrl Pts',(110.059563366867,2.12952031953925,-12.4325956901));
#57845=CARTESIAN_POINT('Ctrl Pts',(109.972381969055,2.14868687232742,-12.4292823113118));
#57846=CARTESIAN_POINT('Origin',(106.9,0.,0.));
#57847=CARTESIAN_POINT('Origin',(106.9,0.,0.));
#57848=CARTESIAN_POINT('Origin',(106.9,0.,0.));
#57849=CARTESIAN_POINT('Origin',(106.9,0.,0.));
#57850=CARTESIAN_POINT('Origin',(106.9,0.,0.));
#57851=CARTESIAN_POINT('Origin',(106.9,0.,0.));
#57852=CARTESIAN_POINT('Origin',(96.446025,0.,0.));
#57853=CARTESIAN_POINT('Origin',(106.9,0.,0.));
#57854=CARTESIAN_POINT('',(107.3,2.69422295812418E-16,12.61364));
#57855=CARTESIAN_POINT('Ctrl Pts',(107.3,2.08166817117217E-16,12.61364));
#57856=CARTESIAN_POINT('Ctrl Pts',(107.3,-0.276841916654518,12.61364));
#57857=CARTESIAN_POINT('Ctrl Pts',(107.35544265574,-0.571753236528152,12.6036005699437));
#57858=CARTESIAN_POINT('Ctrl Pts',(107.472444208643,-0.853911663388667,
12.5847079999432));
#57859=CARTESIAN_POINT('Ctrl Pts',(107.477190873565,-0.865095837719748,
12.583944055971));
#57860=CARTESIAN_POINT('Ctrl Pts',(107.482029246699,-0.876238574147231,
12.583168122964));
#57861=CARTESIAN_POINT('Ctrl Pts',(107.444020192937,0.782909338907701,12.5893195613048));
#57862=CARTESIAN_POINT('Ctrl Pts',(107.347281269023,0.528865525353306,12.6051181335116));
#57863=CARTESIAN_POINT('Ctrl Pts',(107.3,0.256601073912259,12.61364));
#57864=CARTESIAN_POINT('Ctrl Pts',(107.3,1.17961196366423E-15,12.61364));
#57865=CARTESIAN_POINT('Ctrl Pts',(108.090714382958,-1.68935314531923,-12.5));
#57866=CARTESIAN_POINT('Ctrl Pts',(108.164345299838,-1.75077724271102,-12.4916986406298));
#57867=CARTESIAN_POINT('Ctrl Pts',(108.243231824376,-1.80836647601685,-12.4834503986049));
#57868=CARTESIAN_POINT('Ctrl Pts',(108.326343655004,-1.86078767833678,-12.47563157783));
#57869=CARTESIAN_POINT('Origin',(106.9,0.,0.));
#57870=CARTESIAN_POINT('Ctrl Pts',(109.873072103706,-2.1681368050555,-12.4259042666586));
#57871=CARTESIAN_POINT('Ctrl Pts',(109.960853831938,-2.15303217054067,-12.428539802336));
#57872=CARTESIAN_POINT('Ctrl Pts',(110.048551732082,-2.13242381263147,-12.4321108515432));
#57873=CARTESIAN_POINT('Ctrl Pts',(110.134936209547,-2.10638458259799,-12.4365211389598));
#57874=CARTESIAN_POINT('Ctrl Pts',(109.065424143322,-2.156651067,12.4279028892572));
#57875=CARTESIAN_POINT('Ctrl Pts',(109.152578695929,-2.17421314041195,12.4248552902616));
#57876=CARTESIAN_POINT('Ctrl Pts',(109.240090470105,-2.18632008331947,12.4227197843719));
#57877=CARTESIAN_POINT('Ctrl Pts',(109.326702434851,-2.19316391405513,12.4215114255748));
#57878=CARTESIAN_POINT('Origin',(109.5,0.,15.));
#57879=CARTESIAN_POINT('Ctrl Pts',(109.226016506445,2.1828726589656,12.4233240722578));
#57880=CARTESIAN_POINT('Ctrl Pts',(109.139566669173,2.17202189846165,12.4252306335207));
#57881=CARTESIAN_POINT('Ctrl Pts',(109.05272927934,2.15587790155921,12.4280561642703));
#57882=CARTESIAN_POINT('Ctrl Pts',(108.966713351646,2.13438641081873,12.4317460036357));
#57883=CARTESIAN_POINT('',(107.3,2.69422295812418E-16,15.));
#57884=CARTESIAN_POINT('Ctrl Pts',(108.413053017994,1.91273266775782,-12.467773168906));
#57885=CARTESIAN_POINT('Ctrl Pts',(108.319914928113,1.85980516387165,-12.4758929962669));
#57886=CARTESIAN_POINT('Ctrl Pts',(108.23126343941,1.80036107420324,-12.4846642863292));
#57887=CARTESIAN_POINT('Ctrl Pts',(108.14853343171,1.73595452555452,-12.4936134058489));
#57888=CARTESIAN_POINT('Origin',(-13.25,0.,0.));
#57889=CARTESIAN_POINT('',(-12.5,-21.8313,-2.67356316662256E-15));
#57890=CARTESIAN_POINT('Origin',(-12.5,0.,0.));
#57891=CARTESIAN_POINT('',(-13.25,-23.61565,-2.89208301822842E-15));
#57892=CARTESIAN_POINT('Origin',(1.7825,0.,0.));
#57893=CARTESIAN_POINT('',(16.065,-21.8313,-2.67356316662256E-15));
#57894=CARTESIAN_POINT('Origin',(16.065,0.,0.));
#57895=CARTESIAN_POINT('',(1.7825,-21.8313,-2.67356316662256E-15));
#57896=CARTESIAN_POINT('Origin',(16.065,17.97,0.));
#57897=CARTESIAN_POINT('',(16.065,-17.97,-2.20069029806779E-15));
#57898=CARTESIAN_POINT('Origin',(16.065,0.,0.));
#57899=CARTESIAN_POINT('Origin',(16.315,0.,0.));
#57900=CARTESIAN_POINT('',(16.565,-17.47,-2.13945795811043E-15));
#57901=CARTESIAN_POINT('Origin',(16.565,0.,0.));
#57902=CARTESIAN_POINT('',(16.315,-17.72,-2.17007412808911E-15));
#57903=CARTESIAN_POINT('Origin',(25.7825,0.,0.));
#57904=CARTESIAN_POINT('',(35.,-17.47,-2.13945795811043E-15));
#57905=CARTESIAN_POINT('Origin',(35.,0.,0.));
#57906=CARTESIAN_POINT('',(25.7825,-17.47,-2.13945795811043E-15));
#57907=CARTESIAN_POINT('Origin',(37.5,0.,0.));
#57908=CARTESIAN_POINT('',(40.,-13.97,-1.71083157840885E-15));
#57909=CARTESIAN_POINT('Origin',(40.,0.,0.));
#57910=CARTESIAN_POINT('',(37.5,-15.72,-1.92514476825964E-15));
#57911=CARTESIAN_POINT('Origin',(40.25,0.,0.));
#57912=CARTESIAN_POINT('',(40.5,-13.47,-1.64959923845148E-15));
#57913=CARTESIAN_POINT('Origin',(40.5,0.,0.));
#57914=CARTESIAN_POINT('',(40.25,-13.72,-1.68021540843017E-15));
#57915=CARTESIAN_POINT('Origin',(86.,0.,-14.25));
#57916=CARTESIAN_POINT('',(86.,2.7,-13.1966245684266));
#57917=CARTESIAN_POINT('',(86.,-2.7,-13.1966245684266));
#57918=CARTESIAN_POINT('Origin',(86.,0.,0.));
#57919=CARTESIAN_POINT('',(86.,2.7,-12.5));
#57920=CARTESIAN_POINT('',(86.,-2.7,-16.));
#57921=CARTESIAN_POINT('Origin',(118.5,-2.7,-16.));
#57922=CARTESIAN_POINT('',(95.,-2.7,-13.1966245684266));
#57923=CARTESIAN_POINT('',(95.,-2.7,-8.));
#57924=CARTESIAN_POINT('',(67.75,-2.7,-13.1966245684266));
#57925=CARTESIAN_POINT('Origin',(67.75,0.,0.));
#57926=CARTESIAN_POINT('',(95.,2.7,-13.1966245684266));
#57927=CARTESIAN_POINT('',(67.75,2.7,-13.1966245684266));
#57928=CARTESIAN_POINT('',(95.,-13.47,-1.64959923845148E-15));
#57929=CARTESIAN_POINT('Origin',(95.,0.,0.));
#57930=CARTESIAN_POINT('',(67.75,-13.47,-1.64959923845148E-15));
#57931=CARTESIAN_POINT('Origin',(95.,0.,0.));
#57932=CARTESIAN_POINT('Origin',(118.5,2.7,-12.5));
#57933=CARTESIAN_POINT('',(95.,2.7,-6.25));
#57934=CARTESIAN_POINT('Origin',(95.,11.9,0.));
#57935=CARTESIAN_POINT('',(95.,-11.9,-1.45732969098535E-15));
#57936=CARTESIAN_POINT('Origin',(95.,0.,0.));
#57937=CARTESIAN_POINT('Origin',(95.5,0.,0.));
#57938=CARTESIAN_POINT('',(96.,-11.9,-1.45732969098535E-15));
#57939=CARTESIAN_POINT('Origin',(96.,0.,0.));
#57940=CARTESIAN_POINT('',(95.5,-11.9,-1.45732969098535E-15));
#57941=CARTESIAN_POINT('Origin',(96.25,0.,0.));
#57942=CARTESIAN_POINT('Ctrl Pts',(96.4460250000001,1.68935314532052,-12.5));
#57943=CARTESIAN_POINT('Ctrl Pts',(96.3046148851559,1.94289029309402E-15,
-12.5));
#57944=CARTESIAN_POINT('Ctrl Pts',(96.4460250000001,-1.68935314532052,-12.5));
#57945=CARTESIAN_POINT('',(96.25,-12.3,-1.50631556295124E-15));
#57946=CARTESIAN_POINT('Origin',(117.65,0.,0.));
#57947=CARTESIAN_POINT('',(117.65,-12.35,-1.51243879694698E-15));
#57948=CARTESIAN_POINT('Origin',(118.5,-2.7,-12.5));
#57949=CARTESIAN_POINT('Origin',(106.9,0.,0.));
#57950=CARTESIAN_POINT('',(0.,0.,0.));
#57951=CARTESIAN_POINT('Origin',(9.31,0.,0.));
#57952=CARTESIAN_POINT('',(9.12,24.5,-3.00038465791102E-15));
#57953=CARTESIAN_POINT('',(9.12,-24.5,-3.00038465791102E-15));
#57954=CARTESIAN_POINT('Origin',(9.12,0.,0.));
#57955=CARTESIAN_POINT('Origin',(9.12,0.,0.));
#57956=CARTESIAN_POINT('',(9.5,24.88,3.04692123627861E-15));
#57957=CARTESIAN_POINT('',(9.31,24.69,-3.02365294709482E-15));
#57958=CARTESIAN_POINT('Origin',(9.5,0.,0.));
#57959=CARTESIAN_POINT('Origin',(9.5,24.5,0.));
#57960=CARTESIAN_POINT('',(9.5,-32.185,-3.94152572305576E-15));
#57961=CARTESIAN_POINT('Origin',(9.5,0.,0.));
#57962=CARTESIAN_POINT('Origin',(8.95,0.,0.));
#57963=CARTESIAN_POINT('',(8.4,-24.5,-3.00038465791102E-15));
#57964=CARTESIAN_POINT('',(8.95,-24.5,-3.00038465791102E-15));
#57965=CARTESIAN_POINT('Origin',(8.4,0.,0.));
#57966=CARTESIAN_POINT('Origin',(0.19,0.,0.));
#57967=CARTESIAN_POINT('',(0.,29.78,-3.64699816786082E-15));
#57968=CARTESIAN_POINT('Origin',(0.,0.,0.));
#57969=CARTESIAN_POINT('',(0.38,29.4,3.60046158949322E-15));
#57970=CARTESIAN_POINT('',(0.19,29.59,-3.62372987867702E-15));
#57971=CARTESIAN_POINT('',(0.38,-29.4,-3.60046158949322E-15));
#57972=CARTESIAN_POINT('Origin',(0.38,0.,0.));
#57973=CARTESIAN_POINT('Origin',(0.38,0.,0.));
#57974=CARTESIAN_POINT('Origin',(0.,32.185,0.));
#57975=CARTESIAN_POINT('',(-1.14491749414469E-15,-32.185,-3.94152572305576E-15));
#57976=CARTESIAN_POINT('Origin',(0.,0.,0.));
#57977=CARTESIAN_POINT('Origin',(0.8,0.,0.));
#57978=CARTESIAN_POINT('',(1.6,-29.4,-3.60046158949322E-15));
#57979=CARTESIAN_POINT('Origin',(1.6,0.,0.));
#57980=CARTESIAN_POINT('',(0.8,-29.4,-3.60046158949322E-15));
#57981=CARTESIAN_POINT('Origin',(1.6,0.,0.));
#57982=CARTESIAN_POINT('',(1.6,-3.20857461376607E-15,26.2));
#57983=CARTESIAN_POINT('Origin',(1.6,0.,0.));
#57984=CARTESIAN_POINT('',(1.6,3.01263112590249E-15,24.6));
#57985=CARTESIAN_POINT('Origin',(1.6,-3.11060286983428E-15,25.4));
#57986=CARTESIAN_POINT('Origin',(1.6,0.,0.));
#57987=CARTESIAN_POINT('Origin',(1.6,29.4,0.));
#57988=CARTESIAN_POINT('',(1.6,-23.7,-2.90241291397923E-15));
#57989=CARTESIAN_POINT('Origin',(1.6,0.,0.));
#57990=CARTESIAN_POINT('Origin',(0.2,0.,0.));
#57991=CARTESIAN_POINT('',(0.4,-32.585,-3.99051159502165E-15));
#57992=CARTESIAN_POINT('Origin',(0.4,0.,0.));
#57993=CARTESIAN_POINT('',(0.2,-32.385,-3.9660186590387E-15));
#57994=CARTESIAN_POINT('Origin',(4.75,0.,0.));
#57995=CARTESIAN_POINT('',(9.1,-32.585,-3.99051159502165E-15));
#57996=CARTESIAN_POINT('Origin',(9.1,0.,0.));
#57997=CARTESIAN_POINT('',(4.75,-32.585,-3.99051159502165E-15));
#57998=CARTESIAN_POINT('Origin',(9.3,0.,0.));
#57999=CARTESIAN_POINT('',(9.3,-32.385,-3.9660186590387E-15));
#58000=CARTESIAN_POINT('Origin',(7.5,0.,0.));
#58001=CARTESIAN_POINT('',(6.6,-23.4,-2.86567351000481E-15));
#58002=CARTESIAN_POINT('',(7.5,-23.95,-2.93302908395791E-15));
#58003=CARTESIAN_POINT('Origin',(6.6,0.,0.));
#58004=CARTESIAN_POINT('Origin',(5.65,0.,0.));
#58005=CARTESIAN_POINT('',(4.7,-21.8413,-2.67478781342171E-15));
#58006=CARTESIAN_POINT('',(5.65,-22.62065,-2.77023066171326E-15));
#58007=CARTESIAN_POINT('Origin',(4.7,0.,0.));
#58008=CARTESIAN_POINT('Origin',(4.05,0.,0.));
#58009=CARTESIAN_POINT('',(3.4,-21.8413,-2.67478781342171E-15));
#58010=CARTESIAN_POINT('',(4.05,-21.8413,-2.67478781342171E-15));
#58011=CARTESIAN_POINT('Origin',(3.4,0.,0.));
#58012=CARTESIAN_POINT('Origin',(2.5,0.,0.));
#58013=CARTESIAN_POINT('',(2.5,-22.77065,-2.78860036370047E-15));
#58014=CARTESIAN_POINT('Origin',(1.6,29.4,0.));
#58015=CARTESIAN_POINT('',(0.,0.,0.));
#58016=CARTESIAN_POINT('Origin',(0.4,0.,0.));
#58017=CARTESIAN_POINT('',(0.8,-29.5655,-3.62072949401911E-15));
#58018=CARTESIAN_POINT('Origin',(0.8,0.,0.));
#58019=CARTESIAN_POINT('',(-4.85722573273506E-16,-28.7655,-3.52275775008732E-15));
#58020=CARTESIAN_POINT('',(0.4,-29.1655,-3.57174362205321E-15));
#58021=CARTESIAN_POINT('Origin',(0.,0.,0.));
#58022=CARTESIAN_POINT('Origin',(6.069,0.,0.));
#58023=CARTESIAN_POINT('',(11.338,-29.5655,-3.62072949401911E-15));
#58024=CARTESIAN_POINT('Origin',(11.338,0.,0.));
#58025=CARTESIAN_POINT('',(6.069,-29.5655,-3.62072949401911E-15));
#58026=CARTESIAN_POINT('Origin',(11.638,0.,0.));
#58027=CARTESIAN_POINT('',(11.938,-28.9655,-3.54725068607027E-15));
#58028=CARTESIAN_POINT('Origin',(11.938,0.,0.));
#58029=CARTESIAN_POINT('',(11.638,-29.2655,-3.58399009004469E-15));
#58030=CARTESIAN_POINT('Origin',(11.938,28.508778116497,0.));
#58031=CARTESIAN_POINT('',(11.938,-28.508778116497,-3.49131838679701E-15));
#58032=CARTESIAN_POINT('Origin',(11.938,0.,0.));
#58033=CARTESIAN_POINT('Origin',(11.788,0.,0.));
#58034=CARTESIAN_POINT('',(11.638,-28.208778116497,-3.45457898282259E-15));
#58035=CARTESIAN_POINT('',(11.788,-28.358778116497,-3.4729486848098E-15));
#58036=CARTESIAN_POINT('Origin',(11.638,0.,0.));
#58037=CARTESIAN_POINT('Origin',(6.069,0.,0.));
#58038=CARTESIAN_POINT('',(0.5,-26.4446922201623,-3.23854076818586E-15));
#58039=CARTESIAN_POINT('',(6.069,-27.3267351683296,-3.34655987550423E-15));
#58040=CARTESIAN_POINT('Origin',(0.5,0.,0.));
#58041=CARTESIAN_POINT('Origin',(0.25,0.,0.));
#58042=CARTESIAN_POINT('',(-4.85722573273506E-16,-26.8655,-3.29007485824932E-15));
#58043=CARTESIAN_POINT('',(0.25,-26.6550961100811,-3.26430781321759E-15));
#58044=CARTESIAN_POINT('Origin',(0.,0.,0.));
#58045=CARTESIAN_POINT('Origin',(0.,28.7655,0.));
#58046=CARTESIAN_POINT('',(0.,0.,0.));
#58047=CARTESIAN_POINT('Origin',(12.3795635938087,0.,0.));
#58048=CARTESIAN_POINT('',(12.6295635938087,25.8846416389917,-3.16995435302675E-15));
#58049=CARTESIAN_POINT('',(12.6295635938087,-25.8846416389917,-3.16995435302675E-15));
#58050=CARTESIAN_POINT('Origin',(12.6295635938087,0.,0.));
#58051=CARTESIAN_POINT('Origin',(12.6295635938087,0.,0.));
#58052=CARTESIAN_POINT('',(12.1295635938087,25.3846416389917,3.10872201306938E-15));
#58053=CARTESIAN_POINT('',(12.3795635938087,25.6346416389917,3.13933818304807E-15));
#58054=CARTESIAN_POINT('Origin',(12.1295635938087,0.,0.));
#58055=CARTESIAN_POINT('Origin',(12.1295635938087,25.8846416389917,0.));
#58056=CARTESIAN_POINT('',(12.1295635938087,-22.4888907487754,-2.75409480718623E-15));
#58057=CARTESIAN_POINT('Origin',(12.1295635938087,0.,0.));
#58058=CARTESIAN_POINT('Origin',(13.7522817969044,0.,0.));
#58059=CARTESIAN_POINT('',(15.375,-25.8846416389917,-3.16995435302675E-15));
#58060=CARTESIAN_POINT('Origin',(15.375,0.,0.));
#58061=CARTESIAN_POINT('',(13.7522817969044,-25.8846416389917,-3.16995435302675E-15));
#58062=CARTESIAN_POINT('Origin',(0.967576169359906,0.,0.));
#58063=CARTESIAN_POINT('',(1.21757616935991,22.2743990607509,-2.72782715126794E-15));
#58064=CARTESIAN_POINT('Origin',(1.21757616935991,0.,0.));
#58065=CARTESIAN_POINT('',(0.717576169359905,22.7743990607509,2.7890594912253E-15));
#58066=CARTESIAN_POINT('',(0.967576169359906,22.5243990607509,2.75844332124662E-15));
#58067=CARTESIAN_POINT('',(0.717576169359905,-22.7743990607509,-2.7890594912253E-15));
#58068=CARTESIAN_POINT('Origin',(0.717576169359905,0.,0.));
#58069=CARTESIAN_POINT('Origin',(0.717576169359905,0.,0.));
#58070=CARTESIAN_POINT('Origin',(0.364288084679953,0.,0.));
#58071=CARTESIAN_POINT('',(-0.488999999999999,-22.7743990607509,-2.7890594912253E-15));
#58072=CARTESIAN_POINT('',(0.364288084679953,-22.7743990607509,-2.7890594912253E-15));
#58073=CARTESIAN_POINT('Origin',(-0.488999999999999,0.,0.));
#58074=CARTESIAN_POINT('Origin',(1.21757616935991,21.5342155525986,0.));
#58075=CARTESIAN_POINT('',(1.2175761693599,-21.5342155525986,-2.63718081486391E-15));
#58076=CARTESIAN_POINT('Origin',(1.21757616935991,0.,0.));
#58077=CARTESIAN_POINT('Origin',(1.6653400148523,23.0866647604201,-6.77885640724594));
#58078=CARTESIAN_POINT('',(1.95776807072638,20.8526247727479,-5.62882899907203));
#58079=CARTESIAN_POINT('',(1.95776807072638,20.5855189702533,-6.53850782206135));
#58080=CARTESIAN_POINT('Ctrl Pts',(1.95776807072638,20.8526247727479,-5.62882899907201));
#58081=CARTESIAN_POINT('Ctrl Pts',(1.95134808310818,20.8520805812057,-5.62868975053389));
#58082=CARTESIAN_POINT('Ctrl Pts',(1.94501708164843,20.8512847270698,-5.62951292444653));
#58083=CARTESIAN_POINT('Ctrl Pts',(1.9295422670367,20.8487299346928,-5.63377986718356));
#58084=CARTESIAN_POINT('Ctrl Pts',(1.92098940734527,20.8467620801163,-5.63819408082448));
#58085=CARTESIAN_POINT('Ctrl Pts',(1.90083817144694,20.8410870108713,-5.65240862845873));
#58086=CARTESIAN_POINT('Ctrl Pts',(1.89018614013566,20.8369650214857,-5.6640399065301));
#58087=CARTESIAN_POINT('Ctrl Pts',(1.86077829278501,20.8234001483396,-5.70403903582823));
#58088=CARTESIAN_POINT('Ctrl Pts',(1.84665745875297,20.8126796100669,-5.73837519874369));
#58089=CARTESIAN_POINT('Ctrl Pts',(1.82247517384126,20.7910284502552,-5.80859546078155));
#58090=CARTESIAN_POINT('Ctrl Pts',(1.81230887642825,20.776390275316,-5.85747914655454));
#58091=CARTESIAN_POINT('Ctrl Pts',(1.79934881945703,20.7493484902442,-5.94843125987379));
#58092=CARTESIAN_POINT('Ctrl Pts',(1.79572382774354,20.7358065149718,-5.99432875769191));
#58093=CARTESIAN_POINT('Ctrl Pts',(1.79301769946662,20.7096735628667,-6.08315330650854));
#58094=CARTESIAN_POINT('Ctrl Pts',(1.79378222861462,20.696526800513,-6.12796795345379));
#58095=CARTESIAN_POINT('Ctrl Pts',(1.79982187672896,20.6703299712419,-6.2176096395351));
#58096=CARTESIAN_POINT('Ctrl Pts',(1.80545072973348,20.6566260406507,-6.26467818891722));
#58097=CARTESIAN_POINT('Ctrl Pts',(1.82510992022638,20.6280881697227,-6.3639304020438));
#58098=CARTESIAN_POINT('Ctrl Pts',(1.83960979647508,20.6150406765473,-6.4102079966474));
#58099=CARTESIAN_POINT('Ctrl Pts',(1.86695154341759,20.5997934931305,-6.4669505500946));
#58100=CARTESIAN_POINT('Ctrl Pts',(1.88252298601333,20.5925565805752,-6.49448704978994));
#58101=CARTESIAN_POINT('Ctrl Pts',(1.91281431352082,20.5866187437557,-6.52203861053669));
#58102=CARTESIAN_POINT('Ctrl Pts',(1.92253441500054,20.5853643741097,-6.52880678000705));
#58103=CARTESIAN_POINT('Ctrl Pts',(1.93813933311725,20.5847740821371,-6.53517979671551));
#58104=CARTESIAN_POINT('Ctrl Pts',(1.9431128878361,20.584762433612,-6.53665410256436));
#58105=CARTESIAN_POINT('Ctrl Pts',(1.95140011040206,20.5850644550901,-6.53809843282379));
#58106=CARTESIAN_POINT('Ctrl Pts',(1.95458052096174,20.5852542906539,-6.53841990666983));
#58107=CARTESIAN_POINT('Ctrl Pts',(1.95776807072638,20.5855189702533,-6.53850782206139));
#58108=CARTESIAN_POINT('',(1.65494820650842,23.7981126208907,-4.35135855429466));
#58109=CARTESIAN_POINT('Origin',(1.65494820650842,23.0854404918828,-6.7784969295689));
#58110=CARTESIAN_POINT('',(1.36757616935991,23.6797887759252,-4.62909020638214));
#58111=CARTESIAN_POINT('Origin',(1.6653400148523,23.714868609534,-4.63939057489758));
#58112=CARTESIAN_POINT('Origin',(1.36757616935991,23.0515849268112,-6.7685560387305));
#58113=CARTESIAN_POINT('Origin',(1.65494820650842,23.0854404918828,-6.7784969295689));
#58114=CARTESIAN_POINT('Origin',(6.4980472271939,23.6560104598922,-6.94603138825146));
#58115=CARTESIAN_POINT('',(11.664677238709,21.6751526289,-5.84039987251776));
#58116=CARTESIAN_POINT('Ctrl Pts',(11.664677238709,21.6751526289,-5.84039987251776));
#58117=CARTESIAN_POINT('Ctrl Pts',(8.45037669575293,21.402871216531,-5.77002260034825));
#58118=CARTESIAN_POINT('Ctrl Pts',(5.17722936343352,21.1255230570061,-5.69865861638706));
#58119=CARTESIAN_POINT('Ctrl Pts',(1.95776807072638,20.8526247727479,-5.62882899907202));
#58120=CARTESIAN_POINT('',(11.3203626311916,25.0326095573615,-4.35942481973593));
#58121=CARTESIAN_POINT('Origin',(11.3203626311916,24.2241318908269,-7.11284689157994));
#58122=CARTESIAN_POINT('',(11.664677238709,21.3918572850628,-6.80521520986101));
#58123=CARTESIAN_POINT('Origin',(11.3203626311916,24.2241318908269,-7.11284689157994));
#58124=CARTESIAN_POINT('Ctrl Pts',(1.95776807072638,20.5855189702533,-6.53850782206136));
#58125=CARTESIAN_POINT('Ctrl Pts',(5.17722935754855,20.8528483568881,-6.62730336112007));
#58126=CARTESIAN_POINT('Ctrl Pts',(8.45037668926195,21.1247507584877,-6.71721389316579));
#58127=CARTESIAN_POINT('Ctrl Pts',(11.664677238709,21.3918572850628,-6.80521520986103));
#58128=CARTESIAN_POINT('Origin',(11.3307544395355,24.2253561593642,-7.11320636925698));
#58129=CARTESIAN_POINT('',(11.6285182850279,24.9844453796138,-4.65775720885429));
#58130=CARTESIAN_POINT('Origin',(11.6285182850279,24.2604359929731,-7.12350673777241));
#58131=CARTESIAN_POINT('Origin',(11.3307544395355,24.9493655460049,-4.64745684033885));
#58132=CARTESIAN_POINT('Ctrl Pts',(11.664677238709,21.3918572850628,-6.80521520986105));
#58133=CARTESIAN_POINT('Ctrl Pts',(11.66817568376,21.392148003834,-6.80531099050326));
#58134=CARTESIAN_POINT('Ctrl Pts',(11.6716557442405,21.3925320801382,-6.80510802126784));
#58135=CARTESIAN_POINT('Ctrl Pts',(11.6751111337893,21.3930057822509,-6.80461609443976));
#58136=CARTESIAN_POINT('Ctrl Pts',(11.6834492137324,21.394148856289,-6.80342904297689));
#58137=CARTESIAN_POINT('Ctrl Pts',(11.691252831794,21.3957587099621,-6.80061996099569));
#58138=CARTESIAN_POINT('Ctrl Pts',(11.709123952862,21.4004306123475,-6.79107647501344));
#58139=CARTESIAN_POINT('Ctrl Pts',(11.7184891157759,21.403813335391,-6.78312340780538));
#58140=CARTESIAN_POINT('Ctrl Pts',(11.7423632180108,21.4140531027239,-6.75768907273798));
#58141=CARTESIAN_POINT('Ctrl Pts',(11.7550185107736,21.4219230191941,-6.73640225084232));
#58142=CARTESIAN_POINT('Ctrl Pts',(11.7829456066502,21.4426696595899,-6.67837363135184));
#58143=CARTESIAN_POINT('Ctrl Pts',(11.7977324484732,21.4588425587731,-6.63074355011391));
#58144=CARTESIAN_POINT('Ctrl Pts',(11.8194386441992,21.4943291980106,-6.521319716713));
#58145=CARTESIAN_POINT('Ctrl Pts',(11.825673894872,21.5120261889324,-6.46460165559978));
#58146=CARTESIAN_POINT('Ctrl Pts',(11.8317749863308,21.5456655992248,-6.3534917234499));
#58147=CARTESIAN_POINT('Ctrl Pts',(11.8316012176116,21.5626634804396,-6.29550105310408));
#58148=CARTESIAN_POINT('Ctrl Pts',(11.824941361477,21.5942940881578,-6.18401117291967));
#58149=CARTESIAN_POINT('Ctrl Pts',(11.8183083548574,21.6099774638489,-6.126836323049));
#58150=CARTESIAN_POINT('Ctrl Pts',(11.7958216244891,21.6390644648081,-6.01598903175142));
#58151=CARTESIAN_POINT('Ctrl Pts',(11.7805655796945,21.6509055854707,-5.96804659261267));
#58152=CARTESIAN_POINT('Ctrl Pts',(11.7536264417729,21.6637010911389,-5.91239047179336));
#58153=CARTESIAN_POINT('Ctrl Pts',(11.7402881749122,21.6689390523323,-5.88871674863419));
#58154=CARTESIAN_POINT('Ctrl Pts',(11.7136982696186,21.6740487842635,-5.86095365010973));
#58155=CARTESIAN_POINT('Ctrl Pts',(11.7035133274599,21.6753527807432,-5.85270707163253));
#58156=CARTESIAN_POINT('Ctrl Pts',(11.6842762528669,21.6760998603139,-5.84347561415645));
#58157=CARTESIAN_POINT('Ctrl Pts',(11.6760378533014,21.6759905549143,-5.84111037910662));
#58158=CARTESIAN_POINT('Ctrl Pts',(11.6665534479108,21.6753057278234,-5.8404626022536));
#58159=CARTESIAN_POINT('Ctrl Pts',(11.6656136423373,21.6752319510726,-5.84042037512234));
#58160=CARTESIAN_POINT('Ctrl Pts',(11.664677238709,21.6751526289,-5.84039987251776));
#58161=CARTESIAN_POINT('Origin',(11.6285182850279,24.2604359929731,-7.12350673777241));
#58162=CARTESIAN_POINT('Origin',(1.06052702375292,25.4510030262676,-7.47308876036672));
#58163=CARTESIAN_POINT('Origin',(1.6653400148523,20.2416680737422,-13.0085301837882));
#58164=CARTESIAN_POINT('',(1.95776807072638,18.4221225649395,-11.2756851683684));
#58165=CARTESIAN_POINT('',(1.95776807072638,17.9095502835289,-12.0732632065885));
#58166=CARTESIAN_POINT('Ctrl Pts',(1.95776807072638,18.4221225649395,-11.2756851683684));
#58167=CARTESIAN_POINT('Ctrl Pts',(1.95134736181873,18.4216395935691,-11.2753982116637));
#58168=CARTESIAN_POINT('Ctrl Pts',(1.9450156712346,18.4206438937207,-11.2759639830928));
#58169=CARTESIAN_POINT('Ctrl Pts',(1.92948836979285,18.4169777842863,-11.2793502116275));
#58170=CARTESIAN_POINT('Ctrl Pts',(1.92089186233944,18.4138230903948,-11.2830613241244));
#58171=CARTESIAN_POINT('Ctrl Pts',(1.90046800930148,18.404219117633,-11.2953067736055));
#58172=CARTESIAN_POINT('Ctrl Pts',(1.88964186308571,18.3968030080759,-11.3055760598063));
#58173=CARTESIAN_POINT('Ctrl Pts',(1.85810283833446,18.3704851710231,-11.3430782725488));
#58174=CARTESIAN_POINT('Ctrl Pts',(1.84335629303651,18.3481042542479,-11.3767845480163));
#58175=CARTESIAN_POINT('Ctrl Pts',(1.8185401058917,18.3040341652241,-11.4435429822488));
#58176=CARTESIAN_POINT('Ctrl Pts',(1.80836917826471,18.2726985595787,-11.4918522175943));
#58177=CARTESIAN_POINT('Ctrl Pts',(1.79896764765288,18.2274018269566,-11.5619364610544));
#58178=CARTESIAN_POINT('Ctrl Pts',(1.79670145400055,18.2114630036209,-11.5866568740709));
#58179=CARTESIAN_POINT('Ctrl Pts',(1.79434535609111,18.1842435918479,-11.6289286489362));
#58180=CARTESIAN_POINT('Ctrl Pts',(1.79381557303811,18.1727761179958,-11.6467551189361));
#58181=CARTESIAN_POINT('Ctrl Pts',(1.79365032105972,18.1502654058704,-11.6817769814638));
#58182=CARTESIAN_POINT('Ctrl Pts',(1.79398945985935,18.1391347052039,-11.6991076651005));
#58183=CARTESIAN_POINT('Ctrl Pts',(1.79575501944582,18.1136547229068,-11.7388159539015));
#58184=CARTESIAN_POINT('Ctrl Pts',(1.79749007695653,18.0991705776075,-11.7614139961328));
#58185=CARTESIAN_POINT('Ctrl Pts',(1.80455267776998,18.0593401604995,-11.8236744660539));
#58186=CARTESIAN_POINT('Ctrl Pts',(1.8118645191381,18.0330203540234,-11.8649367864138));
#58187=CARTESIAN_POINT('Ctrl Pts',(1.83578355229011,17.9799323185428,-11.9490437490375));
#58188=CARTESIAN_POINT('Ctrl Pts',(1.85214505346392,17.9570952779814,-11.9858397344734));
#58189=CARTESIAN_POINT('Ctrl Pts',(1.88061329933208,17.9321806919607,-12.0275219208858));
#58190=CARTESIAN_POINT('Ctrl Pts',(1.89448595076435,17.9221533057526,-12.0446318207675));
#58191=CARTESIAN_POINT('Ctrl Pts',(1.92022261571983,17.9130069990605,-12.0622553637806));
#58192=CARTESIAN_POINT('Ctrl Pts',(1.92864558703621,17.9109234054499,-12.0666669158282));
#58193=CARTESIAN_POINT('Ctrl Pts',(1.9419227872126,17.9094652452642,-12.0709092294435));
#58194=CARTESIAN_POINT('Ctrl Pts',(1.94616291414738,17.9092382087298,-12.0719097149397));
#58195=CARTESIAN_POINT('Ctrl Pts',(1.95291207284946,17.9092807395708,-12.0729030082249));
#58196=CARTESIAN_POINT('Ctrl Pts',(1.95533909577677,17.9093756366031,-12.0731421041236));
#58197=CARTESIAN_POINT('Ctrl Pts',(1.95776807072638,17.9095502835289,-12.0732632065885));
#58198=CARTESIAN_POINT('',(1.65494820650842,21.6082024737958,-10.8798010752069));
#58199=CARTESIAN_POINT('Origin',(1.65494820650842,20.2405946732479,-13.0078403511776));
#58200=CARTESIAN_POINT('',(1.36757616935991,21.416425527482,-11.1129469645577));
#58201=CARTESIAN_POINT('Origin',(1.6653400148523,21.447182432187,-11.1327132269901));
#58202=CARTESIAN_POINT('Origin',(1.36757616935991,20.2109111690372,-12.9887639213558));
#58203=CARTESIAN_POINT('Origin',(1.65494820650842,20.2405946732479,-13.0078403511776));
#58204=CARTESIAN_POINT('Origin',(6.4980472271939,20.7408526371047,-13.3293366230661));
#58205=CARTESIAN_POINT('',(11.664677238709,19.1517258603906,-11.7104188108481));
#58206=CARTESIAN_POINT('Ctrl Pts',(11.664677238709,19.1517258603906,-11.7104188108481));
#58207=CARTESIAN_POINT('Ctrl Pts',(8.44760841234031,18.9100934028027,-11.566057551542));
#58208=CARTESIAN_POINT('Ctrl Pts',(5.17558411912346,18.6641695178434,-11.4194969970449));
#58209=CARTESIAN_POINT('Ctrl Pts',(1.95776807072638,18.4221225649395,-11.2756851683684));
#58210=CARTESIAN_POINT('',(11.3203626311916,22.7904210807013,-11.2353385785459));
#58211=CARTESIAN_POINT('Origin',(11.3203626311916,21.2389637999728,-13.6494532297333));
#58212=CARTESIAN_POINT('',(11.664677238709,18.6080860766515,-12.5563388263038));
#58213=CARTESIAN_POINT('Origin',(11.3203626311916,21.2389637999728,-13.6494532297333));
#58214=CARTESIAN_POINT('Ctrl Pts',(1.95776807072638,17.9095502835289,-12.0732632065885));
#58215=CARTESIAN_POINT('Ctrl Pts',(5.17558411308691,18.1409160618572,-12.2336952663475));
#58216=CARTESIAN_POINT('Ctrl Pts',(8.44760840593807,18.3763927053254,-12.3965120458592));
#58217=CARTESIAN_POINT('Ctrl Pts',(11.664677238709,18.6080860766515,-12.5563388263038));
#58218=CARTESIAN_POINT('Origin',(11.3307544395355,21.2400372004671,-13.6501430623439));
#58219=CARTESIAN_POINT('',(11.6285182850279,22.6601579437975,-11.5080169927616));
#58220=CARTESIAN_POINT('Origin',(11.6285182850279,21.2707941051722,-13.6699093247763));
#58221=CARTESIAN_POINT('Origin',(11.3307544395355,22.6294010390925,-11.4882507303292));
#58222=CARTESIAN_POINT('Ctrl Pts',(11.664677238709,18.6080860766515,-12.5563388263038));
#58223=CARTESIAN_POINT('Ctrl Pts',(11.6681719057554,18.6083377626526,-12.5565124444052));
#58224=CARTESIAN_POINT('Ctrl Pts',(11.6716519636862,18.6087630873824,-12.5564264617449));
#58225=CARTESIAN_POINT('Ctrl Pts',(11.6751111337893,18.6093568419532,-12.5560875483161));
#58226=CARTESIAN_POINT('Ctrl Pts',(11.6833639439589,18.6107734082434,-12.5552789762861));
#58227=CARTESIAN_POINT('Ctrl Pts',(11.6912209922801,18.6131029323727,-12.5530553109812));
#58228=CARTESIAN_POINT('Ctrl Pts',(11.7092716451021,18.6203670705107,-12.5451050615272));
#58229=CARTESIAN_POINT('Ctrl Pts',(11.7188321121789,18.6259692752841,-12.5382858333101));
#58230=CARTESIAN_POINT('Ctrl Pts',(11.7448362096954,18.6446600490309,-12.5145712192165));
#58231=CARTESIAN_POINT('Ctrl Pts',(11.7582763496129,18.6601414182571,-12.4935901023802));
#58232=CARTESIAN_POINT('Ctrl Pts',(11.7901173768954,18.7031288181136,-12.4342691481539));
#58233=CARTESIAN_POINT('Ctrl Pts',(11.807496900688,18.7427730168718,-12.3773456251789));
#58234=CARTESIAN_POINT('Ctrl Pts',(11.8229354401012,18.8072490251109,-12.2814049176089));
#58235=CARTESIAN_POINT('Ctrl Pts',(11.8261991991769,18.8268628597468,-12.2518426658348));
#58236=CARTESIAN_POINT('Ctrl Pts',(11.8295237141305,18.8585151047524,-12.2035704025212));
#58237=CARTESIAN_POINT('Ctrl Pts',(11.8303434615844,18.8708529717768,-12.1846162306134));
#58238=CARTESIAN_POINT('Ctrl Pts',(11.8309946485842,18.8938873215581,-12.1489677324933));
#58239=CARTESIAN_POINT('Ctrl Pts',(11.8309459330901,18.9046640233566,-12.1321843072664));
#58240=CARTESIAN_POINT('Ctrl Pts',(11.8300359252892,18.9280174953952,-12.0955751475506));
#58241=CARTESIAN_POINT('Ctrl Pts',(11.8290394062419,18.9406788268584,-12.0755774687242));
#58242=CARTESIAN_POINT('Ctrl Pts',(11.8249644421306,18.9736962566426,-12.023004023433));
#58243=CARTESIAN_POINT('Ctrl Pts',(11.8209395722477,18.9943695927783,-11.9896581821858));
#58244=CARTESIAN_POINT('Ctrl Pts',(11.8028867656277,19.0556901070888,-11.8891741309915));
#58245=CARTESIAN_POINT('Ctrl Pts',(11.7841990134601,19.0898144719035,-11.831040921109));
#58246=CARTESIAN_POINT('Ctrl Pts',(11.7507704380576,19.1229326946467,-11.7717678295022));
#58247=CARTESIAN_POINT('Ctrl Pts',(11.7371459986439,19.1343448984335,-11.7509308503553));
#58248=CARTESIAN_POINT('Ctrl Pts',(11.7101248465183,19.1461490561111,-11.7271518112195));
#58249=CARTESIAN_POINT('Ctrl Pts',(11.700195678653,19.1493048584522,-11.7203319567739));
#58250=CARTESIAN_POINT('Ctrl Pts',(11.6812735959896,19.1520152885414,-11.7127291553658));
#58251=CARTESIAN_POINT('Ctrl Pts',(11.6731643433663,19.1523622516496,-11.7108014088155));
#58252=CARTESIAN_POINT('Ctrl Pts',(11.6646867061662,19.1517265711868,-11.7104192361762));
#58253=CARTESIAN_POINT('Ctrl Pts',(11.6646819724071,19.1517262159363,-11.7104190232658));
#58254=CARTESIAN_POINT('Ctrl Pts',(11.664677238709,19.1517258603906,-11.7104188108481));
#58255=CARTESIAN_POINT('Origin',(11.6285182850279,21.2707941051722,-13.6699093247763));
#58256=CARTESIAN_POINT('Origin',(1.06052702375292,22.314646171184,-14.3407523135387));
#58257=CARTESIAN_POINT('Origin',(1.6653400148523,15.756811821565,-18.1843302095478));
#58258=CARTESIAN_POINT('',(1.95776807072638,14.4991695475011,-16.0090523844052));
#58259=CARTESIAN_POINT('',(1.95776807072638,13.7826563450298,-16.6299146085788));
#58260=CARTESIAN_POINT('Ctrl Pts',(1.95776807072638,14.4991695475011,-16.0090523844052));
#58261=CARTESIAN_POINT('Ctrl Pts',(1.95134736175434,14.4987869849071,-16.0086409827002));
#58262=CARTESIAN_POINT('Ctrl Pts',(1.9450156711341,14.4976722216424,-16.0089033153653));
#58263=CARTESIAN_POINT('Ctrl Pts',(1.92948836979141,14.4932006046047,-16.0111195154529));
#58264=CARTESIAN_POINT('Ctrl Pts',(1.92089186233797,14.4891281567692,-16.013791521842));
#58265=CARTESIAN_POINT('Ctrl Pts',(1.90046800929961,14.4764632705929,-16.0228351927764));
#58266=CARTESIAN_POINT('Ctrl Pts',(1.88964186308364,14.4664543733224,-16.0305991412233));
#58267=CARTESIAN_POINT('Ctrl Pts',(1.85810283833147,14.430636999304,-16.0591676593232));
#58268=CARTESIAN_POINT('Ctrl Pts',(1.84335629303329,14.3996665117438,-16.0852031608956));
#58269=CARTESIAN_POINT('Ctrl Pts',(1.81854010589001,14.3385735466119,-16.1368414306103));
#58270=CARTESIAN_POINT('Ctrl Pts',(1.80836917826375,14.2948969687799,-16.1743655421849));
#58271=CARTESIAN_POINT('Ctrl Pts',(1.79896764765251,14.2316900589987,-16.2288493170464));
#58272=CARTESIAN_POINT('Ctrl Pts',(1.79670145400032,14.2094323248355,-16.2480778941888));
#58273=CARTESIAN_POINT('Ctrl Pts',(1.79434535609101,14.171406155279,-16.2809687706792));
#58274=CARTESIAN_POINT('Ctrl Pts',(1.79381557303806,14.1553808977203,-16.2948423826596));
#58275=CARTESIAN_POINT('Ctrl Pts',(1.79365032105974,14.1239152287297,-16.3221036131944));
#58276=CARTESIAN_POINT('Ctrl Pts',(1.79398945985941,14.1083527818359,-16.3355964016136));
#58277=CARTESIAN_POINT('Ctrl Pts',(1.79575501944599,14.0727178001221,-16.3665176851518));
#58278=CARTESIAN_POINT('Ctrl Pts',(1.7974900769568,14.0524537602606,-16.3841196926017));
#58279=CARTESIAN_POINT('Ctrl Pts',(1.80455267777069,13.9966959535269,-16.4326366507742));
#58280=CARTESIAN_POINT('Ctrl Pts',(1.81186451913932,13.9598173451288,-16.4648124108617));
#58281=CARTESIAN_POINT('Ctrl Pts',(1.83578355229297,13.8851840784728,-16.5305558225588));
#58282=CARTESIAN_POINT('Ctrl Pts',(1.85214505346792,13.852905471457,-16.5594273742142));
#58283=CARTESIAN_POINT('Ctrl Pts',(1.88061329933735,13.8172568722789,-16.592401889178));
#58284=CARTESIAN_POINT('Ctrl Pts',(1.89448595076901,13.8028152498295,-16.6059936767371));
#58285=CARTESIAN_POINT('Ctrl Pts',(1.92022261572312,13.7890743069924,-16.6203265300565));
#58286=CARTESIAN_POINT('Ctrl Pts',(1.92864558703888,13.7858322357257,-16.623972367093));
#58287=CARTESIAN_POINT('Ctrl Pts',(1.94192278721444,13.7832379434119,-16.6276320260008));
#58288=CARTESIAN_POINT('Ctrl Pts',(1.94616291414881,13.7827382341155,-16.6285280212212));
#58289=CARTESIAN_POINT('Ctrl Pts',(1.9529120727631,13.782499199105,-16.629493061459));
#58290=CARTESIAN_POINT('Ctrl Pts',(1.95533909571058,13.782522891035,-16.6297492078852));
#58291=CARTESIAN_POINT('Ctrl Pts',(1.95776807072638,13.7826563450298,-16.6299146085789));
#58292=CARTESIAN_POINT('',(1.65494820650842,17.6677242712023,-16.5268268176743));
#58293=CARTESIAN_POINT('Origin',(1.65494820650842,15.755976249638,-18.1833659081392));
#58294=CARTESIAN_POINT('',(1.36757616935991,17.418030851189,-16.6964988509053));
#58295=CARTESIAN_POINT('Origin',(1.6653400148523,17.4419730854894,-16.7241296622268));
#58296=CARTESIAN_POINT('Origin',(1.36757616935991,15.7328695872647,-18.1566993982262));
#58297=CARTESIAN_POINT('Origin',(1.65494820650842,15.755976249638,-18.1833659081392));
#58298=CARTESIAN_POINT('Origin',(6.4980472271939,16.1453942842592,-18.6327782772971));
#58299=CARTESIAN_POINT('',(11.664677238709,15.0767401623716,-16.6317292616657));
#58300=CARTESIAN_POINT('Ctrl Pts',(11.664677238709,15.0767401623716,-16.6317292616657));
#58301=CARTESIAN_POINT('Ctrl Pts',(8.44646649976651,14.8854989259897,-16.425066587821));
#58302=CARTESIAN_POINT('Ctrl Pts',(5.17487115867276,14.6908529438561,-16.2151856480993));
#58303=CARTESIAN_POINT('Ctrl Pts',(1.95776807072638,14.4991695475011,-16.0090523844052));
#58304=CARTESIAN_POINT('',(11.3203626311916,18.7018882279357,-17.2010320248535));
#58305=CARTESIAN_POINT('Origin',(11.3203626311916,16.5331411750263,-19.0802620436377));
#58306=CARTESIAN_POINT('',(11.664677238709,14.316798400859,-17.2902225464619));
#58307=CARTESIAN_POINT('Origin',(11.3203626311916,16.5331411750263,-19.0802620436377));
#58308=CARTESIAN_POINT('Ctrl Pts',(1.95776807072638,13.7826563450298,-16.6299146085789));
#58309=CARTESIAN_POINT('Ctrl Pts',(5.17487115257265,13.959412077432,-16.8489827660136));
#58310=CARTESIAN_POINT('Ctrl Pts',(8.44646649340719,14.1394557203275,-17.0715167046817));
#58311=CARTESIAN_POINT('Ctrl Pts',(11.664677238709,14.316798400859,-17.2902225464619));
#58312=CARTESIAN_POINT('Origin',(11.3307544395355,16.5339767469533,-19.0812263450464));
#58313=CARTESIAN_POINT('',(11.6285182850279,18.5000792765231,-17.4259656807277));
#58314=CARTESIAN_POINT('Origin',(11.6285182850279,16.5579189812536,-19.1088571563679));
#58315=CARTESIAN_POINT('Origin',(11.3307544395355,18.4761370422228,-17.3983348694061));
#58316=CARTESIAN_POINT('Ctrl Pts',(11.664677238709,14.316798400859,-17.2902225464619));
#58317=CARTESIAN_POINT('Ctrl Pts',(11.6681719057554,14.316990977937,-17.2904600399508));
#58318=CARTESIAN_POINT('Ctrl Pts',(11.6716519636862,14.3174232981415,-17.2904973680161));
#58319=CARTESIAN_POINT('Ctrl Pts',(11.6751111337893,14.3180884844271,-17.2903394629558));
#58320=CARTESIAN_POINT('Ctrl Pts',(11.6833639439589,14.3196754708946,-17.2899627366173));
#58321=CARTESIAN_POINT('Ctrl Pts',(11.6912209922801,14.3225371118404,-17.2884854481706));
#58322=CARTESIAN_POINT('Ctrl Pts',(11.7092716451021,14.3317468454494,-17.282903783892));
#58323=CARTESIAN_POINT('Ctrl Pts',(11.7188321121788,14.3390433201674,-17.2779391058069));
#58324=CARTESIAN_POINT('Ctrl Pts',(11.7448362096952,14.3636581651119,-17.2604508996893));
#58325=CARTESIAN_POINT('Ctrl Pts',(11.7582763496127,14.3844234937979,-17.2446812712418));
#58326=CARTESIAN_POINT('Ctrl Pts',(11.7901173768955,14.442382246023,-17.1998741825469));
#58327=CARTESIAN_POINT('Ctrl Pts',(11.807496900688,14.4964577858483,-17.1564255236989));
#58328=CARTESIAN_POINT('Ctrl Pts',(11.8229354401012,14.5853516835692,-17.0825360795582));
#58329=CARTESIAN_POINT('Ctrl Pts',(11.8261991991769,14.6124996688663,-17.0596971624782));
#58330=CARTESIAN_POINT('Ctrl Pts',(11.8295237141305,14.656469643716,-17.0222977329236));
#58331=CARTESIAN_POINT('Ctrl Pts',(11.8303434615844,14.6736477477497,-17.0075873169801));
#58332=CARTESIAN_POINT('Ctrl Pts',(11.8309946485842,14.7057923870397,-16.979872359773));
#58333=CARTESIAN_POINT('Ctrl Pts',(11.8309459330901,14.7208609939958,-16.9668049289466));
#58334=CARTESIAN_POINT('Ctrl Pts',(11.8300359252892,14.7535824784968,-16.938258130818));
#58335=CARTESIAN_POINT('Ctrl Pts',(11.8290394062419,14.771364934259,-16.9226376077816));
#58336=CARTESIAN_POINT('Ctrl Pts',(11.8249644421306,14.8178565773077,-16.8814958413394));
#58337=CARTESIAN_POINT('Ctrl Pts',(11.8209395722478,14.8470871071857,-16.8553250928114));
#58338=CARTESIAN_POINT('Ctrl Pts',(11.8028867656278,14.9342333384695,-16.7761873370138));
#58339=CARTESIAN_POINT('Ctrl Pts',(11.7841990134602,14.983353444596,-16.7300228751476));
#58340=CARTESIAN_POINT('Ctrl Pts',(11.7507704380578,15.0318293062667,-16.6824812417983));
#58341=CARTESIAN_POINT('Ctrl Pts',(11.7371459986441,15.0486496910258,-16.6657034960673));
#58342=CARTESIAN_POINT('Ctrl Pts',(11.7101248465183,15.0666750268719,-16.6462132906209));
#58343=CARTESIAN_POINT('Ctrl Pts',(11.700195678653,15.0716243720746,-16.6405587804617));
#58344=CARTESIAN_POINT('Ctrl Pts',(11.6812735959896,15.0763669673805,-16.6340275623301));
#58345=CARTESIAN_POINT('Ctrl Pts',(11.6731643433662,15.0772429850095,-16.6322756538638));
#58346=CARTESIAN_POINT('Ctrl Pts',(11.6646867061662,15.0767407245468,-16.6317298700195));
#58347=CARTESIAN_POINT('Ctrl Pts',(11.664681972407,15.0767404436703,-16.6317295656479));
#58348=CARTESIAN_POINT('Ctrl Pts',(11.664677238709,15.0767401623716,-16.6317292616657));
#58349=CARTESIAN_POINT('Origin',(11.6285182850279,16.5579189812536,-19.1088571563679));
#58350=CARTESIAN_POINT('Origin',(1.06052702375292,17.3704893936218,-20.0466134020057));
#58351=CARTESIAN_POINT('Origin',(1.6653400148523,9.99543238497271,-21.8869439481057));
#58352=CARTESIAN_POINT('',(1.95776807072638,9.40158004320574,-19.4454613857581));
#58353=CARTESIAN_POINT('',(1.95776807072638,8.5391735580698,-19.8393092308925));
#58354=CARTESIAN_POINT('Ctrl Pts',(1.95776807072638,9.40158004320574,-19.4454613857581));
#58355=CARTESIAN_POINT('Ctrl Pts',(1.95134736182033,9.40132888234158,-19.4449588683802));
#58356=CARTESIAN_POINT('Ctrl Pts',(1.9450156712371,9.4001853671993,-19.4448965096135));
#58357=CARTESIAN_POINT('Ctrl Pts',(1.9294883697929,9.39527050632201,-19.4457631379299));
#58358=CARTESIAN_POINT('Ctrl Pts',(1.9208918623395,9.39061023004678,-19.4471795681443));
#58359=CARTESIAN_POINT('Ctrl Pts',(1.90046800930151,9.37591046421419,-19.4522887960966));
#58360=CARTESIAN_POINT('Ctrl Pts',(1.88964186308573,9.36411964056307,-19.4569184178595));
#58361=CARTESIAN_POINT('Ctrl Pts',(1.85810283833451,9.32170444021247,-19.4742387898801));
#58362=CARTESIAN_POINT('Ctrl Pts',(1.84335629303657,9.28465342658525,-19.490494276055));
#58363=CARTESIAN_POINT('Ctrl Pts',(1.81854010589175,9.21148697404632,-19.5228289557441));
#58364=CARTESIAN_POINT('Ctrl Pts',(1.80836917826474,9.15900784060588,-19.5465279631953));
#58365=CARTESIAN_POINT('Ctrl Pts',(1.79896764765288,9.08301140158671,-19.5809973180491));
#58366=CARTESIAN_POINT('Ctrl Pts',(1.79670145400056,9.05623794584522,-19.5931762743548));
#58367=CARTESIAN_POINT('Ctrl Pts',(1.7943453560911,9.01048567261109,-19.6140216292677));
#58368=CARTESIAN_POINT('Ctrl Pts',(1.79381557303811,8.99120090240708,-19.6228184256956));
#58369=CARTESIAN_POINT('Ctrl Pts',(1.79365032105972,8.95332943791956,-19.6401104814682));
#58370=CARTESIAN_POINT('Ctrl Pts',(1.79398945985935,8.93459602169254,-19.6486722691968));
#58371=CARTESIAN_POINT('Ctrl Pts',(1.79575501944581,8.89169297485158,-19.6683014889754));
#58372=CARTESIAN_POINT('Ctrl Pts',(1.79749007695653,8.86729071242359,-19.6794814516828));
#58373=CARTESIAN_POINT('Ctrl Pts',(1.80455267776997,8.80012268196408,-19.7103243426947));
#58374=CARTESIAN_POINT('Ctrl Pts',(1.81186451913807,8.75567295717316,-19.7308068537818));
#58375=CARTESIAN_POINT('Ctrl Pts',(1.83578355228958,8.6655408027493,-19.7728605743246));
#58376=CARTESIAN_POINT('Ctrl Pts',(1.85214505346309,8.62643565005177,-19.7914686907894));
#58377=CARTESIAN_POINT('Ctrl Pts',(1.8806132993318,8.58294107520657,-19.8130641352126));
#58378=CARTESIAN_POINT('Ctrl Pts',(1.89448595076413,8.56525519087511,-19.822036684658));
#58379=CARTESIAN_POINT('Ctrl Pts',(1.92022261571973,8.54803282135688,-19.8319176857522));
#58380=CARTESIAN_POINT('Ctrl Pts',(1.92864558703613,8.54389492576569,-19.8345024437446));
#58381=CARTESIAN_POINT('Ctrl Pts',(1.94192278721276,8.54037467545705,-19.8372829641461));
#58382=CARTESIAN_POINT('Ctrl Pts',(1.94616291414744,8.5396427768739,-19.8380018808868));
#58383=CARTESIAN_POINT('Ctrl Pts',(1.9529120728908,8.53914154119746,-19.838860486286));
#58384=CARTESIAN_POINT('Ctrl Pts',(1.95533909580839,8.53909210866309,-19.8391129317619));
#58385=CARTESIAN_POINT('Ctrl Pts',(1.95776807072638,8.53917355806979,-19.8393092308925));
#58386=CARTESIAN_POINT('',(1.65494820650842,12.2959121221581,-20.8349473401973));
#58387=CARTESIAN_POINT('Origin',(1.65494820650842,9.9949023346812,-21.8857832998643));
#58388=CARTESIAN_POINT('',(1.36757616935991,12.0085309043509,-20.9273996982545));
#58389=CARTESIAN_POINT('Origin',(1.6653400148523,12.0237188108134,-20.9606565744588));
#58390=CARTESIAN_POINT('Origin',(1.36757616935991,9.98024447851015,-21.8536870719015));
#58391=CARTESIAN_POINT('Origin',(1.65494820650842,9.9949023346812,-21.8857832998643));
#58392=CARTESIAN_POINT('Origin',(6.4980472271939,10.24193210686,-22.4267030489007));
#58393=CARTESIAN_POINT('',(11.664677238709,9.78032664122358,-20.2056359204057));
#58394=CARTESIAN_POINT('Ctrl Pts',(11.664677238709,9.78032664122358,-20.2056359204057));
#58395=CARTESIAN_POINT('Ctrl Pts',(8.44908820479151,9.65515767378835,-19.9536710841398));
#58396=CARTESIAN_POINT('Ctrl Pts',(5.17648536371073,9.52748760709607,-19.697374593167));
#58397=CARTESIAN_POINT('Ctrl Pts',(1.95776807072638,9.40158004320575,-19.4454613857581));
#58398=CARTESIAN_POINT('',(11.3203626311916,13.0982396153547,-21.7732001549839));
#58399=CARTESIAN_POINT('Origin',(11.3203626311916,10.4879017784557,-22.9653015014543));
#58400=CARTESIAN_POINT('',(11.664677238709,8.86564886390742,-20.6233552648184));
#58401=CARTESIAN_POINT('Origin',(11.3203626311916,10.4879017784557,-22.9653015014543));
#58402=CARTESIAN_POINT('Ctrl Pts',(1.95776807072638,8.5391735580698,-19.8393092308925));
#58403=CARTESIAN_POINT('Ctrl Pts',(5.17648535775567,8.64710493744507,-20.0994318861236));
#58404=CARTESIAN_POINT('Ctrl Pts',(8.44908819833864,8.75719478781139,-20.3637569928305));
#58405=CARTESIAN_POINT('Ctrl Pts',(11.664677238709,8.86564886390743,-20.6233552648184));
#58406=CARTESIAN_POINT('Origin',(11.3307544395355,10.4884318287472,-22.9664621496957));
#58407=CARTESIAN_POINT('',(11.6285182850279,12.8412342104726,-21.9321662654496));
#58408=CARTESIAN_POINT('Origin',(11.6285182850279,10.5036197352098,-22.9997190259));
#58409=CARTESIAN_POINT('Origin',(11.3307544395355,12.8260463040101,-21.8989093892453));
#58410=CARTESIAN_POINT('Ctrl Pts',(11.664677238709,8.86564886390742,-20.6233552648184));
#58411=CARTESIAN_POINT('Ctrl Pts',(11.6681531449969,8.8657660978575,-20.6236358788069));
#58412=CARTESIAN_POINT('Ctrl Pts',(11.6716331726355,8.86616731353293,-20.623794813083));
#58413=CARTESIAN_POINT('Ctrl Pts',(11.6751111337893,8.86685375084357,-20.623830903915));
#58414=CARTESIAN_POINT('Ctrl Pts',(11.6835034416364,8.8685101216234,-20.623917990964));
#58415=CARTESIAN_POINT('Ctrl Pts',(11.6913221163004,8.87170945339749,-20.6232869878783));
#58416=CARTESIAN_POINT('Ctrl Pts',(11.7093237578239,8.88207391467146,-20.6205407109361));
#58417=CARTESIAN_POINT('Ctrl Pts',(11.7187565997267,8.89041824124016,-20.6178443174412));
#58418=CARTESIAN_POINT('Ctrl Pts',(11.7431727782355,8.91707792401492,-20.6086622526054));
#58419=CARTESIAN_POINT('Ctrl Pts',(11.7560898230284,8.93917319578265,-20.6003233906746));
#58420=CARTESIAN_POINT('Ctrl Pts',(11.7841758181733,8.9980591075342,-20.5773806426638));
#58421=CARTESIAN_POINT('Ctrl Pts',(11.7988195826631,9.04537291470594,-20.5580695606808));
#58422=CARTESIAN_POINT('Ctrl Pts',(11.8183861888449,9.14332972967495,-20.5165359590652));
#58423=CARTESIAN_POINT('Ctrl Pts',(11.8239771978735,9.18842241074054,-20.4969162334911));
#58424=CARTESIAN_POINT('Ctrl Pts',(11.8302306705076,9.27219438300242,-20.4597498600097));
#58425=CARTESIAN_POINT('Ctrl Pts',(11.8313291886565,9.31273094134296,-20.4414345067909));
#58426=CARTESIAN_POINT('Ctrl Pts',(11.8301000822046,9.39324349826456,-20.4044483831862));
#58427=CARTESIAN_POINT('Ctrl Pts',(11.8275983467483,9.43446674805166,-20.3851769035863));
#58428=CARTESIAN_POINT('Ctrl Pts',(11.8179490511515,9.51988766495169,-20.3445084778329));
#58429=CARTESIAN_POINT('Ctrl Pts',(11.8098404493788,9.56648167385506,-20.3218506008119));
#58430=CARTESIAN_POINT('Ctrl Pts',(11.7817370234729,9.66788637809238,-20.271128320578));
#58431=CARTESIAN_POINT('Ctrl Pts',(11.7608617911997,9.7115392210737,-20.2481472837836));
#58432=CARTESIAN_POINT('Ctrl Pts',(11.727864569176,9.75179858555556,-20.2255615388921));
#58433=CARTESIAN_POINT('Ctrl Pts',(11.7163738956147,9.76278438208106,-20.2191422746271));
#58434=CARTESIAN_POINT('Ctrl Pts',(11.6949981921876,9.77494241482742,-20.2111886963503));
#58435=CARTESIAN_POINT('Ctrl Pts',(11.6861739271887,9.77828873356615,-20.2087116448862));
#58436=CARTESIAN_POINT('Ctrl Pts',(11.6727399598045,9.7802682842181,-20.2064478679052));
#58437=CARTESIAN_POINT('Ctrl Pts',(11.6686987410324,9.78048318090824,-20.2059510344218));
#58438=CARTESIAN_POINT('Ctrl Pts',(11.664677238709,9.78032664122358,-20.2056359204057));
#58439=CARTESIAN_POINT('Origin',(11.6285182850279,10.5036197352098,-22.9997190259));
#58440=CARTESIAN_POINT('Origin',(1.06052702375292,11.0190788716665,-24.1284170944427));
#58441=CARTESIAN_POINT('Origin',(1.6653400148523,3.42428246167523,-23.8164076546558));
#58442=CARTESIAN_POINT('',(1.95776807072638,3.54233043715926,-21.3065147522487));
#58443=CARTESIAN_POINT('',(1.95776807072638,2.60389771385557,-21.4414410082343));
#58444=CARTESIAN_POINT('Ctrl Pts',(1.95776807072638,3.54233043715926,-21.3065147522487));
#58445=CARTESIAN_POINT('Ctrl Pts',(1.9513478551885,3.54223103321939,-21.3059618726496));
#58446=CARTESIAN_POINT('Ctrl Pts',(1.94501663599459,3.54115156508228,-21.3055798899085));
#58447=CARTESIAN_POINT('Ctrl Pts',(1.92952577557711,3.53620362915063,-21.3050279766058));
#58448=CARTESIAN_POINT('Ctrl Pts',(1.92095957337033,3.53135931038363,-21.3050724139772));
#58449=CARTESIAN_POINT('Ctrl Pts',(1.90072805817451,3.51599592158735,-21.3058205399649));
#58450=CARTESIAN_POINT('Ctrl Pts',(1.8900249560485,3.5036082187607,-21.3069139518805));
#58451=CARTESIAN_POINT('Ctrl Pts',(1.86013121923959,3.46075124654105,-21.3112847102786));
#58452=CARTESIAN_POINT('Ctrl Pts',(1.8458449021105,3.42403619031257,-21.3159449618369));
#58453=CARTESIAN_POINT('Ctrl Pts',(1.82200825445925,3.35110430677947,-21.3254531739389));
#58454=CARTESIAN_POINT('Ctrl Pts',(1.81203215259484,3.30105316932586,-21.3323795986619));
#58455=CARTESIAN_POINT('Ctrl Pts',(1.79984169249385,3.21193645609611,-21.3448875851979));
#58456=CARTESIAN_POINT('Ctrl Pts',(1.79638078494032,3.16936789071309,-21.3509444797466));
#58457=CARTESIAN_POINT('Ctrl Pts',(1.79327894813701,3.08828446690876,-21.3625442583892));
#58458=CARTESIAN_POINT('Ctrl Pts',(1.79337026915323,3.0484033806662,-21.36827974357));
#58459=CARTESIAN_POINT('Ctrl Pts',(1.79687828838528,2.96705307114344,-21.3800426367113));
#58460=CARTESIAN_POINT('Ctrl Pts',(1.80059938175367,2.92417828176263,-21.3862765917232));
#58461=CARTESIAN_POINT('Ctrl Pts',(1.81351118858405,2.83463727606645,-21.3994816448112));
#58462=CARTESIAN_POINT('Ctrl Pts',(1.82404219007374,2.78419034711656,-21.4070273995978));
#58463=CARTESIAN_POINT('Ctrl Pts',(1.84885798811629,2.71258004937781,-21.4183745299768));
#58464=CARTESIAN_POINT('Ctrl Pts',(1.86388962647713,2.67578411025394,-21.4243315771976));
#58465=CARTESIAN_POINT('Ctrl Pts',(1.89490216133537,2.63563438875233,-21.4320245979044));
#58466=CARTESIAN_POINT('Ctrl Pts',(1.90722460488475,2.62233152903849,-21.4347412883587));
#58467=CARTESIAN_POINT('Ctrl Pts',(1.92907437017015,2.60993293818406,-21.4381786237551));
#58468=CARTESIAN_POINT('Ctrl Pts',(1.93579728934589,2.60716195128725,-21.4391080543931));
#58469=CARTESIAN_POINT('Ctrl Pts',(1.94779808654533,2.60440407097883,-21.440500869962));
#58470=CARTESIAN_POINT('Ctrl Pts',(1.95276363818104,2.60385064352413,-21.4410056766482));
#58471=CARTESIAN_POINT('Ctrl Pts',(1.95776807072638,2.60389771385557,-21.4414410082343));
#58472=CARTESIAN_POINT('',(1.65494820650842,5.92795829958164,-23.4551443394205));
#58473=CARTESIAN_POINT('Origin',(1.65494820650842,3.42410087454151,-23.8151446883994));
#58474=CARTESIAN_POINT('',(1.36757616935991,5.62617120112542,-23.4628870820895));
#58475=CARTESIAN_POINT('Origin',(1.6653400148523,5.63137434589457,-23.4990757488526));
#58476=CARTESIAN_POINT('Origin',(1.36757616935991,3.41907931690607,-23.7802189878927));
#58477=CARTESIAN_POINT('Origin',(1.65494820650842,3.42410087454151,-23.8151446883994));
#58478=CARTESIAN_POINT('Origin',(6.4980472271939,3.50872950127857,-24.4037497162211));
#58479=CARTESIAN_POINT('',(11.664677238709,3.69156922144576,-22.1426021244183));
#58480=CARTESIAN_POINT('Ctrl Pts',(11.664677238709,3.69156922144575,-22.1426021244183));
#58481=CARTESIAN_POINT('Ctrl Pts',(8.45131537604982,3.64249119006552,-21.8657713317644));
#58482=CARTESIAN_POINT('Ctrl Pts',(5.17772237568178,3.5921848606183,-21.5838024904321));
#58483=CARTESIAN_POINT('Ctrl Pts',(1.95776807072638,3.54233043715926,-21.3065147522487));
#58484=CARTESIAN_POINT('',(11.3203626311916,6.43344952736807,-24.5814330987647));
#58485=CARTESIAN_POINT('Origin',(11.3203626311916,3.5929949537482,-24.98982881153));
#58486=CARTESIAN_POINT('',(11.664677238709,2.69625718204607,-22.2857063914358));
#58487=CARTESIAN_POINT('Origin',(11.3203626311916,3.5929949537482,-24.98982881153));
#58488=CARTESIAN_POINT('Ctrl Pts',(1.95776807072638,2.60389771385556,-21.4414410082343));
#58489=CARTESIAN_POINT('Ctrl Pts',(5.17772236984729,2.63418372824732,-21.7215422583742));
#58490=CARTESIAN_POINT('Ctrl Pts',(8.45131536953639,2.66535496122478,-22.0062623111724));
#58491=CARTESIAN_POINT('Ctrl Pts',(11.664677238709,2.69625718204608,-22.2857063914358));
#58492=CARTESIAN_POINT('Origin',(11.3307544395355,3.59317654088192,-24.9910917777863));
#58493=CARTESIAN_POINT('',(11.6285182850279,6.14206871845015,-24.6615531749599));
#58494=CARTESIAN_POINT('Origin',(11.6285182850279,3.59837968565107,-25.0272804445494));
#58495=CARTESIAN_POINT('Origin',(11.3307544395355,6.136865573681,-24.6253645081968));
#58496=CARTESIAN_POINT('Ctrl Pts',(11.664677238709,2.69625718204607,-22.2857063914358));
#58497=CARTESIAN_POINT('Ctrl Pts',(11.668173931419,2.6962908089996,-22.2860104748594));
#58498=CARTESIAN_POINT('Ctrl Pts',(11.6716539907387,2.69663467728562,-22.2862755639136));
#58499=CARTESIAN_POINT('Ctrl Pts',(11.6751111337893,2.69727925957648,-22.2865022196842));
#58500=CARTESIAN_POINT('Ctrl Pts',(11.6834715430146,2.69883805296517,-22.2870503413465));
#58501=CARTESIAN_POINT('Ctrl Pts',(11.6912510114763,2.70206385531498,-22.2873454247033));
#58502=CARTESIAN_POINT('Ctrl Pts',(11.709035822972,2.7126169387773,-22.2876313864347));
#58503=CARTESIAN_POINT('Ctrl Pts',(11.7183186554656,2.72116951930899,-22.2874079360076));
#58504=CARTESIAN_POINT('Ctrl Pts',(11.7418333015258,2.74801369053577,-22.2861920544586));
#58505=CARTESIAN_POINT('Ctrl Pts',(11.7542369034695,2.76996803543835,-22.2845703704499));
#58506=CARTESIAN_POINT('Ctrl Pts',(11.7824157539259,2.83096774741555,-22.2794147158946));
#58507=CARTESIAN_POINT('Ctrl Pts',(11.797437382068,2.88153241037196,-22.2742976507484));
#58508=CARTESIAN_POINT('Ctrl Pts',(11.8209603099608,3.00475150470494,-22.2601056375115));
#58509=CARTESIAN_POINT('Ctrl Pts',(11.8274214370012,3.07312747241092,-22.2513392489146));
#58510=CARTESIAN_POINT('Ctrl Pts',(11.8323708659761,3.20740533159247,-22.2328342493678));
#58511=CARTESIAN_POINT('Ctrl Pts',(11.8303885473322,3.27899188856699,-22.2222076907846));
#58512=CARTESIAN_POINT('Ctrl Pts',(11.8177935569394,3.40658761118923,-22.2018688414514));
#58513=CARTESIAN_POINT('Ctrl Pts',(11.8075558566742,3.46929474611099,-22.1912401030956));
#58514=CARTESIAN_POINT('Ctrl Pts',(11.7765253671339,3.57657231689514,-22.1714404504546));
#58515=CARTESIAN_POINT('Ctrl Pts',(11.7586671916648,3.61570515885657,-22.1634661165603));
#58516=CARTESIAN_POINT('Ctrl Pts',(11.7297382659252,3.65639661653937,-22.1542106095143));
#58517=CARTESIAN_POINT('Ctrl Pts',(11.7183817710579,3.66905637710907,-22.1511082048343));
#58518=CARTESIAN_POINT('Ctrl Pts',(11.6971067724022,3.68375234586319,-22.1467808943914));
#58519=CARTESIAN_POINT('Ctrl Pts',(11.688166617688,3.68804578318866,-22.1452727334554));
#58520=CARTESIAN_POINT('Ctrl Pts',(11.6739702938601,3.69116836143546,-22.1434932346172));
#58521=CARTESIAN_POINT('Ctrl Pts',(11.6693161741268,3.69164007241986,-22.1430017682255));
#58522=CARTESIAN_POINT('Ctrl Pts',(11.664677238709,3.69156922144579,-22.1426021244183));
#58523=CARTESIAN_POINT('Origin',(11.6285182850279,3.59837968565107,-25.0272804445494));
#58524=CARTESIAN_POINT('Origin',(1.06052702375292,3.7749681125142,-26.2554799311097));
#58525=CARTESIAN_POINT('Origin',(1.6653400148523,-3.42428246167523,-23.8164076546558));
#58526=CARTESIAN_POINT('',(1.95776807072638,-2.60389771385556,-21.4414410082343));
#58527=CARTESIAN_POINT('',(1.95776807072638,-3.54233043715928,-21.3065147522487));
#58528=CARTESIAN_POINT('Ctrl Pts',(1.95776807072638,-2.60389771385556,-21.4414410082343));
#58529=CARTESIAN_POINT('Ctrl Pts',(1.9513478551885,-2.60383732705435,-21.4408825188176));
#58530=CARTESIAN_POINT('Ctrl Pts',(1.94501663599459,-2.60476545217281,-21.4402118877432));
#58531=CARTESIAN_POINT('Ctrl Pts',(1.92952577557707,-2.60935746998721,-21.4382883361661));
#58532=CARTESIAN_POINT('Ctrl Pts',(1.92095957337023,-2.61401807926046,-21.4369661711994));
#58533=CARTESIAN_POINT('Ctrl Pts',(1.90072805817454,-2.62896991430867,-21.4333556260207));
#58534=CARTESIAN_POINT('Ctrl Pts',(1.89002495604859,-2.64116387786459,-21.4309147278802));
#58535=CARTESIAN_POINT('Ctrl Pts',(1.86013121924006,-2.68351622651802,-21.4230342354907));
#58536=CARTESIAN_POINT('Ctrl Pts',(1.84584490211098,-2.72005700958138,-21.4171618874505));
#58537=CARTESIAN_POINT('Ctrl Pts',(1.82200825445927,-2.79271341229176,-21.4057376641306));
#58538=CARTESIAN_POINT('Ctrl Pts',(1.81203215259485,-2.84268852634673,-21.398282485057));
#58539=CARTESIAN_POINT('Ctrl Pts',(1.79984169249383,-2.93171929355026,-21.3851767307768));
#58540=CARTESIAN_POINT('Ctrl Pts',(1.79638078494031,-2.97426995731992,-21.3789953277718));
#58541=CARTESIAN_POINT('Ctrl Pts',(1.793278948137,-3.05533696803266,-21.367281393569));
#58542=CARTESIAN_POINT('Ctrl Pts',(1.79337026915323,-3.09521846296713,-21.3615487509035));
#58543=CARTESIAN_POINT('Ctrl Pts',(1.79687828838528,-3.17658750331602,-21.3499161335203));
#58544=CARTESIAN_POINT('Ctrl Pts',(1.80059938175368,-3.21948187055685,-21.3438183455158));
#58545=CARTESIAN_POINT('Ctrl Pts',(1.81351118858406,-3.30911612974239,-21.331261884693));
#58546=CARTESIAN_POINT('Ctrl Pts',(1.82404219007374,-3.35964548839957,-21.3242894411135));
#58547=CARTESIAN_POINT('Ctrl Pts',(1.84885798811644,-3.43155192197327,-21.3150019807047));
#58548=CARTESIAN_POINT('Ctrl Pts',(1.86388962647725,-3.46853566116466,-21.3103511116458));
#58549=CARTESIAN_POINT('Ctrl Pts',(1.89490216133386,-3.50922641122945,-21.3064210272649));
#58550=CARTESIAN_POINT('Ctrl Pts',(1.90722460488324,-3.52275579180277,-21.3052798239866));
#58551=CARTESIAN_POINT('Ctrl Pts',(1.92907437017048,-3.53562056190136,-21.3050848364448));
#58552=CARTESIAN_POINT('Ctrl Pts',(1.93579728934604,-3.53854115522866,-21.305195941388));
#58553=CARTESIAN_POINT('Ctrl Pts',(1.94779808654517,-3.54157972349803,-21.3057553534691));
#58554=CARTESIAN_POINT('Ctrl Pts',(1.95276363818094,-3.54225295373074,-21.3060837934058));
#58555=CARTESIAN_POINT('Ctrl Pts',(1.95776807072638,-3.54233043715928,-21.3065147522487));
#58556=CARTESIAN_POINT('',(1.65494820650842,-0.920243449501391,-24.1751450373783));
#58557=CARTESIAN_POINT('Origin',(1.65494820650842,-3.42410087454152,-23.8151446883994));
#58558=CARTESIAN_POINT('',(1.36757616935991,-1.21198743268674,-24.0975508936959));
#58559=CARTESIAN_POINT('Origin',(1.6653400148523,-1.21719057745589,-24.133739560459));
#58560=CARTESIAN_POINT('Origin',(1.36757616935991,-3.41907931690608,-23.7802189878927));
#58561=CARTESIAN_POINT('Origin',(1.65494820650842,-3.42410087454152,-23.8151446883994));
#58562=CARTESIAN_POINT('Origin',(6.4980472271939,-3.50872950127858,-24.4037497162211));
#58563=CARTESIAN_POINT('',(11.664677238709,-2.69625718204607,-22.2857063914358));
#58564=CARTESIAN_POINT('Ctrl Pts',(11.664677238709,-2.69625718204607,-22.2857063914358));
#58565=CARTESIAN_POINT('Ctrl Pts',(8.45131537604982,-2.66535496128742,-22.0062623117388));
#58566=CARTESIAN_POINT('Ctrl Pts',(5.17772237568178,-2.6341837283022,-21.7215422588817));
#58567=CARTESIAN_POINT('Ctrl Pts',(1.95776807072638,-2.60389771385556,-21.4414410082343));
#58568=CARTESIAN_POINT('',(11.3203626311916,-0.752540380128349,-25.3982245242953));
#58569=CARTESIAN_POINT('Origin',(11.3203626311916,-3.59299495374821,-24.98982881153));
#58570=CARTESIAN_POINT('',(11.664677238709,-3.69156922144578,-22.1426021244183));
#58571=CARTESIAN_POINT('Origin',(11.3203626311916,-3.59299495374821,-24.98982881153));
#58572=CARTESIAN_POINT('Ctrl Pts',(1.95776807072638,-3.54233043715928,-21.3065147522487));
#58573=CARTESIAN_POINT('Ctrl Pts',(5.17772236984729,-3.59218486052798,-21.5838024899296));
#58574=CARTESIAN_POINT('Ctrl Pts',(8.45131536953638,-3.64249118996606,-21.8657713312033));
#58575=CARTESIAN_POINT('Ctrl Pts',(11.664677238709,-3.69156922144577,-22.1426021244183));
#58576=CARTESIAN_POINT('Origin',(11.3307544395355,-3.59317654088193,-24.9910917777863));
#58577=CARTESIAN_POINT('',(11.6285182850279,-1.054690652852,-25.393007714139));
#58578=CARTESIAN_POINT('Origin',(11.6285182850279,-3.59837968565108,-25.0272804445494));
#58579=CARTESIAN_POINT('Origin',(11.3307544395355,-1.04948750808285,-25.3568190473759));
#58580=CARTESIAN_POINT('Ctrl Pts',(11.664677238709,-3.69156922144578,-22.1426021244183));
#58581=CARTESIAN_POINT('Ctrl Pts',(11.6681739314189,-3.69162262682055,-22.1429033641341));
#58582=CARTESIAN_POINT('Ctrl Pts',(11.6716539907387,-3.69136737183329,-22.1432545941105));
#58583=CARTESIAN_POINT('Ctrl Pts',(11.6751111337893,-3.69081275596405,-22.1436536685467));
#58584=CARTESIAN_POINT('Ctrl Pts',(11.6834715430144,-3.68947152837769,-22.1446187502773));
#58585=CARTESIAN_POINT('Ctrl Pts',(11.691251011476,-3.68645952827763,-22.1458106942287));
#58586=CARTESIAN_POINT('Ctrl Pts',(11.7090358229721,-3.67641448357506,-22.1490582196872));
#58587=CARTESIAN_POINT('Ctrl Pts',(11.7183186554659,-3.66814538938815,-22.1512533609532));
#58588=CARTESIAN_POINT('Ctrl Pts',(11.7418333015258,-3.64204604229627,-22.1576496081462));
#58589=CARTESIAN_POINT('Ctrl Pts',(11.7542369034694,-3.62052412143989,-22.1622788674575));
#58590=CARTESIAN_POINT('Ctrl Pts',(11.7824157539265,-3.560542810664,-22.1745176579595));
#58591=CARTESIAN_POINT('Ctrl Pts',(11.7974373820683,-3.51058472799645,-22.1838535816868));
#58592=CARTESIAN_POINT('Ctrl Pts',(11.8209603099608,-3.38835852059437,-22.2049512752024));
#58593=CARTESIAN_POINT('Ctrl Pts',(11.8274214370012,-3.32028248294269,-22.215803723148));
#58594=CARTESIAN_POINT('Ctrl Pts',(11.8323708659761,-3.1862303597095,-22.2358787507005));
#58595=CARTESIAN_POINT('Ctrl Pts',(11.8303885473322,-3.11454971376705,-22.2458509061382));
#58596=CARTESIAN_POINT('Ctrl Pts',(11.8177935569394,-2.9863923984218,-22.2622837922879));
#58597=CARTESIAN_POINT('Ctrl Pts',(11.8075558566742,-2.92323088143592,-22.2697522339708));
#58598=CARTESIAN_POINT('Ctrl Pts',(11.7765253671338,-2.81472059927844,-22.2809781906907));
#58599=CARTESIAN_POINT('Ctrl Pts',(11.7586671916646,-2.774926282902,-22.2843518689721));
#58600=CARTESIAN_POINT('Ctrl Pts',(11.7297382659251,-2.73327553750453,-22.2869353834087));
#58601=CARTESIAN_POINT('Ctrl Pts',(11.7183817710579,-2.72025453778751,-22.2875253146313));
#58602=CARTESIAN_POINT('Ctrl Pts',(11.6971067724022,-2.70493471479219,-22.287513623519));
#58603=CARTESIAN_POINT('Ctrl Pts',(11.688166617688,-2.70039029380909,-22.2872761547732));
#58604=CARTESIAN_POINT('Ctrl Pts',(11.6739702938601,-2.69689285916415,-22.2864484700947));
#58605=CARTESIAN_POINT('Ctrl Pts',(11.6693161741268,-2.69630179370591,-22.2861098078869));
#58606=CARTESIAN_POINT('Ctrl Pts',(11.664677238709,-2.69625718204607,-22.2857063914358));
#58607=CARTESIAN_POINT('Origin',(11.6285182850279,-3.59837968565108,-25.0272804445494));
#58608=CARTESIAN_POINT('Origin',(1.06052702375292,-3.77496811251421,-26.2554799311097));
#58609=CARTESIAN_POINT('Origin',(1.6653400148523,-9.99543238497271,-21.8869439481057));
#58610=CARTESIAN_POINT('',(1.95776807072638,-8.5391735580698,-19.8393092308925));
#58611=CARTESIAN_POINT('',(1.95776807072638,-9.40158004320575,-19.4454613857581));
#58612=CARTESIAN_POINT('Ctrl Pts',(1.95776807072638,-8.53917355806981,-19.8393092308925));
#58613=CARTESIAN_POINT('Ctrl Pts',(1.95134736181011,-8.53895825616284,-19.8387903372766));
#58614=CARTESIAN_POINT('Ctrl Pts',(1.94501567122114,-8.53965997172107,-19.8378852898844));
#58615=CARTESIAN_POINT('Ctrl Pts',(1.92948836979265,-8.54353347509979,-19.8347384067269));
#58616=CARTESIAN_POINT('Ctrl Pts',(1.92089186233923,-8.54765577357349,-19.8321439694452));
#58617=CARTESIAN_POINT('Ctrl Pts',(1.90046800930119,-8.56114336986581,-19.8243804604408));
#58618=CARTESIAN_POINT('Ctrl Pts',(1.88964186308534,-8.57236355197267,-19.8185013079906));
#58619=CARTESIAN_POINT('Ctrl Pts',(1.85810283833392,-8.61322946498746,-19.7977884699129));
#58620=CARTESIAN_POINT('Ctrl Pts',(1.84335629303589,-8.64977779572316,-19.7804322617416));
#58621=CARTESIAN_POINT('Ctrl Pts',(1.81854010589147,-8.72212855294446,-19.7463114584516));
#58622=CARTESIAN_POINT('Ctrl Pts',(1.80836917826458,-8.7744055915797,-19.7221699251048));
#58623=CARTESIAN_POINT('Ctrl Pts',(1.79896764765284,-8.85022287567158,-19.6873082756821));
#58624=CARTESIAN_POINT('Ctrl Pts',(1.79670145400053,-8.87696000159258,-19.6750497681666));
#58625=CARTESIAN_POINT('Ctrl Pts',(1.79434535609109,-8.922675236925,-19.6541233115617));
#58626=CARTESIAN_POINT('Ctrl Pts',(1.7938155730381,-8.94195225085071,-19.6453095312537));
#58627=CARTESIAN_POINT('Ctrl Pts',(1.79365032105972,-8.97982124967063,-19.6280120764217));
#58628=CARTESIAN_POINT('Ctrl Pts',(1.79398945985935,-8.99855959580199,-19.6194610836778));
#58629=CARTESIAN_POINT('Ctrl Pts',(1.79575501944584,-9.04148989103746,-19.5998915295602));
#58630=CARTESIAN_POINT('Ctrl Pts',(1.79749007695657,-9.06591922657842,-19.588770848701));
#58631=CARTESIAN_POINT('Ctrl Pts',(1.80455267777008,-9.1332144340572,-19.5582064365159));
#58632=CARTESIAN_POINT('Ctrl Pts',(1.81186451913826,-9.17780246249345,-19.5380267681685));
#58633=CARTESIAN_POINT('Ctrl Pts',(1.83578355229033,-9.26860855269313,-19.4974487611261));
#58634=CARTESIAN_POINT('Ctrl Pts',(1.8521450534642,-9.3082800577872,-19.4800807834256));
#58635=CARTESIAN_POINT('Ctrl Pts',(1.88061329933269,-9.35308369492277,-19.4613517855849));
#58636=CARTESIAN_POINT('Ctrl Pts',(1.8944859507649,-9.37144648654039,-19.4538614563447));
#58637=CARTESIAN_POINT('Ctrl Pts',(1.92022261572022,-9.39019230245402,-19.4473163375408));
#58638=CARTESIAN_POINT('Ctrl Pts',(1.92864558703654,-9.39485547755033,-19.445881781225));
#58639=CARTESIAN_POINT('Ctrl Pts',(1.94192278721307,-9.39926212836097,-19.4450422071836));
#58640=CARTESIAN_POINT('Ctrl Pts',(1.94616291414767,-9.40028474102502,-19.4449598654854));
#58641=CARTESIAN_POINT('Ctrl Pts',(1.95291207288063,-9.4012618712514,-19.4451433237978));
#58642=CARTESIAN_POINT('Ctrl Pts',(1.95533909580059,-9.40148502823929,-19.4452712818103));
#58643=CARTESIAN_POINT('Ctrl Pts',(1.95776807072638,-9.40158004320576,-19.4454613857581));
#58644=CARTESIAN_POINT('',(1.65494820650842,-7.69389254720435,-22.9366192595313));
#58645=CARTESIAN_POINT('Origin',(1.65494820650842,-9.99490233468121,-21.8857832998643));
#58646=CARTESIAN_POINT('',(1.36757616935991,-7.95195805266942,-22.7799744455484));
#58647=CARTESIAN_POINT('Origin',(1.6653400148523,-7.96714595913197,-22.8132313217527));
#58648=CARTESIAN_POINT('Origin',(1.36757616935991,-9.98024447851016,-21.8536870719015));
#58649=CARTESIAN_POINT('Origin',(1.65494820650842,-9.99490233468121,-21.8857832998643));
#58650=CARTESIAN_POINT('Origin',(6.4980472271939,-10.24193210686,-22.4267030489007));
#58651=CARTESIAN_POINT('',(11.664677238709,-8.86564886390744,-20.6233552648184));
#58652=CARTESIAN_POINT('Ctrl Pts',(11.664677238709,-8.86564886390743,-20.6233552648184));
#58653=CARTESIAN_POINT('Ctrl Pts',(8.44908820479151,-8.75719478802904,-20.3637569933514));
#58654=CARTESIAN_POINT('Ctrl Pts',(5.17648536371073,-8.64710493764476,-20.0994318866049));
#58655=CARTESIAN_POINT('Ctrl Pts',(1.95776807072638,-8.5391735580698,-19.8393092308925));
#58656=CARTESIAN_POINT('',(11.3203626311916,-7.87756394155673,-24.1574028479247));
#58657=CARTESIAN_POINT('Origin',(11.3203626311916,-10.4879017784557,-22.9653015014543));
#58658=CARTESIAN_POINT('',(11.664677238709,-9.78032664122357,-20.2056359204057));
#58659=CARTESIAN_POINT('Origin',(11.3203626311916,-10.4879017784557,-22.9653015014543));
#58660=CARTESIAN_POINT('Ctrl Pts',(1.95776807072638,-9.40158004320575,-19.4454613857581));
#58661=CARTESIAN_POINT('Ctrl Pts',(5.17648535775567,-9.52748760686313,-19.6973745927009));
#58662=CARTESIAN_POINT('Ctrl Pts',(8.44908819833864,-9.65515767353718,-19.9536710836342));
#58663=CARTESIAN_POINT('Ctrl Pts',(11.664677238709,-9.78032664122359,-20.2056359204057));
#58664=CARTESIAN_POINT('Origin',(11.3307544395355,-10.4884318287472,-22.9664621496957));
#58665=CARTESIAN_POINT('',(11.6285182850279,-8.16600525994691,-24.0672717863504));
#58666=CARTESIAN_POINT('Origin',(11.6285182850279,-10.5036197352098,-22.9997190259));
#58667=CARTESIAN_POINT('Origin',(11.3307544395355,-8.15081735348436,-24.0340149101461));
#58668=CARTESIAN_POINT('Ctrl Pts',(11.664677238709,-9.78032664122358,-20.2056359204057));
#58669=CARTESIAN_POINT('Ctrl Pts',(11.6681531449969,-9.78046194321534,-20.205908282996));
#58670=CARTESIAN_POINT('Ctrl Pts',(11.6716331726355,-9.78031931733511,-20.2063155813886));
#58671=CARTESIAN_POINT('Ctrl Pts',(11.6751111337893,-9.77989707212503,-20.2068579905627));
#58672=CARTESIAN_POINT('Ctrl Pts',(11.6835034416364,-9.77887819594063,-20.2081668219633));
#58673=CARTESIAN_POINT('Ctrl Pts',(11.6913221163003,-9.77630619887358,-20.210171496446));
#58674=CARTESIAN_POINT('Ctrl Pts',(11.7093237578239,-9.76744342252662,-20.2162060047083));
#58675=CARTESIAN_POINT('Ctrl Pts',(11.7187565997267,-9.75994125246948,-20.2207464637378));
#58676=CARTESIAN_POINT('Ctrl Pts',(11.7431727782355,-9.73554353144944,-20.2348815339297));
#58677=CARTESIAN_POINT('Ctrl Pts',(11.7560898230284,-9.7147721142081,-20.2461192329191));
#58678=CARTESIAN_POINT('Ctrl Pts',(11.7841758181735,-9.65887107077546,-20.27559793086));
#58679=CARTESIAN_POINT('Ctrl Pts',(11.7988195826632,-9.61329277429603,-20.2987092511704));
#58680=CARTESIAN_POINT('Ctrl Pts',(11.8183861888449,-9.51775570080867,-20.3455413475508));
#58681=CARTESIAN_POINT('Ctrl Pts',(11.8239771978735,-9.47339867533899,-20.3667719341833));
#58682=CARTESIAN_POINT('Ctrl Pts',(11.8302306705076,-9.39045122916041,-20.405743767947));
#58683=CARTESIAN_POINT('Ctrl Pts',(11.8313291886565,-9.35006360841451,-20.4243852490074));
#58684=CARTESIAN_POINT('Ctrl Pts',(11.8301000822046,-9.26938684912614,-20.4610118195814));
#58685=CARTESIAN_POINT('Ctrl Pts',(11.8275983467482,-9.2278269490101,-20.4795461377865));
#58686=CARTESIAN_POINT('Ctrl Pts',(11.8179490511515,-9.14115299922197,-20.5174708042373));
#58687=CARTESIAN_POINT('Ctrl Pts',(11.8098404493788,-9.09351673143953,-20.5378464526579));
#58688=CARTESIAN_POINT('Ctrl Pts',(11.7817370234729,-8.9887774307,-20.5812669850615));
#58689=CARTESIAN_POINT('Ctrl Pts',(11.7608617911997,-8.94282298913096,-20.599208223942));
#58690=CARTESIAN_POINT('Ctrl Pts',(11.7278645691759,-8.89938954507,-20.6148437040365));
#58691=CARTESIAN_POINT('Ctrl Pts',(11.7163738956146,-8.88734402205839,-20.6189424909766));
#58692=CARTESIAN_POINT('Ctrl Pts',(11.6949981921877,-8.87337129041363,-20.6229224329418));
#58693=CARTESIAN_POINT('Ctrl Pts',(11.6861739271888,-8.86930788707863,-20.6238292881645));
#58694=CARTESIAN_POINT('Ctrl Pts',(11.6727399598044,-8.86630070859597,-20.6238428740718));
#58695=CARTESIAN_POINT('Ctrl Pts',(11.6686987410324,-8.86578449949814,-20.6236799254143));
#58696=CARTESIAN_POINT('Ctrl Pts',(11.664677238709,-8.86564886390742,-20.6233552648184));
#58697=CARTESIAN_POINT('Origin',(11.6285182850279,-10.5036197352098,-22.9997190259));
#58698=CARTESIAN_POINT('Origin',(1.06052702375292,-11.0190788716665,-24.1284170944427));
#58699=CARTESIAN_POINT('Origin',(1.6653400148523,-15.756811821565,-18.1843302095478));
#58700=CARTESIAN_POINT('',(1.95776807072638,-13.7826563450298,-16.6299146085789));
#58701=CARTESIAN_POINT('',(1.95776807072638,-14.4991695475011,-16.0090523844052));
#58702=CARTESIAN_POINT('Ctrl Pts',(1.95776807072638,-13.7826563450298,-16.6299146085789));
#58703=CARTESIAN_POINT('Ctrl Pts',(1.95134736176265,-13.7823035751351,-16.6294773913538));
#58704=CARTESIAN_POINT('Ctrl Pts',(1.94501567114707,-13.7827218849829,-16.6284113086055));
#58705=CARTESIAN_POINT('Ctrl Pts',(1.92948836979158,-13.7855519048069,-16.6243006043354));
#58706=CARTESIAN_POINT('Ctrl Pts',(1.92089186233812,-13.7887762837787,-16.6206498743041));
#58707=CARTESIAN_POINT('Ctrl Pts',(1.90046800929984,-13.7995303044108,-16.6094009469743));
#58708=CARTESIAN_POINT('Ctrl Pts',(1.88964186308388,-13.8086396416535,-16.600598850914));
#58709=CARTESIAN_POINT('Ctrl Pts',(1.85810283833188,-13.842014717222,-16.5692117701521));
#58710=CARTESIAN_POINT('Ctrl Pts',(1.84335629303374,-13.8721927748564,-16.5422617556955));
#58711=CARTESIAN_POINT('Ctrl Pts',(1.81854010589022,-13.9319998768941,-16.4891395208629));
#58712=CARTESIAN_POINT('Ctrl Pts',(1.80836917826387,-13.975357872229,-16.4512477454867));
#58713=CARTESIAN_POINT('Ctrl Pts',(1.79896764765255,-14.038282361965,-16.3964380405179));
#58714=CARTESIAN_POINT('Ctrl Pts',(1.79670145400034,-14.0604828257552,-16.3771433698416));
#58715=CARTESIAN_POINT('Ctrl Pts',(1.79434535609103,-14.0984506087182,-16.3441851116304));
#58716=CARTESIAN_POINT('Ctrl Pts',(1.79381557303806,-14.1144636392704,-16.3302973889325));
#58717=CARTESIAN_POINT('Ctrl Pts',(1.79365032105973,-14.1459254213794,-16.3030316726971));
#58718=CARTESIAN_POINT('Ctrl Pts',(1.7939894598594,-14.1614956397804,-16.2895478530753));
#58719=CARTESIAN_POINT('Ctrl Pts',(1.79575501944596,-14.1971735758964,-16.2586761415598));
#58720=CARTESIAN_POINT('Ctrl Pts',(1.79749007695676,-14.2174802938461,-16.2411233872494));
#58721=CARTESIAN_POINT('Ctrl Pts',(1.8045526777706,-14.2734385825878,-16.192837797648));
#58722=CARTESIAN_POINT('Ctrl Pts',(1.81186451913917,-14.3105352130209,-16.1609136484021));
#58723=CARTESIAN_POINT('Ctrl Pts',(1.83578355229256,-14.3862308728547,-16.0963963037919));
#58724=CARTESIAN_POINT('Ctrl Pts',(1.85214505346734,-14.4194022784807,-16.0685550966583));
#58725=CARTESIAN_POINT('Ctrl Pts',(1.88061329933679,-14.4571144850547,-16.0379621115825));
#58726=CARTESIAN_POINT('Ctrl Pts',(1.8944859507685,-14.4726231849777,-16.0256017970747));
#58727=CARTESIAN_POINT('Ctrl Pts',(1.92022261572266,-14.4887656905743,-16.0140404949249));
#58728=CARTESIAN_POINT('Ctrl Pts',(1.92864558703852,-14.4928358130947,-16.0113502799772));
#58729=CARTESIAN_POINT('Ctrl Pts',(1.94192278721418,-14.4968274282428,-16.0093032175839));
#58730=CARTESIAN_POINT('Ctrl Pts',(1.94616291414861,-14.4977854195714,-16.0089361080226));
#58731=CARTESIAN_POINT('Ctrl Pts',(1.95291207280144,-14.4987746553256,-16.0088368455885));
#58732=CARTESIAN_POINT('Ctrl Pts',(1.95533909573991,-14.4990248228335,-16.0088967498086));
#58733=CARTESIAN_POINT('Ctrl Pts',(1.95776807072638,-14.4991695475011,-16.0090523844052));
#58734=CARTESIAN_POINT('',(1.65494820650842,-13.8442282280737,-19.8399049986041));
#58735=CARTESIAN_POINT('Origin',(1.65494820650842,-15.755976249638,-18.1833659081392));
#58736=CARTESIAN_POINT('',(1.36757616935991,-14.0477083233403,-19.6168999455472));
#58737=CARTESIAN_POINT('Origin',(1.6653400148523,-14.0716505576406,-19.6445307568688));
#58738=CARTESIAN_POINT('Origin',(1.36757616935991,-15.7328695872647,-18.1566993982262));
#58739=CARTESIAN_POINT('Origin',(1.65494820650842,-15.755976249638,-18.1833659081392));
#58740=CARTESIAN_POINT('Origin',(6.4980472271939,-16.1453942842592,-18.6327782772971));
#58741=CARTESIAN_POINT('',(11.664677238709,-14.316798400859,-17.2902225464619));
#58742=CARTESIAN_POINT('Ctrl Pts',(11.664677238709,-14.316798400859,-17.2902225464619));
#58743=CARTESIAN_POINT('Ctrl Pts',(8.44646649976651,-14.1394557206779,-17.0715167051139));
#58744=CARTESIAN_POINT('Ctrl Pts',(5.17487115867276,-13.9594120777672,-16.848982766429));
#58745=CARTESIAN_POINT('Ctrl Pts',(1.95776807072638,-13.7826563450298,-16.6299146085789));
#58746=CARTESIAN_POINT('',(11.3203626311916,-14.3643941221169,-20.959492062422));
#58747=CARTESIAN_POINT('Origin',(11.3203626311916,-16.5331411750263,-19.0802620436377));
#58748=CARTESIAN_POINT('',(11.664677238709,-15.0767401623717,-16.6317292616657));
#58749=CARTESIAN_POINT('Origin',(11.3203626311916,-16.5331411750263,-19.0802620436377));
#58750=CARTESIAN_POINT('Ctrl Pts',(1.95776807072638,-14.4991695475011,-16.0090523844052));
#58751=CARTESIAN_POINT('Ctrl Pts',(5.17487115257265,-14.6908529434927,-16.2151856477085));
#58752=CARTESIAN_POINT('Ctrl Pts',(8.44646649340719,-14.8854989256118,-16.4250665874126));
#58753=CARTESIAN_POINT('Ctrl Pts',(11.664677238709,-15.0767401623716,-16.6317292616657));
#58754=CARTESIAN_POINT('Origin',(11.3307544395355,-16.5339767469533,-19.0812263450464));
#58755=CARTESIAN_POINT('',(11.6285182850279,-14.6157586859842,-20.7917486320082));
#58756=CARTESIAN_POINT('Origin',(11.6285182850279,-16.5579189812536,-19.1088571563679));
#58757=CARTESIAN_POINT('Origin',(11.3307544395355,-14.5918164516839,-20.7641178206866));
#58758=CARTESIAN_POINT('Ctrl Pts',(11.664677238709,-15.0767401623716,-16.6317292616657));
#58759=CARTESIAN_POINT('Ctrl Pts',(11.6681719057554,-15.0769478319436,-16.6319536774342));
#58760=CARTESIAN_POINT('Ctrl Pts',(11.6716519636862,-15.076923254483,-16.6323869095799));
#58761=CARTESIAN_POINT('Ctrl Pts',(11.6751111337893,-15.0766722907899,-16.6330228529951));
#58762=CARTESIAN_POINT('Ctrl Pts',(11.6833639439589,-15.0760735472598,-16.6345400724807));
#58763=CARTESIAN_POINT('Ctrl Pts',(11.6912209922801,-15.0742040415111,-16.6371623459814));
#58764=CARTESIAN_POINT('Ctrl Pts',(11.7092716451022,-15.0673685087776,-16.6454839841326));
#58765=CARTESIAN_POINT('Ctrl Pts',(11.7188321121789,-15.0614159673375,-16.6519996438999));
#58766=CARTESIAN_POINT('Ctrl Pts',(11.7448362096949,-15.0406027082651,-16.6738751139888));
#58767=CARTESIAN_POINT('Ctrl Pts',(11.7582763496123,-15.022038377504,-16.6921848294475));
#58768=CARTESIAN_POINT('Ctrl Pts',(11.7901173768951,-14.9694389699161,-16.7431769315634));
#58769=CARTESIAN_POINT('Ctrl Pts',(11.8074969006878,-14.9187368040632,-16.7905186715063));
#58770=CARTESIAN_POINT('Ctrl Pts',(11.8229354401012,-14.8329485272452,-16.8679921932309));
#58771=CARTESIAN_POINT('Ctrl Pts',(11.826199199177,-14.806478516273,-16.8916135343913));
#58772=CARTESIAN_POINT('Ctrl Pts',(11.8295237141305,-14.7632021791261,-16.9298134645279));
#58773=CARTESIAN_POINT('Ctrl Pts',(11.8303434615844,-14.7461967949088,-16.9447232097655));
#58774=CARTESIAN_POINT('Ctrl Pts',(11.8309946485842,-14.7141892768629,-16.9725964133232));
#58775=CARTESIAN_POINT('Ctrl Pts',(11.8309459330901,-14.6991103672785,-16.9856519542831));
#58776=CARTESIAN_POINT('Ctrl Pts',(11.8300359252892,-14.6661973816186,-17.0139777482937));
#58777=CARTESIAN_POINT('Ctrl Pts',(11.8290394062419,-14.648205145668,-17.0293561720867));
#58778=CARTESIAN_POINT('Ctrl Pts',(11.8249644421306,-14.6008656924252,-17.0695195134069));
#58779=CARTESIAN_POINT('Ctrl Pts',(11.8209395722477,-14.5708013862499,-17.0947280327935));
#58780=CARTESIAN_POINT('Ctrl Pts',(11.8028867656276,-14.4800669368871,-17.1697247641803));
#58781=CARTESIAN_POINT('Ctrl Pts',(11.7841990134598,-14.42738184272,-17.211775010527));
#58782=CARTESIAN_POINT('Ctrl Pts',(11.7507704380578,-14.3734252802354,-17.2529915779606));
#58783=CARTESIAN_POINT('Ctrl Pts',(11.737145998644,-14.3544245174278,-17.2672530332855));
#58784=CARTESIAN_POINT('Ctrl Pts',(11.7101248465184,-14.3325674214146,-17.2823211517671));
#58785=CARTESIAN_POINT('Ctrl Pts',(11.700195678653,-14.3262661007535,-17.2864153990732));
#58786=CARTESIAN_POINT('Ctrl Pts',(11.6812735959896,-14.3191264193213,-17.290180232345));
#58787=CARTESIAN_POINT('Ctrl Pts',(11.6731643433662,-14.3172676724499,-17.2907980108076));
#58788=CARTESIAN_POINT('Ctrl Pts',(11.6646867061662,-14.3167989230148,-17.2902231894927));
#58789=CARTESIAN_POINT('Ctrl Pts',(11.664681972407,-14.3167986617141,-17.2902228681585));
#58790=CARTESIAN_POINT('Ctrl Pts',(11.664677238709,-14.316798400859,-17.2902225464619));
#58791=CARTESIAN_POINT('Origin',(11.6285182850279,-16.5579189812536,-19.1088571563679));
#58792=CARTESIAN_POINT('Origin',(1.06052702375292,-17.3704893936218,-20.0466134020057));
#58793=CARTESIAN_POINT('Origin',(1.6653400148523,-20.2416680737422,-13.0085301837882));
#58794=CARTESIAN_POINT('',(1.95776807072638,-17.9095502835289,-12.0732632065885));
#58795=CARTESIAN_POINT('',(1.95776807072638,-18.4221225649395,-11.2756851683683));
#58796=CARTESIAN_POINT('Ctrl Pts',(1.95776807072638,-17.9095502835289,-12.0732632065885));
#58797=CARTESIAN_POINT('Ctrl Pts',(1.95134736183621,-17.9090886249723,-12.0729430865012));
#58798=CARTESIAN_POINT('Ctrl Pts',(1.94501567126188,-17.9091896400968,-12.0718023361232));
#58799=CARTESIAN_POINT('Ctrl Pts',(1.92948836979328,-17.9107469050198,-12.0670608355043));
#58800=CARTESIAN_POINT('Ctrl Pts',(1.92089186233993,-17.9128121444813,-12.062649573159));
#58801=CARTESIAN_POINT('Ctrl Pts',(1.90046800930196,-17.919961362657,-12.0488265486971));
#58802=CARTESIAN_POINT('Ctrl Pts',(1.88964186308622,-17.9262218707066,-12.0378146025024));
#58803=CARTESIAN_POINT('Ctrl Pts',(1.8581028383352,-17.9494022586918,-11.9982960736773));
#58804=CARTESIAN_POINT('Ctrl Pts',(1.8433562930373,-17.9707651964678,-11.9639355828322));
#58805=CARTESIAN_POINT('Ctrl Pts',(1.81854010589216,-18.0131834276005,-11.8961155639935));
#58806=CARTESIAN_POINT('Ctrl Pts',(1.80836917826496,-18.0441097727155,-11.847543312875));
#58807=CARTESIAN_POINT('Ctrl Pts',(1.79896764765298,-18.0890437001663,-11.7772259086882));
#58808=CARTESIAN_POINT('Ctrl Pts',(1.79670145400062,-18.1049089522812,-11.752458214319));
#58809=CARTESIAN_POINT('Ctrl Pts',(1.79434535609112,-18.1320533589037,-11.71013823657));
#58810=CARTESIAN_POINT('Ctrl Pts',(1.79381557303812,-18.1435051255807,-11.6923016721812));
#58811=CARTESIAN_POINT('Ctrl Pts',(1.79365032105971,-18.1660108445022,-11.657276600717));
#58812=CARTESIAN_POINT('Ctrl Pts',(1.79398945985931,-18.1771515286775,-11.6399523330916));
#58813=CARTESIAN_POINT('Ctrl Pts',(1.79575501944576,-18.2026866914744,-11.6002795066445));
#58814=CARTESIAN_POINT('Ctrl Pts',(1.79749007695645,-18.2172256623124,-11.5777166986477));
#58815=CARTESIAN_POINT('Ctrl Pts',(1.8045526777698,-18.2573136245575,-11.5156217429364));
#58816=CARTESIAN_POINT('Ctrl Pts',(1.81186451913778,-18.2839135086097,-11.4745394175059));
#58817=CARTESIAN_POINT('Ctrl Pts',(1.83578355228869,-18.3383663258931,-11.3913095468931));
#58818=CARTESIAN_POINT('Ctrl Pts',(1.85214505346182,-18.3623502820448,-11.3552506393502));
#58819=CARTESIAN_POINT('Ctrl Pts',(1.88061329933037,-18.3899158393672,-11.3152721287427));
#58820=CARTESIAN_POINT('Ctrl Pts',(1.8944859507629,-18.4013140249654,-11.2990431881354));
#58821=CARTESIAN_POINT('Ctrl Pts',(1.92022261571886,-18.4135454504487,-11.2834023305784));
#58822=CARTESIAN_POINT('Ctrl Pts',(1.92864558703543,-18.4166927832737,-11.2796744022134));
#58823=CARTESIAN_POINT('Ctrl Pts',(1.94192278721233,-18.4199459858402,-11.2765856922882));
#58824=CARTESIAN_POINT('Ctrl Pts',(1.94616291414708,-18.4207617450736,-11.275963555897));
#58825=CARTESIAN_POINT('Ctrl Pts',(1.95291207297762,-18.4216829443939,-11.2755896143607));
#58826=CARTESIAN_POINT('Ctrl Pts',(1.95533909587482,-18.4219398553151,-11.2755766117231));
#58827=CARTESIAN_POINT('Ctrl Pts',(1.95776807072638,-18.4221225649395,-11.2756851683683));
#58828=CARTESIAN_POINT('',(1.65494820650842,-18.8729868727,-15.1358796271483));
#58829=CARTESIAN_POINT('Origin',(1.65494820650842,-20.2405946732479,-13.0078403511776));
#58830=CARTESIAN_POINT('',(1.36757616935991,-19.0053968105924,-14.8645808781538));
#58831=CARTESIAN_POINT('Origin',(1.6653400148523,-19.0361537152975,-14.8843471405862));
#58832=CARTESIAN_POINT('Origin',(1.36757616935991,-20.2109111690372,-12.9887639213558));
#58833=CARTESIAN_POINT('Origin',(1.65494820650842,-20.2405946732479,-13.0078403511776));
#58834=CARTESIAN_POINT('Origin',(6.4980472271939,-20.7408526371047,-13.3293366230661));
#58835=CARTESIAN_POINT('',(11.664677238709,-18.6080860766515,-12.5563388263038));
#58836=CARTESIAN_POINT('Ctrl Pts',(11.664677238709,-18.6080860766515,-12.5563388263039));
#58837=CARTESIAN_POINT('Ctrl Pts',(8.44760841234031,-18.3763927057865,-12.3965120461773));
#58838=CARTESIAN_POINT('Ctrl Pts',(5.17558411912346,-18.1409160622912,-12.2336952666484));
#58839=CARTESIAN_POINT('Ctrl Pts',(1.95776807072638,-17.9095502835289,-12.0732632065885));
#58840=CARTESIAN_POINT('',(11.3203626311916,-19.6875065192443,-16.0635678809207));
#58841=CARTESIAN_POINT('Origin',(11.3203626311916,-21.2389637999728,-13.6494532297333));
#58842=CARTESIAN_POINT('',(11.664677238709,-19.1517258603906,-11.7104188108481));
#58843=CARTESIAN_POINT('Origin',(11.3203626311916,-21.2389637999728,-13.6494532297333));
#58844=CARTESIAN_POINT('Ctrl Pts',(1.95776807072638,-18.4221225649395,-11.2756851683683));
#58845=CARTESIAN_POINT('Ctrl Pts',(5.17558411308691,-18.6641695173893,-11.4194969967751));
#58846=CARTESIAN_POINT('Ctrl Pts',(8.44760840593807,-18.9100934023218,-11.5660575512547));
#58847=CARTESIAN_POINT('Ctrl Pts',(11.664677238709,-19.1517258603906,-11.710418810848));
#58848=CARTESIAN_POINT('Origin',(11.3307544395355,-21.2400372004671,-13.6501430623439));
#58849=CARTESIAN_POINT('',(11.6285182850279,-19.8814302665469,-15.831801656791));
#58850=CARTESIAN_POINT('Origin',(11.6285182850279,-21.2707941051722,-13.6699093247763));
#58851=CARTESIAN_POINT('Origin',(11.3307544395355,-19.8506733618418,-15.8120353943587));
#58852=CARTESIAN_POINT('Ctrl Pts',(11.664677238709,-19.1517258603906,-11.710418810848));
#58853=CARTESIAN_POINT('Ctrl Pts',(11.6681719057554,-19.151988343114,-11.7105756289215));
#58854=CARTESIAN_POINT('Ctrl Pts',(11.6716519636862,-19.1520868168133,-11.7109982363922));
#58855=CARTESIAN_POINT('Ctrl Pts',(11.6751111337893,-19.1520251848775,-11.7116791242736));
#58856=CARTESIAN_POINT('Ctrl Pts',(11.6833639439589,-19.1518781447924,-11.713303571255));
#58857=CARTESIAN_POINT('Ctrl Pts',(11.6912209922801,-19.1508231469805,-11.7163463248885));
#58858=CARTESIAN_POINT('Ctrl Pts',(11.7092716451022,-19.1466089777452,-11.7262566703379));
#58859=CARTESIAN_POINT('Ctrl Pts',(11.7188321121789,-19.142733229544,-11.7341854248227));
#58860=CARTESIAN_POINT('Ctrl Pts',(11.7448362096951,-19.1289260858263,-11.7610385573624));
#58861=CARTESIAN_POINT('Ctrl Pts',(11.7582763496125,-19.1162721838523,-11.7838367770654));
#58862=CARTESIAN_POINT('Ctrl Pts',(11.7901173768954,-19.080169557163,-11.8475823063438));
#58863=CARTESIAN_POINT('Ctrl Pts',(11.807496900688,-19.0448588947193,-11.9072908240012));
#58864=CARTESIAN_POINT('Ctrl Pts',(11.8229354401012,-18.9843724592575,-12.0057954743111));
#58865=CARTESIAN_POINT('Ctrl Pts',(11.826199199177,-18.9656295705594,-12.0359174490525));
#58866=CARTESIAN_POINT('Ctrl Pts',(11.8295237141305,-18.9348683931316,-12.0847623667265));
#58867=CARTESIAN_POINT('Ctrl Pts',(11.8303434615844,-18.9227524071091,-12.103859132896));
#58868=CARTESIAN_POINT('Ctrl Pts',(11.8309946485842,-18.8998942073469,-12.139620835759));
#58869=CARTESIAN_POINT('Ctrl Pts',(11.8309459330901,-18.8891042704865,-12.1563957553283));
#58870=CARTESIAN_POINT('Ctrl Pts',(11.8300359252892,-18.8655047903765,-12.1928468152564));
#58871=CARTESIAN_POINT('Ctrl Pts',(11.8290394062419,-18.8525739690576,-12.2126713034689));
#58872=CARTESIAN_POINT('Ctrl Pts',(11.8249644421306,-18.8184674171377,-12.2645448124643));
#58873=CARTESIAN_POINT('Ctrl Pts',(11.8209395722477,-18.7967229872269,-12.2972023035393));
#58874=CARTESIAN_POINT('Ctrl Pts',(11.8028867656278,-18.7307929414874,-12.3947239887608));
#58875=CARTESIAN_POINT('Ctrl Pts',(11.7841990134602,-18.6920888872388,-12.4499140109567));
#58876=CARTESIAN_POINT('Ctrl Pts',(11.7507704380579,-18.6519299935815,-12.5046623381132));
#58877=CARTESIAN_POINT('Ctrl Pts',(11.7371459986441,-18.6377168114472,-12.5236992377788));
#58878=CARTESIAN_POINT('Ctrl Pts',(11.7101248465183,-18.6209902609454,-12.5443148471325));
#58879=CARTESIAN_POINT('Ctrl Pts',(11.700195678653,-18.6160976708085,-12.5500185358362));
#58880=CARTESIAN_POINT('Ctrl Pts',(11.6812735959896,-18.6103078727442,-12.5556423476123));
#58881=CARTESIAN_POINT('Ctrl Pts',(11.6731643433662,-18.6086984664872,-12.556758771215));
#58882=CARTESIAN_POINT('Ctrl Pts',(11.6646867061662,-18.608086758819,-12.5563392961791));
#58883=CARTESIAN_POINT('Ctrl Pts',(11.6646819724071,-18.6080864175726,-12.5563390614781));
#58884=CARTESIAN_POINT('Ctrl Pts',(11.664677238709,-18.6080860766515,-12.5563388263038));
#58885=CARTESIAN_POINT('Origin',(11.6285182850279,-21.2707941051722,-13.6699093247763));
#58886=CARTESIAN_POINT('Origin',(1.06052702375292,-22.314646171184,-14.3407523135387));
#58887=CARTESIAN_POINT('Origin',(1.6653400148523,-23.0866647604201,-6.77885640724593));
#58888=CARTESIAN_POINT('',(1.95776807072638,-20.5855189702533,-6.53850782206133));
#58889=CARTESIAN_POINT('',(1.95776807072638,-20.8526247727479,-5.62882899907203));
#58890=CARTESIAN_POINT('Ctrl Pts',(1.95776807072638,-20.5855189702533,-6.53850782206133));
#58891=CARTESIAN_POINT('Ctrl Pts',(1.95134808313108,-20.5849858837543,-6.53833075322637));
#58892=CARTESIAN_POINT('Ctrl Pts',(1.94501708168414,-20.5847614100656,-6.53720798404442));
#58893=CARTESIAN_POINT('Ctrl Pts',(1.9295422670371,-20.5849190653626,-6.53223717834212));
#58894=CARTESIAN_POINT('Ctrl Pts',(1.92098940734579,-20.5856501048191,-6.52745980301533));
#58895=CARTESIAN_POINT('Ctrl Pts',(1.90083817144732,-20.5885608974204,-6.5124335905247));
#58896=CARTESIAN_POINT('Ctrl Pts',(1.89018614013605,-20.5913816029721,-6.50042022104495));
#58897=CARTESIAN_POINT('Ctrl Pts',(1.86077829278545,-20.6015952674766,-6.45943708810668));
#58898=CARTESIAN_POINT('Ctrl Pts',(1.84665745875343,-20.6111401079677,-6.42475570917512));
#58899=CARTESIAN_POINT('Ctrl Pts',(1.82247517384168,-20.6308899331561,-6.35397716492069));
#58900=CARTESIAN_POINT('Ctrl Pts',(1.81230887642857,-20.6450040326109,-6.30493959670102));
#58901=CARTESIAN_POINT('Ctrl Pts',(1.79934881945722,-20.6714274602793,-6.21380591726621));
#58902=CARTESIAN_POINT('Ctrl Pts',(1.79572382774366,-20.6848492864795,-6.16787314049738));
#58903=CARTESIAN_POINT('Ctrl Pts',(1.79301769946662,-20.7108870248801,-6.07902063441458));
#58904=CARTESIAN_POINT('Ctrl Pts',(1.79378222861456,-20.7240558919632,-6.0342124780035));
#58905=CARTESIAN_POINT('Ctrl Pts',(1.79982187672879,-20.750481671231,-5.94463801770676));
#58906=CARTESIAN_POINT('Ctrl Pts',(1.80545072973323,-20.7644003702219,-5.89763253001672));
#58907=CARTESIAN_POINT('Ctrl Pts',(1.82510992022552,-20.7940525831227,-5.79870751721765));
#58908=CARTESIAN_POINT('Ctrl Pts',(1.83960979647382,-20.8080958899708,-5.75272231988961));
#58909=CARTESIAN_POINT('Ctrl Pts',(1.86695154341724,-20.8259464835367,-5.69674419663136));
#58910=CARTESIAN_POINT('Ctrl Pts',(1.88252298601468,-20.834745760989,-5.66966644865782));
#58911=CARTESIAN_POINT('Ctrl Pts',(1.91281431352441,-20.8446460331116,-5.64327836389298));
#58912=CARTESIAN_POINT('Ctrl Pts',(1.92253441500334,-20.8472499388902,-5.63690645398558));
#58913=CARTESIAN_POINT('Ctrl Pts',(1.93813933311858,-20.8501988666454,-5.63122599523119));
#58914=CARTESIAN_POINT('Ctrl Pts',(1.94311288783717,-20.8509861372017,-5.62997943255939));
#58915=CARTESIAN_POINT('Ctrl Pts',(1.95140011049575,-20.8520210777408,-5.62892766975318));
#58916=CARTESIAN_POINT('Ctrl Pts',(1.95458052103001,-20.8523545794566,-5.6287598616123));
#58917=CARTESIAN_POINT('Ctrl Pts',(1.95776807072638,-20.8526247727479,-5.62882899907203));
#58918=CARTESIAN_POINT('',(1.65494820650842,-22.3727683628749,-9.20563530484313));
#58919=CARTESIAN_POINT('Origin',(1.65494820650842,-23.0854404918828,-6.77849692956889));
#58920=CARTESIAN_POINT('',(1.36757616935991,-22.4233810776973,-8.90802187107885));
#58921=CARTESIAN_POINT('Origin',(1.6653400148523,-22.4584609113062,-8.91832223959429));
#58922=CARTESIAN_POINT('Origin',(1.36757616935991,-23.0515849268112,-6.76855603873049));
#58923=CARTESIAN_POINT('Origin',(1.65494820650842,-23.0854404918828,-6.77849692956889));
#58924=CARTESIAN_POINT('Origin',(6.4980472271939,-23.6560104598922,-6.94603138825145));
#58925=CARTESIAN_POINT('',(11.664677238709,-21.3918572850628,-6.805215209861));
#58926=CARTESIAN_POINT('Ctrl Pts',(11.664677238709,-21.3918572850628,-6.80521520986101));
#58927=CARTESIAN_POINT('Ctrl Pts',(8.45037669575293,-21.1247507590271,-6.71721389334347));
#58928=CARTESIAN_POINT('Ctrl Pts',(5.17722936343353,-20.8528483573768,-6.62730336128236));
#58929=CARTESIAN_POINT('Ctrl Pts',(1.95776807072638,-20.5855189702533,-6.53850782206134));
#58930=CARTESIAN_POINT('',(11.3203626311916,-23.4156542242922,-9.86626896342394));
#58931=CARTESIAN_POINT('Origin',(11.3203626311916,-24.2241318908269,-7.11284689157993));
#58932=CARTESIAN_POINT('',(11.664677238709,-21.6751526289,-5.84039987251776));
#58933=CARTESIAN_POINT('Origin',(11.3203626311916,-24.2241318908269,-7.11284689157993));
#58934=CARTESIAN_POINT('Ctrl Pts',(1.95776807072638,-20.8526247727479,-5.62882899907202));
#58935=CARTESIAN_POINT('Ctrl Pts',(5.17722935754855,-21.1255230565072,-5.69865861625941));
#58936=CARTESIAN_POINT('Ctrl Pts',(8.45037668926196,-21.4028712159812,-5.77002260020613));
#58937=CARTESIAN_POINT('Ctrl Pts',(11.664677238709,-21.6751526289,-5.84039987251776));
#58938=CARTESIAN_POINT('Origin',(11.3307544395355,-24.2253561593642,-7.11320636925697));
#58939=CARTESIAN_POINT('',(11.6285182850279,-23.5364266063324,-9.58925626669053));
#58940=CARTESIAN_POINT('Origin',(11.6285182850279,-24.2604359929731,-7.1235067377724));
#58941=CARTESIAN_POINT('Origin',(11.3307544395355,-23.5013467727236,-9.5789558981751));
#58942=CARTESIAN_POINT('Ctrl Pts',(11.664677238709,-21.6751526289,-5.84039987251776));
#58943=CARTESIAN_POINT('Ctrl Pts',(11.6681756837601,-21.6754489800181,-5.84047647114824));
#58944=CARTESIAN_POINT('Ctrl Pts',(11.6716557442406,-21.6756623521126,-5.84085486706167));
#58945=CARTESIAN_POINT('Ctrl Pts',(11.6751111337893,-21.6757948999659,-5.84152480494109));
#58946=CARTESIAN_POINT('Ctrl Pts',(11.6834492137324,-21.6761147465654,-5.84314140866023));
#58947=CARTESIAN_POINT('Ctrl Pts',(11.691252831794,-21.6759503372767,-5.84637491140676));
#58948=CARTESIAN_POINT('Ctrl Pts',(11.7091239528621,-21.6747209936006,-5.85692922382957));
#58949=CARTESIAN_POINT('Ctrl Pts',(11.718489115776,-21.6732669685549,-5.86544860786683));
#58950=CARTESIAN_POINT('Ctrl Pts',(11.7423632180107,-21.6681303692968,-5.8923813682787));
#58951=CARTESIAN_POINT('Ctrl Pts',(11.7550185107735,-21.6632424395398,-5.91454378047483));
#58952=CARTESIAN_POINT('Ctrl Pts',(11.7829456066499,-21.6493229837901,-5.97457704224912));
#58953=CARTESIAN_POINT('Ctrl Pts',(11.7977324484731,-21.6371777263082,-6.02338974579431));
#58954=CARTESIAN_POINT('Ctrl Pts',(11.8194386441992,-21.6078719961959,-6.13462845786548));
#58955=CARTESIAN_POINT('Ctrl Pts',(11.825673894872,-21.5920955534046,-6.19191044279064));
#58956=CARTESIAN_POINT('Ctrl Pts',(11.8317749863308,-21.5603242616105,-6.30356890402385));
#58957=CARTESIAN_POINT('Ctrl Pts',(11.8316012176116,-21.5432716658125,-6.3615435087185));
#58958=CARTESIAN_POINT('Ctrl Pts',(11.824941361477,-21.5096050463401,-6.47243556191196));
#58959=CARTESIAN_POINT('Ctrl Pts',(11.8183083548574,-21.491887683975,-6.52901317940878));
#58960=CARTESIAN_POINT('Ctrl Pts',(11.7958216244887,-21.4564286561109,-6.63798947479533));
#58961=CARTESIAN_POINT('Ctrl Pts',(11.780565579694,-21.4404704012144,-6.68472301424738));
#58962=CARTESIAN_POINT('Ctrl Pts',(11.7536264417728,-21.4211446949063,-6.73846169515357));
#58963=CARTESIAN_POINT('Ctrl Pts',(11.7402881749122,-21.4127521672241,-6.76120915401777));
#58964=CARTESIAN_POINT('Ctrl Pts',(11.7136982696188,-21.4020408829818,-6.7873274883819));
#58965=CARTESIAN_POINT('Ctrl Pts',(11.7035133274599,-21.398679437698,-6.79496994538256));
#58966=CARTESIAN_POINT('Ctrl Pts',(11.6842762528667,-21.3943170183098,-6.80313984330739));
#58967=CARTESIAN_POINT('Ctrl Pts',(11.6760378533013,-21.3929463221456,-6.80507051068833));
#58968=CARTESIAN_POINT('Ctrl Pts',(11.6665534479108,-21.3920199943286,-6.80524520977615));
#58969=CARTESIAN_POINT('Ctrl Pts',(11.6656136423373,-21.3919350996656,-6.80524084677675));
#58970=CARTESIAN_POINT('Ctrl Pts',(11.664677238709,-21.3918572850628,-6.80521520986104));
#58971=CARTESIAN_POINT('Origin',(11.6285182850279,-24.2604359929731,-7.1235067377724));
#58972=CARTESIAN_POINT('Origin',(1.06052702375292,-25.4510030262676,-7.47308876036671));
#58973=CARTESIAN_POINT('Origin',(1.6653400148523,-24.0613171698908,2.94666150553761E-15));
#58974=CARTESIAN_POINT('',(1.95776807072638,-21.593771336803,-0.474041419794069));
#58975=CARTESIAN_POINT('',(1.79371994466189,-21.5846216014986,-2.61616378886991E-15));
#58976=CARTESIAN_POINT('Ctrl Pts',(1.95776807072638,-21.593771336803,-0.47404141979409));
#58977=CARTESIAN_POINT('Ctrl Pts',(1.95134776803084,-21.5932099304442,-0.47402171034616));
#58978=CARTESIAN_POINT('Ctrl Pts',(1.94501646548725,-21.5926782047101,-0.473007564224911));
#58979=CARTESIAN_POINT('Ctrl Pts',(1.92951932707461,-21.5914272389869,-0.468186519780772));
#58980=CARTESIAN_POINT('Ctrl Pts',(1.92094790453018,-21.5907814463351,-0.46338067495892));
#58981=CARTESIAN_POINT('Ctrl Pts',(1.9006842838642,-21.5893333422068,-0.44803695037139));
#58982=CARTESIAN_POINT('Ctrl Pts',(1.88996070920407,-21.5886516447308,-0.435581293464189));
#58983=CARTESIAN_POINT('Ctrl Pts',(1.85988430203368,-21.586868815578,-0.392217225061399));
#58984=CARTESIAN_POINT('Ctrl Pts',(1.84552319454939,-21.5862561010085,-0.354793494139702));
#58985=CARTESIAN_POINT('Ctrl Pts',(1.82174065150218,-21.5852941592389,-0.280937783834421));
#58986=CARTESIAN_POINT('Ctrl Pts',(1.81181923278629,-21.585029713215,-0.230359404107756));
#58987=CARTESIAN_POINT('Ctrl Pts',(1.799968444636,-21.5847372703622,-0.142150220758282));
#58988=CARTESIAN_POINT('Ctrl Pts',(1.79660846342292,-21.5846751446254,-0.101128548747823));
#58989=CARTESIAN_POINT('Ctrl Pts',(1.7941317217012,-21.5846288405808,-0.0406090573298228));
#58990=CARTESIAN_POINT('Ctrl Pts',(1.7937199446619,-21.5846216014986,-0.0202986714769121));
#58991=CARTESIAN_POINT('Ctrl Pts',(1.7937199446619,-21.5846216014986,-2.58897380223162E-15));
#58992=CARTESIAN_POINT('',(1.65494820650842,-24.0600412162663,-2.52960515816076));
#58993=CARTESIAN_POINT('Origin',(1.65494820650842,-24.0600412162663,3.10139888928781E-15));
#58994=CARTESIAN_POINT('',(1.36757616935991,-24.0247563668693,-2.22978791005503));
#58995=CARTESIAN_POINT('Origin',(1.6653400148523,-24.0613171698908,-2.22978791005503));
#58996=CARTESIAN_POINT('Origin',(1.36757616935991,-24.0247563668693,2.94218409849815E-15));
#58997=CARTESIAN_POINT('',(1.95776807072638,-21.593771336803,0.474041419794074));
#58998=CARTESIAN_POINT('Origin',(1.65494820650842,-24.0600412162663,3.10139888928781E-15));
#58999=CARTESIAN_POINT('Ctrl Pts',(1.7937199446619,-21.5846216014986,-2.58897380223162E-15));
#59000=CARTESIAN_POINT('Ctrl Pts',(1.7937199446619,-21.5846216014986,0.0170010253597482));
#59001=CARTESIAN_POINT('Ctrl Pts',(1.79400880365352,-21.5846267121308,0.0339938333246223));
#59002=CARTESIAN_POINT('Ctrl Pts',(1.79594647664015,-21.5846625069698,0.0907225510823662));
#59003=CARTESIAN_POINT('Ctrl Pts',(1.79895084940682,-21.5847168190493,0.131181998467417));
#59004=CARTESIAN_POINT('Ctrl Pts',(1.80977106001253,-21.5849749085674,0.218244549034728));
#59005=CARTESIAN_POINT('Ctrl Pts',(1.81886112579789,-21.5852081198308,0.267828304156));
#59006=CARTESIAN_POINT('Ctrl Pts',(1.8416420910732,-21.5860852333225,0.344658261477164));
#59007=CARTESIAN_POINT('Ctrl Pts',(1.8579971898861,-21.5867311486231,0.391115268135561));
#59008=CARTESIAN_POINT('Ctrl Pts',(1.89263444116857,-21.5888210219462,0.438752720203498));
#59009=CARTESIAN_POINT('Ctrl Pts',(1.90520057316487,-21.58962179489,0.453157912548167));
#59010=CARTESIAN_POINT('Ctrl Pts',(1.9276047246656,-21.5912873878866,0.466915949381054));
#59011=CARTESIAN_POINT('Ctrl Pts',(1.93461040386461,-21.5918315367061,0.47007865594089));
#59012=CARTESIAN_POINT('Ctrl Pts',(1.94721684080077,-21.5928636195134,0.473331332978818));
#59013=CARTESIAN_POINT('Ctrl Pts',(1.952468820417,-21.5933079578999,0.474025151823078));
#59014=CARTESIAN_POINT('Ctrl Pts',(1.95776807072638,-21.593771336803,0.474041419794074));
#59015=CARTESIAN_POINT('Origin',(6.4980472271939,-24.6546990029305,3.01932982178803E-15));
#59016=CARTESIAN_POINT('',(11.664677238709,-22.4425874385122,-0.502773529288436));
#59017=CARTESIAN_POINT('Ctrl Pts',(11.664677238709,-22.4425874385122,-0.502773529288436));
#59018=CARTESIAN_POINT('Ctrl Pts',(8.45174540654375,-22.1616274567787,-0.493593399690551));
#59019=CARTESIAN_POINT('Ctrl Pts',(5.17782841008702,-21.875340981737,-0.483926563002776));
#59020=CARTESIAN_POINT('Ctrl Pts',(1.95776807072638,-21.593771336803,-0.474041419794072));
#59021=CARTESIAN_POINT('',(11.3203626311916,-25.2468048823457,-2.86966361147139));
#59022=CARTESIAN_POINT('Origin',(11.3203626311916,-25.2468048823457,3.26755809660714E-15));
#59023=CARTESIAN_POINT('',(11.664677238709,-22.4425874385122,0.502773529288443));
#59024=CARTESIAN_POINT('Origin',(11.3203626311916,-25.2468048823457,3.26755809660714E-15));
#59025=CARTESIAN_POINT('Ctrl Pts',(1.95776807072638,-21.593771336803,0.474041419794083));
#59026=CARTESIAN_POINT('Ctrl Pts',(5.17782840427536,-21.8753409812288,0.483926562984946));
#59027=CARTESIAN_POINT('Ctrl Pts',(8.4517454000289,-22.161627456209,0.493593399671947));
#59028=CARTESIAN_POINT('Ctrl Pts',(11.664677238709,-22.4425874385122,0.502773529288447));
#59029=CARTESIAN_POINT('Origin',(11.3307544395355,-25.2480808359702,3.09199813803845E-15));
#59030=CARTESIAN_POINT('',(11.6285182850279,-25.2846416389917,-2.56984636336567));
#59031=CARTESIAN_POINT('Origin',(11.6285182850279,-25.2846416389917,3.09647554507791E-15));
#59032=CARTESIAN_POINT('Origin',(11.3307544395355,-25.2480808359702,-2.56984636336567));
#59033=CARTESIAN_POINT('',(11.8308859678787,-22.4627598424576,-2.87010257891296E-15));
#59034=CARTESIAN_POINT('Ctrl Pts',(11.8308859678787,-22.4627598424576,-2.98931046371777E-15));
#59035=CARTESIAN_POINT('Ctrl Pts',(11.8308859678787,-22.4627598424576,-0.0309229856857021));
#59036=CARTESIAN_POINT('Ctrl Pts',(11.8300161901638,-22.4626192678459,-0.0615943949967859));
#59037=CARTESIAN_POINT('Ctrl Pts',(11.825990760224,-22.4619778159673,-0.132571716988348));
#59038=CARTESIAN_POINT('Ctrl Pts',(11.8220311067205,-22.4613492475643,-0.173539728186851));
#59039=CARTESIAN_POINT('Ctrl Pts',(11.8081497193984,-22.4592328861399,-0.268683426062508));
#59040=CARTESIAN_POINT('Ctrl Pts',(11.795461589778,-22.4573293352261,-0.327557844264764));
#59041=CARTESIAN_POINT('Ctrl Pts',(11.7672407996649,-22.4535873444032,-0.403094447780781));
#59042=CARTESIAN_POINT('Ctrl Pts',(11.7555857098412,-22.4520974558946,-0.428285481038756));
#59043=CARTESIAN_POINT('Ctrl Pts',(11.7315700529649,-22.4492776427903,-0.464161175185097));
#59044=CARTESIAN_POINT('Ctrl Pts',(11.7196350773267,-22.4479351247539,-0.478241088357663));
#59045=CARTESIAN_POINT('Ctrl Pts',(11.6975720132428,-22.4456574568071,-0.494192277150503));
#59046=CARTESIAN_POINT('Ctrl Pts',(11.6885594272652,-22.4447671654469,-0.49875486063898));
#59047=CARTESIAN_POINT('Ctrl Pts',(11.6741930061584,-22.4434324790847,-0.50222507262704));
#59048=CARTESIAN_POINT('Ctrl Pts',(11.6694225684331,-22.4430024014875,-0.502787087852407));
#59049=CARTESIAN_POINT('Ctrl Pts',(11.664677238709,-22.4425874385122,-0.502773529288413));
#59050=CARTESIAN_POINT('Ctrl Pts',(11.664677238709,-22.4425874385122,0.502773529288419));
#59051=CARTESIAN_POINT('Ctrl Pts',(11.6681753033368,-22.4428933323889,0.502783524111933));
#59052=CARTESIAN_POINT('Ctrl Pts',(11.6716553635687,-22.4432046663249,0.502480637546269));
#59053=CARTESIAN_POINT('Ctrl Pts',(11.6751111337893,-22.4435206231749,0.50187511320202));
#59054=CARTESIAN_POINT('Ctrl Pts',(11.6835623119453,-22.4442933040705,0.500394287283531));
#59055=CARTESIAN_POINT('Ctrl Pts',(11.691384091347,-22.4450491314624,0.497199786883784));
#59056=CARTESIAN_POINT('Ctrl Pts',(11.7094694893507,-22.4468652011622,0.486572040199528));
#59057=CARTESIAN_POINT('Ctrl Pts',(11.7189285997145,-22.4478827563863,0.477782875801506));
#59058=CARTESIAN_POINT('Ctrl Pts',(11.7437048785722,-22.4506469894916,0.449218987208414));
#59059=CARTESIAN_POINT('Ctrl Pts',(11.756758696355,-22.4522625711256,0.425077089680007));
#59060=CARTESIAN_POINT('Ctrl Pts',(11.7862943788245,-22.4560498423181,0.357948221183704));
#59061=CARTESIAN_POINT('Ctrl Pts',(11.8016138506642,-22.4582634908384,0.301713314632811));
#59062=CARTESIAN_POINT('Ctrl Pts',(11.8195646608092,-22.4609621241242,0.195134214413126));
#59063=CARTESIAN_POINT('Ctrl Pts',(11.8242738201003,-22.4617066134238,0.151903163592283));
#59064=CARTESIAN_POINT('Ctrl Pts',(11.8295027526625,-22.46253623103,0.0759831017665234));
#59065=CARTESIAN_POINT('Ctrl Pts',(11.830683585196,-22.4627272832912,0.0420217792041652));
#59066=CARTESIAN_POINT('Ctrl Pts',(11.830878013723,-22.462758562633,0.00591621364952152));
#59067=CARTESIAN_POINT('Ctrl Pts',(11.8308859678787,-22.4627598424576,0.00295695664177951));
#59068=CARTESIAN_POINT('Ctrl Pts',(11.8308859678787,-22.4627598424576,-2.98931046371777E-15));
#59069=CARTESIAN_POINT('Origin',(11.6285182850279,-25.2846416389917,3.09647554507791E-15));
#59070=CARTESIAN_POINT('Origin',(1.06052702375292,-26.5254709791062,3.24843331304384E-15));
#59071=CARTESIAN_POINT('Origin',(1.6653400148523,-23.0866647604201,6.77885640724594));
#59072=CARTESIAN_POINT('',(1.95776807072638,-20.8526247727479,5.62882899907204));
#59073=CARTESIAN_POINT('',(1.95776807072638,-20.5855189702533,6.53850782206133));
#59074=CARTESIAN_POINT('Ctrl Pts',(1.95776807072638,-20.8526247727479,5.62882899907204));
#59075=CARTESIAN_POINT('Ctrl Pts',(1.95134808328295,-20.8520805812205,5.62868975053771));
#59076=CARTESIAN_POINT('Ctrl Pts',(1.94501708192101,-20.8512847271148,5.62951292437162));
#59077=CARTESIAN_POINT('Ctrl Pts',(1.92954226703916,-20.8487299346933,5.63377986718257));
#59078=CARTESIAN_POINT('Ctrl Pts',(1.92098940734792,-20.846762080117,5.63819408082297));
#59079=CARTESIAN_POINT('Ctrl Pts',(1.90083817144993,-20.8410870108723,5.65240862845604));
#59080=CARTESIAN_POINT('Ctrl Pts',(1.89018614013894,-20.8369650214871,5.66403990652636));
#59081=CARTESIAN_POINT('Ctrl Pts',(1.86077829278984,-20.8234001483423,5.70403903581996));
#59082=CARTESIAN_POINT('Ctrl Pts',(1.8466574587581,-20.8126796100708,5.7383751987311));
#59083=CARTESIAN_POINT('Ctrl Pts',(1.82247517384463,-20.7910284502593,5.8085954607679));
#59084=CARTESIAN_POINT('Ctrl Pts',(1.81230887643079,-20.77639027532,5.8574791465412));
#59085=CARTESIAN_POINT('Ctrl Pts',(1.79934881945839,-20.7493484902482,5.94843125986021));
#59086=CARTESIAN_POINT('Ctrl Pts',(1.79572382774438,-20.7358065149758,5.99432875767835));
#59087=CARTESIAN_POINT('Ctrl Pts',(1.79301769946659,-20.7096735628705,6.08315330649572));
#59088=CARTESIAN_POINT('Ctrl Pts',(1.7937822286142,-20.6965268005168,6.12796795344078));
#59089=CARTESIAN_POINT('Ctrl Pts',(1.7998218767276,-20.6703299712458,6.21760963952165));
#59090=CARTESIAN_POINT('Ctrl Pts',(1.80545072973152,-20.6566260406547,6.2646781889035));
#59091=CARTESIAN_POINT('Ctrl Pts',(1.82510992022243,-20.6280881697271,6.36393040202843));
#59092=CARTESIAN_POINT('Ctrl Pts',(1.83960979646987,-20.6150406765513,6.410207996633));
#59093=CARTESIAN_POINT('Ctrl Pts',(1.86695154341405,-20.5997934931318,6.46695055008921));
#59094=CARTESIAN_POINT('Ctrl Pts',(1.88252298601552,-20.5925565805734,6.49448704979649));
#59095=CARTESIAN_POINT('Ctrl Pts',(1.91281431353043,-20.5866187437543,6.52203861054359));
#59096=CARTESIAN_POINT('Ctrl Pts',(1.922534415008,-20.5853643741092,6.5288067800109));
#59097=CARTESIAN_POINT('Ctrl Pts',(1.9381393331208,-20.5847740821371,6.53517979671659));
#59098=CARTESIAN_POINT('Ctrl Pts',(1.94311288783888,-20.5847624336121,6.53665410256502));
#59099=CARTESIAN_POINT('Ctrl Pts',(1.95140011070329,-20.5850644551011,6.53809843287623));
#59100=CARTESIAN_POINT('Ctrl Pts',(1.95458052118134,-20.5852542906722,6.53841990667583));
#59101=CARTESIAN_POINT('Ctrl Pts',(1.95776807072638,-20.5855189702533,6.53850782206133));
#59102=CARTESIAN_POINT('',(1.65494820650842,-23.7981126208907,4.35135855429466));
#59103=CARTESIAN_POINT('Origin',(1.65494820650842,-23.0854404918828,6.7784969295689));
#59104=CARTESIAN_POINT('',(1.36757616935991,-23.6797887759252,4.62909020638214));
#59105=CARTESIAN_POINT('Origin',(1.6653400148523,-23.714868609534,4.63939057489758));
#59106=CARTESIAN_POINT('Origin',(1.36757616935991,-23.0515849268112,6.7685560387305));
#59107=CARTESIAN_POINT('Origin',(1.65494820650842,-23.0854404918828,6.7784969295689));
#59108=CARTESIAN_POINT('Origin',(6.4980472271939,-23.6560104598922,6.94603138825146));
#59109=CARTESIAN_POINT('',(11.664677238709,-21.6751526289,5.84039987251778));
#59110=CARTESIAN_POINT('Ctrl Pts',(11.664677238709,-21.6751526289,5.84039987251777));
#59111=CARTESIAN_POINT('Ctrl Pts',(8.45037669575292,-21.402871216531,5.77002260034827));
#59112=CARTESIAN_POINT('Ctrl Pts',(5.17722936343352,-21.1255230570061,5.69865861638707));
#59113=CARTESIAN_POINT('Ctrl Pts',(1.95776807072638,-20.8526247727479,5.62882899907203));
#59114=CARTESIAN_POINT('',(11.3203626311916,-25.0326095573615,4.35942481973593));
#59115=CARTESIAN_POINT('Origin',(11.3203626311916,-24.2241318908269,7.11284689157994));
#59116=CARTESIAN_POINT('',(11.664677238709,-21.3918572850628,6.805215209861));
#59117=CARTESIAN_POINT('Origin',(11.3203626311916,-24.2241318908269,7.11284689157994));
#59118=CARTESIAN_POINT('Ctrl Pts',(1.95776807072638,-20.5855189702533,6.53850782206134));
#59119=CARTESIAN_POINT('Ctrl Pts',(5.17722935754855,-20.8528483568881,6.62730336112004));
#59120=CARTESIAN_POINT('Ctrl Pts',(8.45037668926196,-21.1247507584877,6.71721389316576));
#59121=CARTESIAN_POINT('Ctrl Pts',(11.664677238709,-21.3918572850628,6.805215209861));
#59122=CARTESIAN_POINT('Origin',(11.3307544395355,-24.2253561593642,7.11320636925698));
#59123=CARTESIAN_POINT('',(11.6285182850279,-24.9844453796138,4.65775720885429));
#59124=CARTESIAN_POINT('Origin',(11.6285182850279,-24.2604359929731,7.12350673777241));
#59125=CARTESIAN_POINT('Origin',(11.3307544395355,-24.9493655460049,4.64745684033885));
#59126=CARTESIAN_POINT('Ctrl Pts',(11.664677238709,-21.3918572850628,6.805215209861));
#59127=CARTESIAN_POINT('Ctrl Pts',(11.6681756837601,-21.392148003834,6.80531099050321));
#59128=CARTESIAN_POINT('Ctrl Pts',(11.6716557442406,-21.3925320801382,6.80510802126781));
#59129=CARTESIAN_POINT('Ctrl Pts',(11.6751111337893,-21.3930057822509,6.80461609443974));
#59130=CARTESIAN_POINT('Ctrl Pts',(11.6834492137325,-21.394148856289,6.80342904297686));
#59131=CARTESIAN_POINT('Ctrl Pts',(11.6912528317941,-21.3957587099622,6.80061996099559));
#59132=CARTESIAN_POINT('Ctrl Pts',(11.709123952862,-21.4004306123475,6.79107647501339));
#59133=CARTESIAN_POINT('Ctrl Pts',(11.7184891157759,-21.403813335391,6.78312340780531));
#59134=CARTESIAN_POINT('Ctrl Pts',(11.7423632180108,-21.4140531027239,6.75768907273794));
#59135=CARTESIAN_POINT('Ctrl Pts',(11.7550185107736,-21.4219230191941,6.73640225084234));
#59136=CARTESIAN_POINT('Ctrl Pts',(11.7829456066499,-21.4426696595898,6.6783736313523));
#59137=CARTESIAN_POINT('Ctrl Pts',(11.7977324484731,-21.4588425587729,6.63074355011461));
#59138=CARTESIAN_POINT('Ctrl Pts',(11.8194386441992,-21.4943291980106,6.52131971671298));
#59139=CARTESIAN_POINT('Ctrl Pts',(11.825673894872,-21.5120261889324,6.46460165559978));
#59140=CARTESIAN_POINT('Ctrl Pts',(11.8317749863308,-21.5456655992248,6.35349172344992));
#59141=CARTESIAN_POINT('Ctrl Pts',(11.8316012176116,-21.5626634804396,6.29550105310408));
#59142=CARTESIAN_POINT('Ctrl Pts',(11.824941361477,-21.5942940881578,6.18401117291958));
#59143=CARTESIAN_POINT('Ctrl Pts',(11.8183083548574,-21.6099774638489,6.12683632304897));
#59144=CARTESIAN_POINT('Ctrl Pts',(11.795821624489,-21.6390644648082,6.01598903175088));
#59145=CARTESIAN_POINT('Ctrl Pts',(11.7805655796943,-21.6509055854708,5.96804659261232));
#59146=CARTESIAN_POINT('Ctrl Pts',(11.7536264417728,-21.6637010911389,5.91239047179329));
#59147=CARTESIAN_POINT('Ctrl Pts',(11.7402881749122,-21.6689390523323,5.88871674863418));
#59148=CARTESIAN_POINT('Ctrl Pts',(11.7136982696187,-21.6740487842635,5.86095365010984));
#59149=CARTESIAN_POINT('Ctrl Pts',(11.7035133274599,-21.6753527807432,5.85270707163255));
#59150=CARTESIAN_POINT('Ctrl Pts',(11.6842762528667,-21.6760998603139,5.84347561415638));
#59151=CARTESIAN_POINT('Ctrl Pts',(11.6760378533013,-21.6759905549143,5.84111037910665));
#59152=CARTESIAN_POINT('Ctrl Pts',(11.6665534479108,-21.6753057278234,5.84046260225363));
#59153=CARTESIAN_POINT('Ctrl Pts',(11.6656136423373,-21.6752319510726,5.84042037512235));
#59154=CARTESIAN_POINT('Ctrl Pts',(11.664677238709,-21.6751526289,5.84039987251778));
#59155=CARTESIAN_POINT('Origin',(11.6285182850279,-24.2604359929731,7.12350673777241));
#59156=CARTESIAN_POINT('Origin',(1.06052702375292,-25.4510030262676,7.47308876036672));
#59157=CARTESIAN_POINT('Origin',(1.6653400148523,-20.2416680737422,13.0085301837882));
#59158=CARTESIAN_POINT('',(1.95776807072638,-18.4221225649395,11.2756851683684));
#59159=CARTESIAN_POINT('',(1.95776807072638,-17.9095502835289,12.0732632065885));
#59160=CARTESIAN_POINT('Ctrl Pts',(1.95776807072638,-18.4221225649395,11.2756851683684));
#59161=CARTESIAN_POINT('Ctrl Pts',(1.95134736183191,-18.4216395935701,11.2753982116643));
#59162=CARTESIAN_POINT('Ctrl Pts',(1.94501567125517,-18.4206438937256,11.2759639830883));
#59163=CARTESIAN_POINT('Ctrl Pts',(1.92948836979317,-18.4169777842864,11.2793502116274));
#59164=CARTESIAN_POINT('Ctrl Pts',(1.9208918623398,-18.4138230903949,11.2830613241242));
#59165=CARTESIAN_POINT('Ctrl Pts',(1.90046800930186,-18.4042191176333,11.2953067736052));
#59166=CARTESIAN_POINT('Ctrl Pts',(1.88964186308612,-18.3968030080762,11.3055760598059));
#59167=CARTESIAN_POINT('Ctrl Pts',(1.85810283833502,-18.3704851710237,11.3430782725479));
#59168=CARTESIAN_POINT('Ctrl Pts',(1.8433562930371,-18.3481042542488,11.3767845480151));
#59169=CARTESIAN_POINT('Ctrl Pts',(1.81854010589205,-18.304034165225,11.4435429822473));
#59170=CARTESIAN_POINT('Ctrl Pts',(1.8083691782649,-18.2726985595794,11.4918522175932));
#59171=CARTESIAN_POINT('Ctrl Pts',(1.79896764765296,-18.2274018269571,11.5619364610537));
#59172=CARTESIAN_POINT('Ctrl Pts',(1.79670145400061,-18.2114630036213,11.5866568740703));
#59173=CARTESIAN_POINT('Ctrl Pts',(1.79434535609113,-18.1842435918483,11.6289286489356));
#59174=CARTESIAN_POINT('Ctrl Pts',(1.79381557303812,-18.1727761179962,11.6467551189356));
#59175=CARTESIAN_POINT('Ctrl Pts',(1.79365032105971,-18.1502654058706,11.6817769814635));
#59176=CARTESIAN_POINT('Ctrl Pts',(1.79398945985934,-18.1391347052042,11.6991076651001));
#59177=CARTESIAN_POINT('Ctrl Pts',(1.79575501944578,-18.1136547229072,11.7388159539009));
#59178=CARTESIAN_POINT('Ctrl Pts',(1.79749007695648,-18.0991705776079,11.7614139961321));
#59179=CARTESIAN_POINT('Ctrl Pts',(1.80455267776983,-18.0593401605001,11.8236744660528));
#59180=CARTESIAN_POINT('Ctrl Pts',(1.81186451913785,-18.0330203540242,11.8649367864125));
#59181=CARTESIAN_POINT('Ctrl Pts',(1.8357835522891,-17.9799323185448,11.9490437490344));
#59182=CARTESIAN_POINT('Ctrl Pts',(1.85214505346243,-17.957095277983,11.9858397344708));
#59183=CARTESIAN_POINT('Ctrl Pts',(1.88061329933065,-17.9321806919618,12.027521920884));
#59184=CARTESIAN_POINT('Ctrl Pts',(1.89448595076313,-17.9221533057532,12.0446318207664));
#59185=CARTESIAN_POINT('Ctrl Pts',(1.92022261571912,-17.9130069990607,12.0622553637802));
#59186=CARTESIAN_POINT('Ctrl Pts',(1.92864558703565,-17.91092340545,12.0666669158279));
#59187=CARTESIAN_POINT('Ctrl Pts',(1.94192278721254,-17.9094652452642,12.0709092294435));
#59188=CARTESIAN_POINT('Ctrl Pts',(1.94616291414725,-17.9092382087298,12.0719097149397));
#59189=CARTESIAN_POINT('Ctrl Pts',(1.95291207286072,-17.9092807395709,12.0729030082265));
#59190=CARTESIAN_POINT('Ctrl Pts',(1.95533909578542,-17.9093756366037,12.073142104124));
#59191=CARTESIAN_POINT('Ctrl Pts',(1.95776807072638,-17.9095502835289,12.0732632065885));
#59192=CARTESIAN_POINT('',(1.65494820650842,-21.6082024737958,10.8798010752069));
#59193=CARTESIAN_POINT('Origin',(1.65494820650842,-20.2405946732479,13.0078403511776));
#59194=CARTESIAN_POINT('',(1.36757616935991,-21.416425527482,11.1129469645577));
#59195=CARTESIAN_POINT('Origin',(1.6653400148523,-21.447182432187,11.1327132269901));
#59196=CARTESIAN_POINT('Origin',(1.36757616935991,-20.2109111690372,12.9887639213558));
#59197=CARTESIAN_POINT('Origin',(1.65494820650842,-20.2405946732479,13.0078403511776));
#59198=CARTESIAN_POINT('Origin',(6.4980472271939,-20.7408526371047,13.3293366230661));
#59199=CARTESIAN_POINT('',(11.664677238709,-19.1517258603906,11.7104188108481));
#59200=CARTESIAN_POINT('Ctrl Pts',(11.664677238709,-19.1517258603906,11.7104188108481));
#59201=CARTESIAN_POINT('Ctrl Pts',(8.44760841234032,-18.9100934028027,11.566057551542));
#59202=CARTESIAN_POINT('Ctrl Pts',(5.17558411912346,-18.6641695178434,11.4194969970449));
#59203=CARTESIAN_POINT('Ctrl Pts',(1.95776807072638,-18.4221225649395,11.2756851683684));
#59204=CARTESIAN_POINT('',(11.3203626311916,-22.7904210807013,11.2353385785459));
#59205=CARTESIAN_POINT('Origin',(11.3203626311916,-21.2389637999728,13.6494532297333));
#59206=CARTESIAN_POINT('',(11.664677238709,-18.6080860766515,12.5563388263039));
#59207=CARTESIAN_POINT('Origin',(11.3203626311916,-21.2389637999728,13.6494532297333));
#59208=CARTESIAN_POINT('Ctrl Pts',(1.95776807072638,-17.9095502835289,12.0732632065885));
#59209=CARTESIAN_POINT('Ctrl Pts',(5.17558411308691,-18.1409160618572,12.2336952663475));
#59210=CARTESIAN_POINT('Ctrl Pts',(8.44760840593807,-18.3763927053254,12.3965120458593));
#59211=CARTESIAN_POINT('Ctrl Pts',(11.664677238709,-18.6080860766515,12.5563388263038));
#59212=CARTESIAN_POINT('Origin',(11.3307544395355,-21.2400372004671,13.6501430623439));
#59213=CARTESIAN_POINT('',(11.6285182850279,-22.6601579437975,11.5080169927616));
#59214=CARTESIAN_POINT('Origin',(11.6285182850279,-21.2707941051722,13.6699093247763));
#59215=CARTESIAN_POINT('Origin',(11.3307544395355,-22.6294010390924,11.4882507303292));
#59216=CARTESIAN_POINT('Ctrl Pts',(11.664677238709,-18.6080860766515,12.5563388263039));
#59217=CARTESIAN_POINT('Ctrl Pts',(11.6681719057553,-18.6083377626526,12.5565124444052));
#59218=CARTESIAN_POINT('Ctrl Pts',(11.6716519636861,-18.6087630873824,12.5564264617449));
#59219=CARTESIAN_POINT('Ctrl Pts',(11.6751111337893,-18.6093568419532,12.5560875483161));
#59220=CARTESIAN_POINT('Ctrl Pts',(11.6833639439589,-18.6107734082434,12.5552789762861));
#59221=CARTESIAN_POINT('Ctrl Pts',(11.6912209922801,-18.6131029323726,12.5530553109812));
#59222=CARTESIAN_POINT('Ctrl Pts',(11.7092716451021,-18.6203670705107,12.5451050615273));
#59223=CARTESIAN_POINT('Ctrl Pts',(11.7188321121789,-18.6259692752841,12.5382858333101));
#59224=CARTESIAN_POINT('Ctrl Pts',(11.7448362096952,-18.6446600490307,12.5145712192167));
#59225=CARTESIAN_POINT('Ctrl Pts',(11.7582763496126,-18.6601414182568,12.4935901023805));
#59226=CARTESIAN_POINT('Ctrl Pts',(11.7901173768953,-18.7031288181134,12.4342691481542));
#59227=CARTESIAN_POINT('Ctrl Pts',(11.8074969006879,-18.7427730168715,12.3773456251793));
#59228=CARTESIAN_POINT('Ctrl Pts',(11.8229354401012,-18.807249025111,12.2814049176088));
#59229=CARTESIAN_POINT('Ctrl Pts',(11.826199199177,-18.8268628597469,12.2518426658347));
#59230=CARTESIAN_POINT('Ctrl Pts',(11.8295237141305,-18.8585151047524,12.2035704025212));
#59231=CARTESIAN_POINT('Ctrl Pts',(11.8303434615844,-18.8708529717768,12.1846162306134));
#59232=CARTESIAN_POINT('Ctrl Pts',(11.8309946485842,-18.893887321558,12.1489677324934));
#59233=CARTESIAN_POINT('Ctrl Pts',(11.8309459330901,-18.9046640233566,12.1321843072664));
#59234=CARTESIAN_POINT('Ctrl Pts',(11.8300359252892,-18.9280174953953,12.0955751475504));
#59235=CARTESIAN_POINT('Ctrl Pts',(11.8290394062419,-18.9406788268584,12.0755774687241));
#59236=CARTESIAN_POINT('Ctrl Pts',(11.8249644421306,-18.9736962566426,12.023004023433));
#59237=CARTESIAN_POINT('Ctrl Pts',(11.8209395722477,-18.9943695927783,11.9896581821858));
#59238=CARTESIAN_POINT('Ctrl Pts',(11.8028867656276,-19.055690107089,11.8891741309911));
#59239=CARTESIAN_POINT('Ctrl Pts',(11.7841990134599,-19.0898144719036,11.8310409211087));
#59240=CARTESIAN_POINT('Ctrl Pts',(11.7507704380578,-19.1229326946464,11.7717678295026));
#59241=CARTESIAN_POINT('Ctrl Pts',(11.737145998644,-19.1343448984334,11.7509308503555));
#59242=CARTESIAN_POINT('Ctrl Pts',(11.7101248465183,-19.1461490561111,11.7271518112195));
#59243=CARTESIAN_POINT('Ctrl Pts',(11.700195678653,-19.1493048584522,11.7203319567739));
#59244=CARTESIAN_POINT('Ctrl Pts',(11.6812735959897,-19.1520152885414,11.7127291553659));
#59245=CARTESIAN_POINT('Ctrl Pts',(11.6731643433663,-19.1523622516496,11.7108014088155));
#59246=CARTESIAN_POINT('Ctrl Pts',(11.6646867061662,-19.1517265711868,11.7104192361762));
#59247=CARTESIAN_POINT('Ctrl Pts',(11.6646819724071,-19.1517262159363,11.7104190232658));
#59248=CARTESIAN_POINT('Ctrl Pts',(11.664677238709,-19.1517258603906,11.7104188108481));
#59249=CARTESIAN_POINT('Origin',(11.6285182850279,-21.2707941051722,13.6699093247763));
#59250=CARTESIAN_POINT('Origin',(1.06052702375292,-22.314646171184,14.3407523135387));
#59251=CARTESIAN_POINT('Origin',(1.6653400148523,-15.756811821565,18.1843302095478));
#59252=CARTESIAN_POINT('',(1.95776807072638,-14.4991695475011,16.0090523844052));
#59253=CARTESIAN_POINT('',(1.95776807072638,-13.7826563450298,16.6299146085789));
#59254=CARTESIAN_POINT('Ctrl Pts',(1.95776807072638,-14.4991695475011,16.0090523844052));
#59255=CARTESIAN_POINT('Ctrl Pts',(1.95134736178518,-14.4987869849089,16.0086409827022));
#59256=CARTESIAN_POINT('Ctrl Pts',(1.94501567118224,-14.4976722216562,16.0089033153585));
#59257=CARTESIAN_POINT('Ctrl Pts',(1.92948836979211,-14.493200604605,16.0111195154527));
#59258=CARTESIAN_POINT('Ctrl Pts',(1.9208918623387,-14.4891281567696,16.0137915218418));
#59259=CARTESIAN_POINT('Ctrl Pts',(1.90046800930049,-14.4764632705936,16.0228351927759));
#59260=CARTESIAN_POINT('Ctrl Pts',(1.8896418630846,-14.4664543733233,16.0305991412226));
#59261=CARTESIAN_POINT('Ctrl Pts',(1.85810283833289,-14.4306369993061,16.0591676593216));
#59262=CARTESIAN_POINT('Ctrl Pts',(1.84335629303482,-14.3996665117469,16.085203160893));
#59263=CARTESIAN_POINT('Ctrl Pts',(1.81854010589082,-14.338573546615,16.1368414306076));
#59264=CARTESIAN_POINT('Ctrl Pts',(1.80836917826421,-14.2948969687822,16.1743655421829));
#59265=CARTESIAN_POINT('Ctrl Pts',(1.7989676476527,-14.2316900590003,16.2288493170451));
#59266=CARTESIAN_POINT('Ctrl Pts',(1.79670145400044,-14.2094323248369,16.2480778941875));
#59267=CARTESIAN_POINT('Ctrl Pts',(1.79434535609105,-14.1714061552799,16.2809687706783));
#59268=CARTESIAN_POINT('Ctrl Pts',(1.79381557303809,-14.1553808977212,16.2948423826588));
#59269=CARTESIAN_POINT('Ctrl Pts',(1.79365032105973,-14.123915228731,16.3221036131932));
#59270=CARTESIAN_POINT('Ctrl Pts',(1.79398945985937,-14.1083527818371,16.3355964016126));
#59271=CARTESIAN_POINT('Ctrl Pts',(1.79575501944591,-14.0727178001231,16.3665176851508));
#59272=CARTESIAN_POINT('Ctrl Pts',(1.79749007695668,-14.052453760262,16.3841196926005));
#59273=CARTESIAN_POINT('Ctrl Pts',(1.80455267777036,-13.996695953529,16.4326366507725));
#59274=CARTESIAN_POINT('Ctrl Pts',(1.81186451913875,-13.9598173451314,16.4648124108593));
#59275=CARTESIAN_POINT('Ctrl Pts',(1.8357835522914,-13.8851840784767,16.5305558225553));
#59276=CARTESIAN_POINT('Ctrl Pts',(1.85214505346569,-13.852905471461,16.5594273742107));
#59277=CARTESIAN_POINT('Ctrl Pts',(1.88061329933481,-13.8172568722815,16.5924018891755));
#59278=CARTESIAN_POINT('Ctrl Pts',(1.89448595076677,-13.8028152498312,16.6059936767355));
#59279=CARTESIAN_POINT('Ctrl Pts',(1.9202226157215,-13.7890743069931,16.6203265300558));
#59280=CARTESIAN_POINT('Ctrl Pts',(1.92864558703758,-13.7858322357261,16.6239723670925));
#59281=CARTESIAN_POINT('Ctrl Pts',(1.94192278721349,-13.783237943412,16.6276320260006));
#59282=CARTESIAN_POINT('Ctrl Pts',(1.94616291414808,-13.7827382341156,16.6285280212211));
#59283=CARTESIAN_POINT('Ctrl Pts',(1.95291207283927,-13.7824991991022,16.6294930614699));
#59284=CARTESIAN_POINT('Ctrl Pts',(1.9553390957689,-13.7825228910382,16.6297492078892));
#59285=CARTESIAN_POINT('Ctrl Pts',(1.95776807072638,-13.7826563450298,16.6299146085789));
#59286=CARTESIAN_POINT('',(1.65494820650842,-17.6677242712023,16.5268268176743));
#59287=CARTESIAN_POINT('Origin',(1.65494820650842,-15.755976249638,18.1833659081392));
#59288=CARTESIAN_POINT('',(1.36757616935991,-17.418030851189,16.6964988509053));
#59289=CARTESIAN_POINT('Origin',(1.6653400148523,-17.4419730854894,16.7241296622268));
#59290=CARTESIAN_POINT('Origin',(1.36757616935991,-15.7328695872647,18.1566993982262));
#59291=CARTESIAN_POINT('Origin',(1.65494820650842,-15.755976249638,18.1833659081392));
#59292=CARTESIAN_POINT('Origin',(6.4980472271939,-16.1453942842592,18.6327782772971));
#59293=CARTESIAN_POINT('',(11.664677238709,-15.0767401623716,16.6317292616657));
#59294=CARTESIAN_POINT('Ctrl Pts',(11.664677238709,-15.0767401623716,16.6317292616657));
#59295=CARTESIAN_POINT('Ctrl Pts',(8.44646649976651,-14.8854989259897,16.425066587821));
#59296=CARTESIAN_POINT('Ctrl Pts',(5.17487115867276,-14.6908529438561,16.2151856480993));
#59297=CARTESIAN_POINT('Ctrl Pts',(1.95776807072638,-14.4991695475011,16.0090523844052));
#59298=CARTESIAN_POINT('',(11.3203626311916,-18.7018882279357,17.2010320248535));
#59299=CARTESIAN_POINT('Origin',(11.3203626311916,-16.5331411750263,19.0802620436378));
#59300=CARTESIAN_POINT('',(11.664677238709,-14.316798400859,17.2902225464619));
#59301=CARTESIAN_POINT('Origin',(11.3203626311916,-16.5331411750263,19.0802620436378));
#59302=CARTESIAN_POINT('Ctrl Pts',(1.95776807072638,-13.7826563450298,16.6299146085789));
#59303=CARTESIAN_POINT('Ctrl Pts',(5.17487115257265,-13.959412077432,16.8489827660136));
#59304=CARTESIAN_POINT('Ctrl Pts',(8.44646649340719,-14.1394557203275,17.0715167046817));
#59305=CARTESIAN_POINT('Ctrl Pts',(11.664677238709,-14.316798400859,17.2902225464619));
#59306=CARTESIAN_POINT('Origin',(11.3307544395355,-16.5339767469533,19.0812263450464));
#59307=CARTESIAN_POINT('',(11.6285182850279,-18.5000792765231,17.4259656807277));
#59308=CARTESIAN_POINT('Origin',(11.6285182850279,-16.5579189812536,19.1088571563679));
#59309=CARTESIAN_POINT('Origin',(11.3307544395355,-18.4761370422228,17.3983348694061));
#59310=CARTESIAN_POINT('Ctrl Pts',(11.664677238709,-14.316798400859,17.2902225464619));
#59311=CARTESIAN_POINT('Ctrl Pts',(11.6681719057554,-14.316990977937,17.2904600399508));
#59312=CARTESIAN_POINT('Ctrl Pts',(11.6716519636863,-14.3174232981415,17.2904973680161));
#59313=CARTESIAN_POINT('Ctrl Pts',(11.6751111337893,-14.318088484427,17.2903394629558));
#59314=CARTESIAN_POINT('Ctrl Pts',(11.6833639439589,-14.3196754708945,17.2899627366173));
#59315=CARTESIAN_POINT('Ctrl Pts',(11.6912209922801,-14.3225371118403,17.2884854481707));
#59316=CARTESIAN_POINT('Ctrl Pts',(11.7092716451021,-14.3317468454494,17.282903783892));
#59317=CARTESIAN_POINT('Ctrl Pts',(11.7188321121789,-14.3390433201674,17.2779391058069));
#59318=CARTESIAN_POINT('Ctrl Pts',(11.744836209695,-14.3636581651116,17.2604508996895));
#59319=CARTESIAN_POINT('Ctrl Pts',(11.7582763496125,-14.3844234937974,17.2446812712422));
#59320=CARTESIAN_POINT('Ctrl Pts',(11.7901173768953,-14.4423822460226,17.1998741825471));
#59321=CARTESIAN_POINT('Ctrl Pts',(11.8074969006879,-14.4964577858478,17.1564255236994));
#59322=CARTESIAN_POINT('Ctrl Pts',(11.8229354401012,-14.5853516835692,17.0825360795582));
#59323=CARTESIAN_POINT('Ctrl Pts',(11.826199199177,-14.6124996688663,17.0596971624782));
#59324=CARTESIAN_POINT('Ctrl Pts',(11.8295237141305,-14.6564696437161,17.0222977329235));
#59325=CARTESIAN_POINT('Ctrl Pts',(11.8303434615844,-14.6736477477498,17.00758731698));
#59326=CARTESIAN_POINT('Ctrl Pts',(11.8309946485842,-14.7057923870393,16.9798723597733));
#59327=CARTESIAN_POINT('Ctrl Pts',(11.8309459330901,-14.7208609939957,16.9668049289467));
#59328=CARTESIAN_POINT('Ctrl Pts',(11.8300359252892,-14.753582478497,16.9382581308177));
#59329=CARTESIAN_POINT('Ctrl Pts',(11.8290394062419,-14.7713649342591,16.9226376077815));
#59330=CARTESIAN_POINT('Ctrl Pts',(11.8249644421306,-14.8178565773075,16.8814958413395));
#59331=CARTESIAN_POINT('Ctrl Pts',(11.8209395722478,-14.8470871071856,16.8553250928115));
#59332=CARTESIAN_POINT('Ctrl Pts',(11.8028867656276,-14.9342333384702,16.7761873370133));
#59333=CARTESIAN_POINT('Ctrl Pts',(11.7841990134599,-14.9833534445964,16.7300228751473));
#59334=CARTESIAN_POINT('Ctrl Pts',(11.7507704380578,-15.0318293062667,16.6824812417983));
#59335=CARTESIAN_POINT('Ctrl Pts',(11.7371459986441,-15.0486496910257,16.6657034960674));
#59336=CARTESIAN_POINT('Ctrl Pts',(11.7101248465184,-15.0666750268719,16.646213290621));
#59337=CARTESIAN_POINT('Ctrl Pts',(11.700195678653,-15.0716243720746,16.6405587804617));
#59338=CARTESIAN_POINT('Ctrl Pts',(11.6812735959896,-15.0763669673805,16.6340275623301));
#59339=CARTESIAN_POINT('Ctrl Pts',(11.6731643433662,-15.0772429850095,16.6322756538638));
#59340=CARTESIAN_POINT('Ctrl Pts',(11.6646867061662,-15.0767407245468,16.6317298700195));
#59341=CARTESIAN_POINT('Ctrl Pts',(11.6646819724071,-15.0767404436703,16.6317295656479));
#59342=CARTESIAN_POINT('Ctrl Pts',(11.664677238709,-15.0767401623716,16.6317292616657));
#59343=CARTESIAN_POINT('Origin',(11.6285182850279,-16.5579189812536,19.1088571563679));
#59344=CARTESIAN_POINT('Origin',(1.06052702375292,-17.3704893936218,20.0466134020057));
#59345=CARTESIAN_POINT('Origin',(1.6653400148523,-9.99543238497271,21.8869439481057));
#59346=CARTESIAN_POINT('',(1.95776807072638,-9.40158004320575,19.4454613857581));
#59347=CARTESIAN_POINT('',(1.95776807072638,-8.5391735580698,19.8393092308925));
#59348=CARTESIAN_POINT('Ctrl Pts',(1.95776807072638,-9.40158004320576,19.4454613857581));
#59349=CARTESIAN_POINT('Ctrl Pts',(1.95134736181189,-9.40132888234126,19.4449588683795));
#59350=CARTESIAN_POINT('Ctrl Pts',(1.94501567122392,-9.40018536719516,19.4448965096142));
#59351=CARTESIAN_POINT('Ctrl Pts',(1.92948836979269,-9.39527050632193,19.4457631379299));
#59352=CARTESIAN_POINT('Ctrl Pts',(1.92089186233927,-9.39061023004665,19.4471795681443));
#59353=CARTESIAN_POINT('Ctrl Pts',(1.90046800930126,-9.37591046421397,19.4522887960967));
#59354=CARTESIAN_POINT('Ctrl Pts',(1.88964186308544,-9.36411964056273,19.4569184178596));
#59355=CARTESIAN_POINT('Ctrl Pts',(1.85810283833409,-9.32170444021175,19.4742387898804));
#59356=CARTESIAN_POINT('Ctrl Pts',(1.8433562930361,-9.28465342658408,19.4904942760555));
#59357=CARTESIAN_POINT('Ctrl Pts',(1.81854010589152,-9.21148697404528,19.5228289557446));
#59358=CARTESIAN_POINT('Ctrl Pts',(1.80836917826461,-9.15900784060505,19.5465279631957));
#59359=CARTESIAN_POINT('Ctrl Pts',(1.79896764765285,-9.08301140158625,19.5809973180493));
#59360=CARTESIAN_POINT('Ctrl Pts',(1.79670145400053,-9.05623794584491,19.5931762743549));
#59361=CARTESIAN_POINT('Ctrl Pts',(1.79434535609109,-9.01048567261076,19.6140216292678));
#59362=CARTESIAN_POINT('Ctrl Pts',(1.7938155730381,-8.99120090240678,19.6228184256957));
#59363=CARTESIAN_POINT('Ctrl Pts',(1.79365032105972,-8.9533294379193,19.6401104814683));
#59364=CARTESIAN_POINT('Ctrl Pts',(1.79398945985935,-8.93459602169225,19.6486722691969));
#59365=CARTESIAN_POINT('Ctrl Pts',(1.79575501944583,-8.8916929748512,19.6683014889756));
#59366=CARTESIAN_POINT('Ctrl Pts',(1.79749007695656,-8.86729071242315,19.679481451683));
#59367=CARTESIAN_POINT('Ctrl Pts',(1.80455267777006,-8.80012268196332,19.7103243426951));
#59368=CARTESIAN_POINT('Ctrl Pts',(1.81186451913824,-8.75567295717225,19.7308068537822));
#59369=CARTESIAN_POINT('Ctrl Pts',(1.8357835522898,-8.6655408027488,19.7728605743248));
#59370=CARTESIAN_POINT('Ctrl Pts',(1.85214505346338,-8.62643565005096,19.7914686907898));
#59371=CARTESIAN_POINT('Ctrl Pts',(1.88061329933222,-8.58294107520611,19.8130641352128));
#59372=CARTESIAN_POINT('Ctrl Pts',(1.89448595076454,-8.56525519087471,19.8220366846582));
#59373=CARTESIAN_POINT('Ctrl Pts',(1.92022261572012,-8.54803282135671,19.8319176857523));
#59374=CARTESIAN_POINT('Ctrl Pts',(1.92864558703646,-8.54389492576558,19.8345024437447));
#59375=CARTESIAN_POINT('Ctrl Pts',(1.94192278721308,-8.54037467545699,19.8372829641462));
#59376=CARTESIAN_POINT('Ctrl Pts',(1.94616291414767,-8.5396427768739,19.8380018808868));
#59377=CARTESIAN_POINT('Ctrl Pts',(1.95291207287856,-8.53914154119839,19.8388604862844));
#59378=CARTESIAN_POINT('Ctrl Pts',(1.95533909579901,-8.53909210866278,19.8391129317611));
#59379=CARTESIAN_POINT('Ctrl Pts',(1.95776807072638,-8.5391735580698,19.8393092308925));
#59380=CARTESIAN_POINT('',(1.65494820650842,-12.2959121221581,20.8349473401973));
#59381=CARTESIAN_POINT('Origin',(1.65494820650842,-9.9949023346812,21.8857832998643));
#59382=CARTESIAN_POINT('',(1.36757616935991,-12.0085309043509,20.9273996982545));
#59383=CARTESIAN_POINT('Origin',(1.6653400148523,-12.0237188108135,20.9606565744588));
#59384=CARTESIAN_POINT('Origin',(1.36757616935991,-9.98024447851016,21.8536870719015));
#59385=CARTESIAN_POINT('Origin',(1.65494820650842,-9.9949023346812,21.8857832998643));
#59386=CARTESIAN_POINT('Origin',(6.4980472271939,-10.24193210686,22.4267030489007));
#59387=CARTESIAN_POINT('',(11.664677238709,-9.78032664122358,20.2056359204057));
#59388=CARTESIAN_POINT('Ctrl Pts',(11.664677238709,-9.78032664122359,20.2056359204057));
#59389=CARTESIAN_POINT('Ctrl Pts',(8.44908820479151,-9.65515767378836,19.9536710841398));
#59390=CARTESIAN_POINT('Ctrl Pts',(5.17648536371074,-9.52748760709608,19.697374593167));
#59391=CARTESIAN_POINT('Ctrl Pts',(1.95776807072638,-9.40158004320576,19.4454613857581));
#59392=CARTESIAN_POINT('',(11.3203626311916,-13.0982396153547,21.7732001549839));
#59393=CARTESIAN_POINT('Origin',(11.3203626311916,-10.4879017784557,22.9653015014543));
#59394=CARTESIAN_POINT('',(11.664677238709,-8.86564886390743,20.6233552648184));
#59395=CARTESIAN_POINT('Origin',(11.3203626311916,-10.4879017784557,22.9653015014543));
#59396=CARTESIAN_POINT('Ctrl Pts',(1.95776807072638,-8.5391735580698,19.8393092308925));
#59397=CARTESIAN_POINT('Ctrl Pts',(5.17648535775567,-8.64710493744507,20.0994318861236));
#59398=CARTESIAN_POINT('Ctrl Pts',(8.44908819833864,-8.7571947878114,20.3637569928305));
#59399=CARTESIAN_POINT('Ctrl Pts',(11.664677238709,-8.86564886390743,20.6233552648184));
#59400=CARTESIAN_POINT('Origin',(11.3307544395355,-10.4884318287472,22.9664621496957));
#59401=CARTESIAN_POINT('',(11.6285182850279,-12.8412342104726,21.9321662654496));
#59402=CARTESIAN_POINT('Origin',(11.6285182850279,-10.5036197352098,22.9997190259));
#59403=CARTESIAN_POINT('Origin',(11.3307544395355,-12.8260463040101,21.8989093892453));
#59404=CARTESIAN_POINT('Ctrl Pts',(11.664677238709,-8.86564886390743,20.6233552648184));
#59405=CARTESIAN_POINT('Ctrl Pts',(11.6681531449969,-8.86576609785752,20.6236358788069));
#59406=CARTESIAN_POINT('Ctrl Pts',(11.6716331726355,-8.86616731353295,20.6237948130829));
#59407=CARTESIAN_POINT('Ctrl Pts',(11.6751111337893,-8.86685375084358,20.623830903915));
#59408=CARTESIAN_POINT('Ctrl Pts',(11.6835034416364,-8.86851012162341,20.6239179909639));
#59409=CARTESIAN_POINT('Ctrl Pts',(11.6913221163004,-8.87170945339749,20.6232869878783));
#59410=CARTESIAN_POINT('Ctrl Pts',(11.7093237578239,-8.88207391467147,20.6205407109361));
#59411=CARTESIAN_POINT('Ctrl Pts',(11.7187565997267,-8.89041824124023,20.6178443174412));
#59412=CARTESIAN_POINT('Ctrl Pts',(11.7431727782354,-8.91707792401486,20.6086622526054));
#59413=CARTESIAN_POINT('Ctrl Pts',(11.7560898230283,-8.9391731957824,20.6003233906747));
#59414=CARTESIAN_POINT('Ctrl Pts',(11.7841758181737,-8.99805910753514,20.5773806426634));
#59415=CARTESIAN_POINT('Ctrl Pts',(11.7988195826634,-9.04537291470731,20.5580695606802));
#59416=CARTESIAN_POINT('Ctrl Pts',(11.8183861888449,-9.14332972967485,20.5165359590653));
#59417=CARTESIAN_POINT('Ctrl Pts',(11.8239771978735,-9.18842241074048,20.4969162334911));
#59418=CARTESIAN_POINT('Ctrl Pts',(11.8302306705076,-9.27219438300235,20.4597498600097));
#59419=CARTESIAN_POINT('Ctrl Pts',(11.8313291886565,-9.31273094134293,20.4414345067909));
#59420=CARTESIAN_POINT('Ctrl Pts',(11.8301000822046,-9.39324349826429,20.4044483831864));
#59421=CARTESIAN_POINT('Ctrl Pts',(11.8275983467483,-9.43446674805149,20.3851769035864));
#59422=CARTESIAN_POINT('Ctrl Pts',(11.8179490511515,-9.51988766495155,20.344508477833));
#59423=CARTESIAN_POINT('Ctrl Pts',(11.8098404493788,-9.56648167385494,20.3218506008119));
#59424=CARTESIAN_POINT('Ctrl Pts',(11.7817370234731,-9.66788637809189,20.2711283205783));
#59425=CARTESIAN_POINT('Ctrl Pts',(11.7608617911999,-9.71153922107345,20.2481472837838));
#59426=CARTESIAN_POINT('Ctrl Pts',(11.727864569176,-9.75179858555561,20.2255615388921));
#59427=CARTESIAN_POINT('Ctrl Pts',(11.7163738956147,-9.76278438208105,20.2191422746271));
#59428=CARTESIAN_POINT('Ctrl Pts',(11.6949981921877,-9.77494241482736,20.2111886963504));
#59429=CARTESIAN_POINT('Ctrl Pts',(11.6861739271888,-9.77828873356616,20.2087116448862));
#59430=CARTESIAN_POINT('Ctrl Pts',(11.6727399598044,-9.78026828421812,20.2064478679052));
#59431=CARTESIAN_POINT('Ctrl Pts',(11.6686987410324,-9.78048318090824,20.2059510344218));
#59432=CARTESIAN_POINT('Ctrl Pts',(11.664677238709,-9.78032664122358,20.2056359204057));
#59433=CARTESIAN_POINT('Origin',(11.6285182850279,-10.5036197352098,22.9997190259));
#59434=CARTESIAN_POINT('Origin',(1.06052702375292,-11.0190788716665,24.1284170944427));
#59435=CARTESIAN_POINT('Origin',(1.6653400148523,-3.42428246167523,23.8164076546558));
#59436=CARTESIAN_POINT('',(1.95776807072638,-3.54233043715926,21.3065147522487));
#59437=CARTESIAN_POINT('',(1.95776807072638,-2.60389771385557,21.4414410082343));
#59438=CARTESIAN_POINT('Ctrl Pts',(1.95776807072638,-3.54233043715926,21.3065147522487));
#59439=CARTESIAN_POINT('Ctrl Pts',(1.9513478551886,-3.54223103321939,21.3059618726496));
#59440=CARTESIAN_POINT('Ctrl Pts',(1.94501663599474,-3.54115156508234,21.3055798899085));
#59441=CARTESIAN_POINT('Ctrl Pts',(1.92952577557711,-3.53620362915065,21.3050279766057));
#59442=CARTESIAN_POINT('Ctrl Pts',(1.92095957337031,-3.53135931038363,21.3050724139772));
#59443=CARTESIAN_POINT('Ctrl Pts',(1.90072805817451,-3.51599592158736,21.3058205399649));
#59444=CARTESIAN_POINT('Ctrl Pts',(1.8900249560485,-3.5036082187607,21.3069139518805));
#59445=CARTESIAN_POINT('Ctrl Pts',(1.86013121923956,-3.460751246541,21.3112847102786));
#59446=CARTESIAN_POINT('Ctrl Pts',(1.84584490211046,-3.42403619031247,21.3159449618369));
#59447=CARTESIAN_POINT('Ctrl Pts',(1.82200825445925,-3.35110430677949,21.3254531739389));
#59448=CARTESIAN_POINT('Ctrl Pts',(1.81203215259484,-3.30105316932589,21.3323795986619));
#59449=CARTESIAN_POINT('Ctrl Pts',(1.79984169249385,-3.21193645609613,21.3448875851979));
#59450=CARTESIAN_POINT('Ctrl Pts',(1.79638078494031,-3.16936789071313,21.3509444797466));
#59451=CARTESIAN_POINT('Ctrl Pts',(1.793278948137,-3.08828446690857,21.3625442583892));
#59452=CARTESIAN_POINT('Ctrl Pts',(1.79337026915323,-3.04840338066611,21.36827974357));
#59453=CARTESIAN_POINT('Ctrl Pts',(1.79687828838527,-2.96705307114361,21.3800426367112));
#59454=CARTESIAN_POINT('Ctrl Pts',(1.80059938175366,-2.9241782817627,21.3862765917232));
#59455=CARTESIAN_POINT('Ctrl Pts',(1.81351118858407,-2.83463727606628,21.3994816448112));
#59456=CARTESIAN_POINT('Ctrl Pts',(1.82404219007376,-2.78419034711654,21.4070273995978));
#59457=CARTESIAN_POINT('Ctrl Pts',(1.84885798811656,-2.71258004937708,21.418374529977));
#59458=CARTESIAN_POINT('Ctrl Pts',(1.86388962647735,-2.67578411025365,21.4243315771977));
#59459=CARTESIAN_POINT('Ctrl Pts',(1.89490216133889,-2.63563438874777,21.4320245979053));
#59460=CARTESIAN_POINT('Ctrl Pts',(1.90722460488827,-2.62233152903652,21.4347412883592));
#59461=CARTESIAN_POINT('Ctrl Pts',(1.92907437017015,-2.60993293818409,21.4381786237551));
#59462=CARTESIAN_POINT('Ctrl Pts',(1.93579728934589,-2.60716195128727,21.439108054393));
#59463=CARTESIAN_POINT('Ctrl Pts',(1.94779808654528,-2.60440407097886,21.440500869962));
#59464=CARTESIAN_POINT('Ctrl Pts',(1.95276363818101,-2.60385064352413,21.4410056766482));
#59465=CARTESIAN_POINT('Ctrl Pts',(1.95776807072638,-2.60389771385557,21.4414410082343));
#59466=CARTESIAN_POINT('',(1.65494820650842,-5.92795829958165,23.4551443394205));
#59467=CARTESIAN_POINT('Origin',(1.65494820650842,-3.42410087454152,23.8151446883994));
#59468=CARTESIAN_POINT('',(1.36757616935991,-5.62617120112542,23.4628870820895));
#59469=CARTESIAN_POINT('Origin',(1.6653400148523,-5.63137434589457,23.4990757488526));
#59470=CARTESIAN_POINT('Origin',(1.36757616935991,-3.41907931690608,23.7802189878927));
#59471=CARTESIAN_POINT('Origin',(1.65494820650842,-3.42410087454152,23.8151446883994));
#59472=CARTESIAN_POINT('Origin',(6.4980472271939,-3.50872950127858,24.4037497162211));
#59473=CARTESIAN_POINT('',(11.664677238709,-3.69156922144577,22.1426021244183));
#59474=CARTESIAN_POINT('Ctrl Pts',(11.664677238709,-3.69156922144575,22.1426021244183));
#59475=CARTESIAN_POINT('Ctrl Pts',(8.45131537604982,-3.64249119006552,21.8657713317644));
#59476=CARTESIAN_POINT('Ctrl Pts',(5.17772237568178,-3.5921848606183,21.5838024904321));
#59477=CARTESIAN_POINT('Ctrl Pts',(1.95776807072638,-3.54233043715926,21.3065147522487));
#59478=CARTESIAN_POINT('',(11.3203626311916,-6.43344952736807,24.5814330987647));
#59479=CARTESIAN_POINT('Origin',(11.3203626311916,-3.59299495374821,24.98982881153));
#59480=CARTESIAN_POINT('',(11.664677238709,-2.69625718204607,22.2857063914358));
#59481=CARTESIAN_POINT('Origin',(11.3203626311916,-3.59299495374821,24.98982881153));
#59482=CARTESIAN_POINT('Ctrl Pts',(1.95776807072638,-2.60389771385557,21.4414410082343));
#59483=CARTESIAN_POINT('Ctrl Pts',(5.17772236984729,-2.63418372824733,21.7215422583742));
#59484=CARTESIAN_POINT('Ctrl Pts',(8.45131536953639,-2.66535496122479,22.0062623111724));
#59485=CARTESIAN_POINT('Ctrl Pts',(11.664677238709,-2.69625718204608,22.2857063914358));
#59486=CARTESIAN_POINT('Origin',(11.3307544395355,-3.59317654088192,24.9910917777863));
#59487=CARTESIAN_POINT('',(11.6285182850279,-6.14206871845015,24.6615531749599));
#59488=CARTESIAN_POINT('Origin',(11.6285182850279,-3.59837968565107,25.0272804445494));
#59489=CARTESIAN_POINT('Origin',(11.3307544395355,-6.136865573681,24.6253645081968));
#59490=CARTESIAN_POINT('Ctrl Pts',(11.664677238709,-2.69625718204609,22.2857063914358));
#59491=CARTESIAN_POINT('Ctrl Pts',(11.6681739314188,-2.69629080899963,22.2860104748593));
#59492=CARTESIAN_POINT('Ctrl Pts',(11.6716539907384,-2.69663467728557,22.2862755639135));
#59493=CARTESIAN_POINT('Ctrl Pts',(11.6751111337893,-2.69727925957649,22.2865022196842));
#59494=CARTESIAN_POINT('Ctrl Pts',(11.6834715430146,-2.69883805296518,22.2870503413465));
#59495=CARTESIAN_POINT('Ctrl Pts',(11.6912510114763,-2.70206385531499,22.2873454247033));
#59496=CARTESIAN_POINT('Ctrl Pts',(11.709035822972,-2.71261693877732,22.2876313864347));
#59497=CARTESIAN_POINT('Ctrl Pts',(11.7183186554656,-2.72116951930901,22.2874079360076));
#59498=CARTESIAN_POINT('Ctrl Pts',(11.7418333015259,-2.74801369053582,22.2861920544586));
#59499=CARTESIAN_POINT('Ctrl Pts',(11.7542369034695,-2.7699680354384,22.2845703704499));
#59500=CARTESIAN_POINT('Ctrl Pts',(11.7824157539259,-2.83096774741543,22.2794147158946));
#59501=CARTESIAN_POINT('Ctrl Pts',(11.797437382068,-2.88153241037179,22.2742976507484));
#59502=CARTESIAN_POINT('Ctrl Pts',(11.8209603099608,-3.00475150470514,22.2601056375114));
#59503=CARTESIAN_POINT('Ctrl Pts',(11.8274214370012,-3.07312747241122,22.2513392489145));
#59504=CARTESIAN_POINT('Ctrl Pts',(11.8323708659761,-3.20740533159261,22.2328342493678));
#59505=CARTESIAN_POINT('Ctrl Pts',(11.8303885473322,-3.27899188856714,22.2222076907846));
#59506=CARTESIAN_POINT('Ctrl Pts',(11.8177935569394,-3.40658761118928,22.2018688414514));
#59507=CARTESIAN_POINT('Ctrl Pts',(11.8075558566742,-3.4692947461111,22.1912401030955));
#59508=CARTESIAN_POINT('Ctrl Pts',(11.7765253671338,-3.57657231689547,22.1714404504546));
#59509=CARTESIAN_POINT('Ctrl Pts',(11.7586671916647,-3.61570515885675,22.1634661165603));
#59510=CARTESIAN_POINT('Ctrl Pts',(11.7297382659251,-3.65639661653946,22.1542106095143));
#59511=CARTESIAN_POINT('Ctrl Pts',(11.7183817710579,-3.66905637710909,22.1511082048343));
#59512=CARTESIAN_POINT('Ctrl Pts',(11.6971067724022,-3.68375234586312,22.1467808943914));
#59513=CARTESIAN_POINT('Ctrl Pts',(11.688166617688,-3.68804578318867,22.1452727334554));
#59514=CARTESIAN_POINT('Ctrl Pts',(11.6739702938601,-3.69116836143547,22.1434932346172));
#59515=CARTESIAN_POINT('Ctrl Pts',(11.6693161741268,-3.69164007241986,22.1430017682255));
#59516=CARTESIAN_POINT('Ctrl Pts',(11.664677238709,-3.69156922144579,22.1426021244183));
#59517=CARTESIAN_POINT('Origin',(11.6285182850279,-3.59837968565107,25.0272804445494));
#59518=CARTESIAN_POINT('Origin',(1.06052702375292,-3.77496811251421,26.2554799311097));
#59519=CARTESIAN_POINT('Origin',(1.6653400148523,3.42428246167523,23.8164076546558));
#59520=CARTESIAN_POINT('',(1.95776807072638,2.60389771385558,21.4414410082343));
#59521=CARTESIAN_POINT('',(1.95776807072638,3.54233043715926,21.3065147522487));
#59522=CARTESIAN_POINT('Ctrl Pts',(1.95776807072638,2.60389771385558,21.4414410082343));
#59523=CARTESIAN_POINT('Ctrl Pts',(1.95134785518859,2.60383732705436,21.4408825188176));
#59524=CARTESIAN_POINT('Ctrl Pts',(1.94501663599474,2.60476545217276,21.4402118877432));
#59525=CARTESIAN_POINT('Ctrl Pts',(1.92952577557707,2.6093574699872,21.4382883361661));
#59526=CARTESIAN_POINT('Ctrl Pts',(1.92095957337023,2.61401807926046,21.4369661711994));
#59527=CARTESIAN_POINT('Ctrl Pts',(1.90072805817454,2.62896991430866,21.4333556260207));
#59528=CARTESIAN_POINT('Ctrl Pts',(1.89002495604858,2.64116387786459,21.4309147278802));
#59529=CARTESIAN_POINT('Ctrl Pts',(1.86013121923974,2.68351622651848,21.4230342354906));
#59530=CARTESIAN_POINT('Ctrl Pts',(1.84584490211065,2.72005700958236,21.4171618874503));
#59531=CARTESIAN_POINT('Ctrl Pts',(1.82200825445924,2.79271341229181,21.4057376641306));
#59532=CARTESIAN_POINT('Ctrl Pts',(1.81203215259483,2.842688526347,21.398282485057));
#59533=CARTESIAN_POINT('Ctrl Pts',(1.79984169249385,2.93171929355019,21.3851767307768));
#59534=CARTESIAN_POINT('Ctrl Pts',(1.79638078494032,2.97426995731976,21.3789953277719));
#59535=CARTESIAN_POINT('Ctrl Pts',(1.79327894813701,3.05533696803247,21.367281393569));
#59536=CARTESIAN_POINT('Ctrl Pts',(1.79337026915323,3.09521846296703,21.3615487509036));
#59537=CARTESIAN_POINT('Ctrl Pts',(1.79687828838528,3.17658750331596,21.3499161335203));
#59538=CARTESIAN_POINT('Ctrl Pts',(1.80059938175367,3.21948187055682,21.3438183455158));
#59539=CARTESIAN_POINT('Ctrl Pts',(1.81351118858406,3.30911612974249,21.331261884693));
#59540=CARTESIAN_POINT('Ctrl Pts',(1.82404219007375,3.35964548839958,21.3242894411135));
#59541=CARTESIAN_POINT('Ctrl Pts',(1.84885798811638,3.43155192197307,21.3150019807047));
#59542=CARTESIAN_POINT('Ctrl Pts',(1.8638896264772,3.46853566116457,21.3103511116458));
#59543=CARTESIAN_POINT('Ctrl Pts',(1.89490216133104,3.50922641122572,21.3064210272653));
#59544=CARTESIAN_POINT('Ctrl Pts',(1.90722460488041,3.52275579180111,21.3052798239866));
#59545=CARTESIAN_POINT('Ctrl Pts',(1.92907437017047,3.53562056190136,21.3050848364448));
#59546=CARTESIAN_POINT('Ctrl Pts',(1.93579728934604,3.53854115522866,21.305195941388));
#59547=CARTESIAN_POINT('Ctrl Pts',(1.94779808654526,3.54157972349806,21.3057553534692));
#59548=CARTESIAN_POINT('Ctrl Pts',(1.952763638181,3.54225295373072,21.3060837934058));
#59549=CARTESIAN_POINT('Ctrl Pts',(1.95776807072638,3.54233043715926,21.3065147522487));
#59550=CARTESIAN_POINT('',(1.65494820650842,0.920243449501388,24.1751450373783));
#59551=CARTESIAN_POINT('Origin',(1.65494820650842,3.42410087454152,23.8151446883994));
#59552=CARTESIAN_POINT('',(1.36757616935991,1.21198743268674,24.0975508936959));
#59553=CARTESIAN_POINT('Origin',(1.6653400148523,1.21719057745589,24.133739560459));
#59554=CARTESIAN_POINT('Origin',(1.36757616935991,3.41907931690608,23.7802189878927));
#59555=CARTESIAN_POINT('Origin',(1.65494820650842,3.42410087454152,23.8151446883994));
#59556=CARTESIAN_POINT('Origin',(6.4980472271939,3.50872950127858,24.4037497162211));
#59557=CARTESIAN_POINT('',(11.664677238709,2.69625718204608,22.2857063914358));
#59558=CARTESIAN_POINT('Ctrl Pts',(11.664677238709,2.69625718204609,22.2857063914358));
#59559=CARTESIAN_POINT('Ctrl Pts',(8.45131537604982,2.66535496128743,22.0062623117388));
#59560=CARTESIAN_POINT('Ctrl Pts',(5.17772237568179,2.63418372830221,21.7215422588817));
#59561=CARTESIAN_POINT('Ctrl Pts',(1.95776807072638,2.60389771385557,21.4414410082343));
#59562=CARTESIAN_POINT('',(11.3203626311916,0.752540380128346,25.3982245242953));
#59563=CARTESIAN_POINT('Origin',(11.3203626311916,3.59299495374821,24.98982881153));
#59564=CARTESIAN_POINT('',(11.664677238709,3.69156922144577,22.1426021244183));
#59565=CARTESIAN_POINT('Origin',(11.3203626311916,3.59299495374821,24.98982881153));
#59566=CARTESIAN_POINT('Ctrl Pts',(1.95776807072638,3.54233043715926,21.3065147522487));
#59567=CARTESIAN_POINT('Ctrl Pts',(5.17772236984729,3.59218486052797,21.5838024899296));
#59568=CARTESIAN_POINT('Ctrl Pts',(8.45131536953639,3.64249118996605,21.8657713312033));
#59569=CARTESIAN_POINT('Ctrl Pts',(11.664677238709,3.69156922144575,22.1426021244183));
#59570=CARTESIAN_POINT('Origin',(11.3307544395355,3.59317654088192,24.9910917777863));
#59571=CARTESIAN_POINT('',(11.6285182850279,1.054690652852,25.393007714139));
#59572=CARTESIAN_POINT('Origin',(11.6285182850279,3.59837968565108,25.0272804445494));
#59573=CARTESIAN_POINT('Origin',(11.3307544395355,1.04948750808285,25.3568190473759));
#59574=CARTESIAN_POINT('Ctrl Pts',(11.664677238709,3.69156922144577,22.1426021244183));
#59575=CARTESIAN_POINT('Ctrl Pts',(11.6681739314189,3.69162262682054,22.1429033641341));
#59576=CARTESIAN_POINT('Ctrl Pts',(11.6716539907386,3.6913673718333,22.1432545941104));
#59577=CARTESIAN_POINT('Ctrl Pts',(11.6751111337893,3.69081275596405,22.1436536685467));
#59578=CARTESIAN_POINT('Ctrl Pts',(11.6834715430145,3.68947152837768,22.1446187502773));
#59579=CARTESIAN_POINT('Ctrl Pts',(11.6912510114761,3.68645952827754,22.1458106942287));
#59580=CARTESIAN_POINT('Ctrl Pts',(11.7090358229721,3.67641448357504,22.1490582196872));
#59581=CARTESIAN_POINT('Ctrl Pts',(11.7183186554658,3.66814538938823,22.1512533609532));
#59582=CARTESIAN_POINT('Ctrl Pts',(11.7418333015259,3.6420460422962,22.1576496081462));
#59583=CARTESIAN_POINT('Ctrl Pts',(11.7542369034695,3.62052412143971,22.1622788674576));
#59584=CARTESIAN_POINT('Ctrl Pts',(11.7824157539258,3.56054281066528,22.1745176579593));
#59585=CARTESIAN_POINT('Ctrl Pts',(11.797437382068,3.51058472799836,22.1838535816865));
#59586=CARTESIAN_POINT('Ctrl Pts',(11.8209603099608,3.38835852059419,22.2049512752024));
#59587=CARTESIAN_POINT('Ctrl Pts',(11.8274214370012,3.32028248294247,22.215803723148));
#59588=CARTESIAN_POINT('Ctrl Pts',(11.8323708659761,3.18623035970919,22.2358787507006));
#59589=CARTESIAN_POINT('Ctrl Pts',(11.8303885473322,3.11454971376682,22.2458509061382));
#59590=CARTESIAN_POINT('Ctrl Pts',(11.8177935569394,2.9863923984218,22.2622837922879));
#59591=CARTESIAN_POINT('Ctrl Pts',(11.8075558566742,2.92323088143582,22.2697522339709));
#59592=CARTESIAN_POINT('Ctrl Pts',(11.7765253671337,2.8147205992782,22.2809781906907));
#59593=CARTESIAN_POINT('Ctrl Pts',(11.7586671916645,2.77492628290187,22.2843518689721));
#59594=CARTESIAN_POINT('Ctrl Pts',(11.7297382659251,2.73327553750452,22.2869353834087));
#59595=CARTESIAN_POINT('Ctrl Pts',(11.7183817710578,2.7202545377875,22.2875253146313));
#59596=CARTESIAN_POINT('Ctrl Pts',(11.6971067724021,2.70493471479212,22.287513623519));
#59597=CARTESIAN_POINT('Ctrl Pts',(11.688166617688,2.70039029380911,22.2872761547731));
#59598=CARTESIAN_POINT('Ctrl Pts',(11.6739702938601,2.69689285916418,22.2864484700947));
#59599=CARTESIAN_POINT('Ctrl Pts',(11.6693161741268,2.69630179370592,22.2861098078869));
#59600=CARTESIAN_POINT('Ctrl Pts',(11.664677238709,2.69625718204608,22.2857063914358));
#59601=CARTESIAN_POINT('Origin',(11.6285182850279,3.59837968565108,25.0272804445494));
#59602=CARTESIAN_POINT('Origin',(1.06052702375292,3.77496811251421,26.2554799311097));
#59603=CARTESIAN_POINT('Origin',(1.6653400148523,9.99543238497271,21.8869439481057));
#59604=CARTESIAN_POINT('',(1.95776807072638,8.53917355806981,19.8393092308925));
#59605=CARTESIAN_POINT('',(1.95776807072638,9.40158004320575,19.4454613857581));
#59606=CARTESIAN_POINT('Ctrl Pts',(1.95776807072638,8.53917355806979,19.8393092308925));
#59607=CARTESIAN_POINT('Ctrl Pts',(1.95134736181104,8.53895825616285,19.8387903372766));
#59608=CARTESIAN_POINT('Ctrl Pts',(1.94501567122259,8.53965997172072,19.8378852898847));
#59609=CARTESIAN_POINT('Ctrl Pts',(1.92948836979272,8.54353347509978,19.8347384067269));
#59610=CARTESIAN_POINT('Ctrl Pts',(1.92089186233936,8.54765577357339,19.8321439694453));
#59611=CARTESIAN_POINT('Ctrl Pts',(1.90046800930124,8.56114336986575,19.8243804604409));
#59612=CARTESIAN_POINT('Ctrl Pts',(1.88964186308543,8.57236355197253,19.8185013079907));
#59613=CARTESIAN_POINT('Ctrl Pts',(1.85810283833411,8.61322946498717,19.7977884699131));
#59614=CARTESIAN_POINT('Ctrl Pts',(1.84335629303613,8.64977779572247,19.7804322617419));
#59615=CARTESIAN_POINT('Ctrl Pts',(1.81854010589151,8.72212855294431,19.7463114584517));
#59616=CARTESIAN_POINT('Ctrl Pts',(1.8083691782646,8.77440559157947,19.7221699251049));
#59617=CARTESIAN_POINT('Ctrl Pts',(1.79896764765282,8.85022287567161,19.6873082756821));
#59618=CARTESIAN_POINT('Ctrl Pts',(1.79670145400052,8.87696000159275,19.6750497681665));
#59619=CARTESIAN_POINT('Ctrl Pts',(1.79434535609109,8.92267523692494,19.6541233115618));
#59620=CARTESIAN_POINT('Ctrl Pts',(1.7938155730381,8.94195225085063,19.6453095312538));
#59621=CARTESIAN_POINT('Ctrl Pts',(1.79365032105971,8.97982124967058,19.6280120764218));
#59622=CARTESIAN_POINT('Ctrl Pts',(1.79398945985935,8.99855959580194,19.6194610836778));
#59623=CARTESIAN_POINT('Ctrl Pts',(1.79575501944583,9.04148989103746,19.5998915295602));
#59624=CARTESIAN_POINT('Ctrl Pts',(1.79749007695656,9.06591922657839,19.588770848701));
#59625=CARTESIAN_POINT('Ctrl Pts',(1.80455267777006,9.13321443405714,19.558206436516));
#59626=CARTESIAN_POINT('Ctrl Pts',(1.81186451913824,9.17780246249336,19.5380267681685));
#59627=CARTESIAN_POINT('Ctrl Pts',(1.83578355229015,9.2686085526925,19.4974487611264));
#59628=CARTESIAN_POINT('Ctrl Pts',(1.85214505346393,9.30828005778674,19.4800807834258));
#59629=CARTESIAN_POINT('Ctrl Pts',(1.88061329933267,9.35308369492278,19.4613517855849));
#59630=CARTESIAN_POINT('Ctrl Pts',(1.89448595076488,9.37144648654037,19.4538614563447));
#59631=CARTESIAN_POINT('Ctrl Pts',(1.92022261572016,9.39019230245401,19.4473163375408));
#59632=CARTESIAN_POINT('Ctrl Pts',(1.92864558703649,9.39485547755034,19.445881781225));
#59633=CARTESIAN_POINT('Ctrl Pts',(1.94192278721305,9.39926212836099,19.4450422071836));
#59634=CARTESIAN_POINT('Ctrl Pts',(1.94616291414765,9.40028474102504,19.4449598654854));
#59635=CARTESIAN_POINT('Ctrl Pts',(1.95291207287644,9.40126187125082,19.4451433237977));
#59636=CARTESIAN_POINT('Ctrl Pts',(1.95533909579739,9.40148502823919,19.4452712818101));
#59637=CARTESIAN_POINT('Ctrl Pts',(1.95776807072638,9.40158004320578,19.4454613857581));
#59638=CARTESIAN_POINT('',(1.65494820650842,7.69389254720435,22.9366192595313));
#59639=CARTESIAN_POINT('Origin',(1.65494820650842,9.99490233468121,21.8857832998643));
#59640=CARTESIAN_POINT('',(1.36757616935991,7.95195805266942,22.7799744455484));
#59641=CARTESIAN_POINT('Origin',(1.6653400148523,7.96714595913197,22.8132313217527));
#59642=CARTESIAN_POINT('Origin',(1.36757616935991,9.98024447851016,21.8536870719015));
#59643=CARTESIAN_POINT('Origin',(1.65494820650842,9.99490233468121,21.8857832998643));
#59644=CARTESIAN_POINT('Origin',(6.4980472271939,10.24193210686,22.4267030489007));
#59645=CARTESIAN_POINT('',(11.664677238709,8.86564886390743,20.6233552648184));
#59646=CARTESIAN_POINT('Ctrl Pts',(11.664677238709,8.86564886390742,20.6233552648184));
#59647=CARTESIAN_POINT('Ctrl Pts',(8.44908820479151,8.75719478802903,20.3637569933514));
#59648=CARTESIAN_POINT('Ctrl Pts',(5.17648536371074,8.64710493764475,20.0994318866049));
#59649=CARTESIAN_POINT('Ctrl Pts',(1.95776807072638,8.53917355806979,19.8393092308925));
#59650=CARTESIAN_POINT('',(11.3203626311916,7.87756394155674,24.1574028479247));
#59651=CARTESIAN_POINT('Origin',(11.3203626311916,10.4879017784557,22.9653015014543));
#59652=CARTESIAN_POINT('',(11.664677238709,9.78032664122359,20.2056359204057));
#59653=CARTESIAN_POINT('Origin',(11.3203626311916,10.4879017784557,22.9653015014543));
#59654=CARTESIAN_POINT('Ctrl Pts',(1.95776807072638,9.40158004320577,19.4454613857581));
#59655=CARTESIAN_POINT('Ctrl Pts',(5.17648535775567,9.52748760686315,19.6973745927009));
#59656=CARTESIAN_POINT('Ctrl Pts',(8.44908819833864,9.65515767353719,19.9536710836342));
#59657=CARTESIAN_POINT('Ctrl Pts',(11.664677238709,9.7803266412236,20.2056359204057));
#59658=CARTESIAN_POINT('Origin',(11.3307544395355,10.4884318287472,22.9664621496957));
#59659=CARTESIAN_POINT('',(11.6285182850279,8.16600525994691,24.0672717863504));
#59660=CARTESIAN_POINT('Origin',(11.6285182850279,10.5036197352098,22.9997190259));
#59661=CARTESIAN_POINT('Origin',(11.3307544395355,8.15081735348436,24.0340149101461));
#59662=CARTESIAN_POINT('Ctrl Pts',(11.664677238709,9.78032664122359,20.2056359204057));
#59663=CARTESIAN_POINT('Ctrl Pts',(11.6681531449969,9.78046194321534,20.205908282996));
#59664=CARTESIAN_POINT('Ctrl Pts',(11.6716331726355,9.7803193173351,20.2063155813886));
#59665=CARTESIAN_POINT('Ctrl Pts',(11.6751111337893,9.77989707212502,20.2068579905627));
#59666=CARTESIAN_POINT('Ctrl Pts',(11.6835034416363,9.77887819594063,20.2081668219633));
#59667=CARTESIAN_POINT('Ctrl Pts',(11.6913221163002,9.77630619887362,20.210171496446));
#59668=CARTESIAN_POINT('Ctrl Pts',(11.709323757824,9.76744342252662,20.2162060047083));
#59669=CARTESIAN_POINT('Ctrl Pts',(11.7187565997267,9.7599412524694,20.2207464637378));
#59670=CARTESIAN_POINT('Ctrl Pts',(11.7431727782355,9.73554353144946,20.2348815339297));
#59671=CARTESIAN_POINT('Ctrl Pts',(11.7560898230284,9.7147721142082,20.2461192329191));
#59672=CARTESIAN_POINT('Ctrl Pts',(11.7841758181731,9.65887107077625,20.2755979308595));
#59673=CARTESIAN_POINT('Ctrl Pts',(11.798819582663,9.61329277429722,20.2987092511699));
#59674=CARTESIAN_POINT('Ctrl Pts',(11.8183861888449,9.51775570080864,20.3455413475508));
#59675=CARTESIAN_POINT('Ctrl Pts',(11.8239771978735,9.47339867533874,20.3667719341834));
#59676=CARTESIAN_POINT('Ctrl Pts',(11.8302306705076,9.39045122916063,20.4057437679469));
#59677=CARTESIAN_POINT('Ctrl Pts',(11.8313291886565,9.35006360841491,20.4243852490072));
#59678=CARTESIAN_POINT('Ctrl Pts',(11.8301000822046,9.26938684912612,20.4610118195814));
#59679=CARTESIAN_POINT('Ctrl Pts',(11.8275983467482,9.22782694901014,20.4795461377865));
#59680=CARTESIAN_POINT('Ctrl Pts',(11.8179490511515,9.141152999222,20.5174708042373));
#59681=CARTESIAN_POINT('Ctrl Pts',(11.8098404493788,9.0935167314396,20.5378464526579));
#59682=CARTESIAN_POINT('Ctrl Pts',(11.7817370234727,8.98877743069939,20.5812669850618));
#59683=CARTESIAN_POINT('Ctrl Pts',(11.7608617911994,8.94282298913066,20.599208223942));
#59684=CARTESIAN_POINT('Ctrl Pts',(11.7278645691761,8.89938954507017,20.6148437040365));
#59685=CARTESIAN_POINT('Ctrl Pts',(11.7163738956147,8.88734402205844,20.6189424909766));
#59686=CARTESIAN_POINT('Ctrl Pts',(11.6949981921877,8.87337129041363,20.6229224329418));
#59687=CARTESIAN_POINT('Ctrl Pts',(11.6861739271888,8.86930788707863,20.6238292881645));
#59688=CARTESIAN_POINT('Ctrl Pts',(11.6727399598044,8.86630070859597,20.6238428740718));
#59689=CARTESIAN_POINT('Ctrl Pts',(11.6686987410323,8.86578449949815,20.6236799254143));
#59690=CARTESIAN_POINT('Ctrl Pts',(11.664677238709,8.86564886390743,20.6233552648184));
#59691=CARTESIAN_POINT('Origin',(11.6285182850279,10.5036197352098,22.9997190259));
#59692=CARTESIAN_POINT('Origin',(1.06052702375292,11.0190788716665,24.1284170944427));
#59693=CARTESIAN_POINT('Origin',(1.6653400148523,15.756811821565,18.1843302095478));
#59694=CARTESIAN_POINT('',(1.95776807072638,13.7826563450298,16.6299146085789));
#59695=CARTESIAN_POINT('',(1.95776807072638,14.4991695475011,16.0090523844052));
#59696=CARTESIAN_POINT('Ctrl Pts',(1.95776807072638,13.7826563450298,16.6299146085789));
#59697=CARTESIAN_POINT('Ctrl Pts',(1.95134736178812,13.7823035751365,16.6294773913556));
#59698=CARTESIAN_POINT('Ctrl Pts',(1.94501567118683,13.7827218849757,16.628411308616));
#59699=CARTESIAN_POINT('Ctrl Pts',(1.92948836979218,13.7855519048067,16.6243006043356));
#59700=CARTESIAN_POINT('Ctrl Pts',(1.92089186233878,13.7887762837785,16.6206498743044));
#59701=CARTESIAN_POINT('Ctrl Pts',(1.90046800930057,13.7995303044103,16.6094009469748));
#59702=CARTESIAN_POINT('Ctrl Pts',(1.88964186308468,13.8086396416528,16.6005988509147));
#59703=CARTESIAN_POINT('Ctrl Pts',(1.858102838333,13.8420147172205,16.5692117701535));
#59704=CARTESIAN_POINT('Ctrl Pts',(1.84335629303492,13.8721927748541,16.5422617556975));
#59705=CARTESIAN_POINT('Ctrl Pts',(1.8185401058909,13.9319998768916,16.4891395208651));
#59706=CARTESIAN_POINT('Ctrl Pts',(1.80836917826425,13.975357872227,16.4512477454883));
#59707=CARTESIAN_POINT('Ctrl Pts',(1.79896764765271,14.0382823619637,16.3964380405191));
#59708=CARTESIAN_POINT('Ctrl Pts',(1.79670145400044,14.060482825754,16.3771433698427));
#59709=CARTESIAN_POINT('Ctrl Pts',(1.79434535609105,14.0984506087175,16.3441851116311));
#59710=CARTESIAN_POINT('Ctrl Pts',(1.79381557303809,14.1144636392699,16.3302973889329));
#59711=CARTESIAN_POINT('Ctrl Pts',(1.79365032105973,14.1459254213784,16.303031672698));
#59712=CARTESIAN_POINT('Ctrl Pts',(1.79398945985937,14.1614956397794,16.2895478530761));
#59713=CARTESIAN_POINT('Ctrl Pts',(1.79575501944589,14.1971735758954,16.2586761415607));
#59714=CARTESIAN_POINT('Ctrl Pts',(1.79749007695665,14.2174802938449,16.2411233872504));
#59715=CARTESIAN_POINT('Ctrl Pts',(1.80455267777032,14.2734385825861,16.1928377976495));
#59716=CARTESIAN_POINT('Ctrl Pts',(1.81186451913869,14.3105352130186,16.1609136484041));
#59717=CARTESIAN_POINT('Ctrl Pts',(1.83578355229124,14.3862308728513,16.0963963037948));
#59718=CARTESIAN_POINT('Ctrl Pts',(1.85214505346546,14.4194022784773,16.0685550966611));
#59719=CARTESIAN_POINT('Ctrl Pts',(1.88061329933466,14.4571144850523,16.0379621115844));
#59720=CARTESIAN_POINT('Ctrl Pts',(1.89448595076662,14.4726231849761,16.0256017970759));
#59721=CARTESIAN_POINT('Ctrl Pts',(1.92022261572143,14.4887656905737,16.0140404949253));
#59722=CARTESIAN_POINT('Ctrl Pts',(1.9286455870375,14.4928358130943,16.0113502799774));
#59723=CARTESIAN_POINT('Ctrl Pts',(1.94192278721348,14.4968274282426,16.009303217584));
#59724=CARTESIAN_POINT('Ctrl Pts',(1.94616291414806,14.4977854195713,16.0089361080226));
#59725=CARTESIAN_POINT('Ctrl Pts',(1.95291207281715,14.4987746553279,16.0088368455883));
#59726=CARTESIAN_POINT('Ctrl Pts',(1.95533909575199,14.4990248228342,16.0088967498094));
#59727=CARTESIAN_POINT('Ctrl Pts',(1.95776807072638,14.4991695475011,16.0090523844052));
#59728=CARTESIAN_POINT('',(1.65494820650842,13.8442282280737,19.8399049986041));
#59729=CARTESIAN_POINT('Origin',(1.65494820650842,15.755976249638,18.1833659081392));
#59730=CARTESIAN_POINT('',(1.36757616935991,14.0477083233403,19.6168999455472));
#59731=CARTESIAN_POINT('Origin',(1.6653400148523,14.0716505576406,19.6445307568688));
#59732=CARTESIAN_POINT('Origin',(1.36757616935991,15.7328695872647,18.1566993982262));
#59733=CARTESIAN_POINT('Origin',(1.65494820650842,15.755976249638,18.1833659081392));
#59734=CARTESIAN_POINT('Origin',(6.4980472271939,16.1453942842592,18.6327782772971));
#59735=CARTESIAN_POINT('',(11.664677238709,14.316798400859,17.2902225464619));
#59736=CARTESIAN_POINT('Ctrl Pts',(11.664677238709,14.316798400859,17.2902225464619));
#59737=CARTESIAN_POINT('Ctrl Pts',(8.44646649976651,14.1394557206779,17.0715167051139));
#59738=CARTESIAN_POINT('Ctrl Pts',(5.17487115867276,13.9594120777672,16.848982766429));
#59739=CARTESIAN_POINT('Ctrl Pts',(1.95776807072638,13.7826563450298,16.6299146085789));
#59740=CARTESIAN_POINT('',(11.3203626311916,14.3643941221169,20.959492062422));
#59741=CARTESIAN_POINT('Origin',(11.3203626311916,16.5331411750263,19.0802620436378));
#59742=CARTESIAN_POINT('',(11.664677238709,15.0767401623716,16.6317292616657));
#59743=CARTESIAN_POINT('Origin',(11.3203626311916,16.5331411750263,19.0802620436378));
#59744=CARTESIAN_POINT('Ctrl Pts',(1.95776807072638,14.4991695475011,16.0090523844052));
#59745=CARTESIAN_POINT('Ctrl Pts',(5.17487115257265,14.6908529434927,16.2151856477085));
#59746=CARTESIAN_POINT('Ctrl Pts',(8.44646649340719,14.8854989256118,16.4250665874126));
#59747=CARTESIAN_POINT('Ctrl Pts',(11.664677238709,15.0767401623716,16.6317292616657));
#59748=CARTESIAN_POINT('Origin',(11.3307544395355,16.5339767469533,19.0812263450464));
#59749=CARTESIAN_POINT('',(11.6285182850279,14.6157586859842,20.7917486320082));
#59750=CARTESIAN_POINT('Origin',(11.6285182850279,16.5579189812536,19.1088571563679));
#59751=CARTESIAN_POINT('Origin',(11.3307544395355,14.5918164516839,20.7641178206866));
#59752=CARTESIAN_POINT('Ctrl Pts',(11.664677238709,15.0767401623717,16.6317292616657));
#59753=CARTESIAN_POINT('Ctrl Pts',(11.6681719057553,15.0769478319436,16.6319536774341));
#59754=CARTESIAN_POINT('Ctrl Pts',(11.6716519636861,15.076923254483,16.6323869095799));
#59755=CARTESIAN_POINT('Ctrl Pts',(11.6751111337893,15.0766722907899,16.6330228529951));
#59756=CARTESIAN_POINT('Ctrl Pts',(11.6833639439589,15.0760735472598,16.6345400724807));
#59757=CARTESIAN_POINT('Ctrl Pts',(11.6912209922802,15.0742040415111,16.6371623459815));
#59758=CARTESIAN_POINT('Ctrl Pts',(11.7092716451021,15.0673685087776,16.6454839841325));
#59759=CARTESIAN_POINT('Ctrl Pts',(11.7188321121789,15.0614159673375,16.6519996438999));
#59760=CARTESIAN_POINT('Ctrl Pts',(11.7448362096952,15.0406027082649,16.6738751139891));
#59761=CARTESIAN_POINT('Ctrl Pts',(11.7582763496127,15.0220383775034,16.6921848294481));
#59762=CARTESIAN_POINT('Ctrl Pts',(11.7901173768955,14.9694389699155,16.743176931564));
#59763=CARTESIAN_POINT('Ctrl Pts',(11.807496900688,14.9187368040621,16.7905186715073));
#59764=CARTESIAN_POINT('Ctrl Pts',(11.8229354401012,14.8329485272452,16.8679921932309));
#59765=CARTESIAN_POINT('Ctrl Pts',(11.826199199177,14.8064785162731,16.8916135343912));
#59766=CARTESIAN_POINT('Ctrl Pts',(11.8295237141305,14.7632021791261,16.9298134645279));
#59767=CARTESIAN_POINT('Ctrl Pts',(11.8303434615844,14.7461967949088,16.9447232097654));
#59768=CARTESIAN_POINT('Ctrl Pts',(11.8309946485842,14.7141892768628,16.9725964133233));
#59769=CARTESIAN_POINT('Ctrl Pts',(11.8309459330901,14.6991103672785,16.9856519542831));
#59770=CARTESIAN_POINT('Ctrl Pts',(11.8300359252892,14.6661973816187,17.0139777482936));
#59771=CARTESIAN_POINT('Ctrl Pts',(11.8290394062419,14.648205145668,17.0293561720866));
#59772=CARTESIAN_POINT('Ctrl Pts',(11.8249644421306,14.6008656924252,17.0695195134069));
#59773=CARTESIAN_POINT('Ctrl Pts',(11.8209395722477,14.5708013862499,17.0947280327935));
#59774=CARTESIAN_POINT('Ctrl Pts',(11.8028867656277,14.4800669368877,17.1697247641798));
#59775=CARTESIAN_POINT('Ctrl Pts',(11.7841990134601,14.4273818427204,17.2117750105268));
#59776=CARTESIAN_POINT('Ctrl Pts',(11.7507704380578,14.3734252802354,17.2529915779606));
#59777=CARTESIAN_POINT('Ctrl Pts',(11.7371459986441,14.3544245174278,17.2672530332855));
#59778=CARTESIAN_POINT('Ctrl Pts',(11.7101248465183,14.3325674214145,17.2823211517672));
#59779=CARTESIAN_POINT('Ctrl Pts',(11.700195678653,14.3262661007535,17.2864153990732));
#59780=CARTESIAN_POINT('Ctrl Pts',(11.6812735959896,14.3191264193213,17.290180232345));
#59781=CARTESIAN_POINT('Ctrl Pts',(11.6731643433662,14.3172676724499,17.2907980108076));
#59782=CARTESIAN_POINT('Ctrl Pts',(11.6646867061662,14.3167989230148,17.2902231894927));
#59783=CARTESIAN_POINT('Ctrl Pts',(11.664681972407,14.3167986617141,17.2902228681585));
#59784=CARTESIAN_POINT('Ctrl Pts',(11.664677238709,14.316798400859,17.2902225464619));
#59785=CARTESIAN_POINT('Origin',(11.6285182850279,16.5579189812536,19.1088571563679));
#59786=CARTESIAN_POINT('Origin',(1.06052702375292,17.3704893936218,20.0466134020057));
#59787=CARTESIAN_POINT('Origin',(1.6653400148523,20.2416680737422,13.0085301837882));
#59788=CARTESIAN_POINT('',(1.95776807072638,17.9095502835289,12.0732632065885));
#59789=CARTESIAN_POINT('',(1.95776807072638,18.4221225649395,11.2756851683683));
#59790=CARTESIAN_POINT('Ctrl Pts',(1.95776807072638,17.9095502835289,12.0732632065885));
#59791=CARTESIAN_POINT('Ctrl Pts',(1.9513473618362,17.9090886249722,12.0729430865012));
#59792=CARTESIAN_POINT('Ctrl Pts',(1.94501567126187,17.9091896400968,12.0718023361232));
#59793=CARTESIAN_POINT('Ctrl Pts',(1.92948836979327,17.9107469050198,12.0670608355043));
#59794=CARTESIAN_POINT('Ctrl Pts',(1.92089186233992,17.9128121444813,12.062649573159));
#59795=CARTESIAN_POINT('Ctrl Pts',(1.90046800930197,17.919961362657,12.0488265486971));
#59796=CARTESIAN_POINT('Ctrl Pts',(1.88964186308624,17.9262218707066,12.0378146025024));
#59797=CARTESIAN_POINT('Ctrl Pts',(1.85810283833519,17.9494022586918,11.9982960736772));
#59798=CARTESIAN_POINT('Ctrl Pts',(1.84335629303728,17.9707651964678,11.9639355828322));
#59799=CARTESIAN_POINT('Ctrl Pts',(1.81854010589216,18.0131834276005,11.8961155639935));
#59800=CARTESIAN_POINT('Ctrl Pts',(1.80836917826496,18.0441097727155,11.847543312875));
#59801=CARTESIAN_POINT('Ctrl Pts',(1.79896764765298,18.0890437001662,11.7772259086882));
#59802=CARTESIAN_POINT('Ctrl Pts',(1.79670145400061,18.1049089522812,11.752458214319));
#59803=CARTESIAN_POINT('Ctrl Pts',(1.79434535609112,18.1320533589037,11.7101382365699));
#59804=CARTESIAN_POINT('Ctrl Pts',(1.79381557303812,18.1435051255807,11.6923016721812));
#59805=CARTESIAN_POINT('Ctrl Pts',(1.79365032105971,18.1660108445023,11.6572766007167));
#59806=CARTESIAN_POINT('Ctrl Pts',(1.79398945985933,18.1771515286776,11.6399523330915));
#59807=CARTESIAN_POINT('Ctrl Pts',(1.79575501944576,18.2026866914743,11.6002795066447));
#59808=CARTESIAN_POINT('Ctrl Pts',(1.79749007695644,18.2172256623124,11.5777166986477));
#59809=CARTESIAN_POINT('Ctrl Pts',(1.80455267776979,18.2573136245575,11.5156217429365));
#59810=CARTESIAN_POINT('Ctrl Pts',(1.81186451913778,18.2839135086097,11.4745394175059));
#59811=CARTESIAN_POINT('Ctrl Pts',(1.83578355228877,18.3383663258933,11.3913095468929));
#59812=CARTESIAN_POINT('Ctrl Pts',(1.85214505346194,18.362350282045,11.3552506393501));
#59813=CARTESIAN_POINT('Ctrl Pts',(1.88061329933071,18.3899158393675,11.3152721287423));
#59814=CARTESIAN_POINT('Ctrl Pts',(1.89448595076315,18.4013140249655,11.2990431881352));
#59815=CARTESIAN_POINT('Ctrl Pts',(1.92022261571902,18.4135454504488,11.2834023305783));
#59816=CARTESIAN_POINT('Ctrl Pts',(1.9286455870355,18.4166927832737,11.2796744022134));
#59817=CARTESIAN_POINT('Ctrl Pts',(1.94192278721223,18.4199459858402,11.2765856922883));
#59818=CARTESIAN_POINT('Ctrl Pts',(1.94616291414703,18.4207617450735,11.275963555897));
#59819=CARTESIAN_POINT('Ctrl Pts',(1.9529120729776,18.4216829443939,11.2755896143607));
#59820=CARTESIAN_POINT('Ctrl Pts',(1.9553390958748,18.4219398553151,11.2755766117231));
#59821=CARTESIAN_POINT('Ctrl Pts',(1.95776807072638,18.4221225649395,11.2756851683683));
#59822=CARTESIAN_POINT('',(1.65494820650842,18.8729868727,15.1358796271483));
#59823=CARTESIAN_POINT('Origin',(1.65494820650842,20.2405946732479,13.0078403511776));
#59824=CARTESIAN_POINT('',(1.36757616935991,19.0053968105924,14.8645808781538));
#59825=CARTESIAN_POINT('Origin',(1.6653400148523,19.0361537152975,14.8843471405862));
#59826=CARTESIAN_POINT('Origin',(1.36757616935991,20.2109111690372,12.9887639213558));
#59827=CARTESIAN_POINT('Origin',(1.65494820650842,20.2405946732479,13.0078403511776));
#59828=CARTESIAN_POINT('Origin',(6.4980472271939,20.7408526371047,13.3293366230661));
#59829=CARTESIAN_POINT('',(11.664677238709,18.6080860766515,12.5563388263038));
#59830=CARTESIAN_POINT('Ctrl Pts',(11.664677238709,18.6080860766515,12.5563388263039));
#59831=CARTESIAN_POINT('Ctrl Pts',(8.44760841234031,18.3763927057865,12.3965120461773));
#59832=CARTESIAN_POINT('Ctrl Pts',(5.17558411912346,18.1409160622912,12.2336952666484));
#59833=CARTESIAN_POINT('Ctrl Pts',(1.95776807072638,17.9095502835289,12.0732632065885));
#59834=CARTESIAN_POINT('',(11.3203626311916,19.6875065192443,16.0635678809207));
#59835=CARTESIAN_POINT('Origin',(11.3203626311916,21.2389637999728,13.6494532297333));
#59836=CARTESIAN_POINT('',(11.664677238709,19.1517258603906,11.7104188108481));
#59837=CARTESIAN_POINT('Origin',(11.3203626311916,21.2389637999728,13.6494532297333));
#59838=CARTESIAN_POINT('Ctrl Pts',(1.95776807072638,18.4221225649395,11.2756851683683));
#59839=CARTESIAN_POINT('Ctrl Pts',(5.17558411308691,18.6641695173893,11.4194969967751));
#59840=CARTESIAN_POINT('Ctrl Pts',(8.44760840593806,18.9100934023218,11.5660575512547));
#59841=CARTESIAN_POINT('Ctrl Pts',(11.664677238709,19.1517258603906,11.710418810848));
#59842=CARTESIAN_POINT('Origin',(11.3307544395355,21.2400372004671,13.6501430623439));
#59843=CARTESIAN_POINT('',(11.6285182850279,19.8814302665469,15.831801656791));
#59844=CARTESIAN_POINT('Origin',(11.6285182850279,21.2707941051722,13.6699093247763));
#59845=CARTESIAN_POINT('Origin',(11.3307544395355,19.8506733618418,15.8120353943587));
#59846=CARTESIAN_POINT('Ctrl Pts',(11.664677238709,19.1517258603906,11.710418810848));
#59847=CARTESIAN_POINT('Ctrl Pts',(11.6681719057553,19.151988343114,11.7105756289215));
#59848=CARTESIAN_POINT('Ctrl Pts',(11.6716519636862,19.1520868168133,11.7109982363921));
#59849=CARTESIAN_POINT('Ctrl Pts',(11.6751111337893,19.1520251848775,11.7116791242736));
#59850=CARTESIAN_POINT('Ctrl Pts',(11.6833639439589,19.1518781447924,11.713303571255));
#59851=CARTESIAN_POINT('Ctrl Pts',(11.6912209922801,19.1508231469805,11.7163463248885));
#59852=CARTESIAN_POINT('Ctrl Pts',(11.7092716451022,19.1466089777452,11.7262566703379));
#59853=CARTESIAN_POINT('Ctrl Pts',(11.7188321121789,19.142733229544,11.7341854248228));
#59854=CARTESIAN_POINT('Ctrl Pts',(11.7448362096952,19.1289260858262,11.7610385573625));
#59855=CARTESIAN_POINT('Ctrl Pts',(11.7582763496126,19.1162721838521,11.7838367770656));
#59856=CARTESIAN_POINT('Ctrl Pts',(11.7901173768954,19.0801695571631,11.8475823063438));
#59857=CARTESIAN_POINT('Ctrl Pts',(11.8074969006879,19.0448588947193,11.9072908240011));
#59858=CARTESIAN_POINT('Ctrl Pts',(11.8229354401012,18.9843724592575,12.0057954743111));
#59859=CARTESIAN_POINT('Ctrl Pts',(11.826199199177,18.9656295705593,12.0359174490527));
#59860=CARTESIAN_POINT('Ctrl Pts',(11.8295237141305,18.9348683931316,12.0847623667266));
#59861=CARTESIAN_POINT('Ctrl Pts',(11.8303434615844,18.9227524071091,12.103859132896));
#59862=CARTESIAN_POINT('Ctrl Pts',(11.8309946485842,18.8998942073469,12.139620835759));
#59863=CARTESIAN_POINT('Ctrl Pts',(11.8309459330901,18.8891042704865,12.1563957553283));
#59864=CARTESIAN_POINT('Ctrl Pts',(11.8300359252892,18.8655047903765,12.1928468152565));
#59865=CARTESIAN_POINT('Ctrl Pts',(11.8290394062419,18.8525739690576,12.2126713034689));
#59866=CARTESIAN_POINT('Ctrl Pts',(11.8249644421306,18.8184674171377,12.2645448124642));
#59867=CARTESIAN_POINT('Ctrl Pts',(11.8209395722477,18.7967229872269,12.2972023035393));
#59868=CARTESIAN_POINT('Ctrl Pts',(11.8028867656277,18.7307929414874,12.3947239887609));
#59869=CARTESIAN_POINT('Ctrl Pts',(11.7841990134601,18.6920888872387,12.4499140109568));
#59870=CARTESIAN_POINT('Ctrl Pts',(11.7507704380581,18.6519299935817,12.5046623381128));
#59871=CARTESIAN_POINT('Ctrl Pts',(11.7371459986443,18.6377168114473,12.5236992377786));
#59872=CARTESIAN_POINT('Ctrl Pts',(11.7101248465184,18.6209902609454,12.5443148471325));
#59873=CARTESIAN_POINT('Ctrl Pts',(11.700195678653,18.6160976708085,12.5500185358362));
#59874=CARTESIAN_POINT('Ctrl Pts',(11.6812735959896,18.6103078727442,12.5556423476123));
#59875=CARTESIAN_POINT('Ctrl Pts',(11.6731643433662,18.6086984664872,12.556758771215));
#59876=CARTESIAN_POINT('Ctrl Pts',(11.6646867061662,18.608086758819,12.5563392961791));
#59877=CARTESIAN_POINT('Ctrl Pts',(11.6646819724071,18.6080864175726,12.5563390614781));
#59878=CARTESIAN_POINT('Ctrl Pts',(11.664677238709,18.6080860766515,12.5563388263038));
#59879=CARTESIAN_POINT('Origin',(11.6285182850279,21.2707941051722,13.6699093247763));
#59880=CARTESIAN_POINT('Origin',(1.06052702375292,22.314646171184,14.3407523135387));
#59881=CARTESIAN_POINT('Origin',(1.6653400148523,23.0866647604201,6.77885640724594));
#59882=CARTESIAN_POINT('',(1.95776807072638,20.5855189702533,6.53850782206133));
#59883=CARTESIAN_POINT('',(1.95776807072638,20.8526247727479,5.62882899907204));
#59884=CARTESIAN_POINT('Ctrl Pts',(1.95776807072638,20.5855189702533,6.53850782206133));
#59885=CARTESIAN_POINT('Ctrl Pts',(1.9513480833199,20.58498588377,6.53833075323157));
#59886=CARTESIAN_POINT('Ctrl Pts',(1.94501708197863,20.5847614100627,6.53720798413881));
#59887=CARTESIAN_POINT('Ctrl Pts',(1.92954226703964,20.5849190653624,6.53223717834333));
#59888=CARTESIAN_POINT('Ctrl Pts',(1.9209894073484,20.5856501048189,6.52745980301691));
#59889=CARTESIAN_POINT('Ctrl Pts',(1.90083817145052,20.5885608974198,6.51243359052771));
#59890=CARTESIAN_POINT('Ctrl Pts',(1.89018614013953,20.5913816029711,6.50042022104901));
#59891=CARTESIAN_POINT('Ctrl Pts',(1.86077829279052,20.6015952674743,6.45943708811552));
#59892=CARTESIAN_POINT('Ctrl Pts',(1.84665745875882,20.611140107964,6.42475570918836));
#59893=CARTESIAN_POINT('Ctrl Pts',(1.82247517384536,20.6308899331518,6.35397716493558));
#59894=CARTESIAN_POINT('Ctrl Pts',(1.81230887643135,20.6450040326066,6.30493959671585));
#59895=CARTESIAN_POINT('Ctrl Pts',(1.79934881945864,20.6714274602751,6.21380591728078));
#59896=CARTESIAN_POINT('Ctrl Pts',(1.79572382774455,20.6848492864753,6.16787314051173));
#59897=CARTESIAN_POINT('Ctrl Pts',(1.79301769946659,20.7108870248761,6.07902063442843));
#59898=CARTESIAN_POINT('Ctrl Pts',(1.79378222861411,20.7240558919591,6.03421247801754));
#59899=CARTESIAN_POINT('Ctrl Pts',(1.7998218767273,20.7504816712267,5.94463801772135));
#59900=CARTESIAN_POINT('Ctrl Pts',(1.8054507297311,20.7644003702175,5.89763253003153));
#59901=CARTESIAN_POINT('Ctrl Pts',(1.82510992022202,20.7940525831188,5.79870751723029));
#59902=CARTESIAN_POINT('Ctrl Pts',(1.83960979646949,20.8080958899669,5.75272231990244));
#59903=CARTESIAN_POINT('Ctrl Pts',(1.86695154341265,20.8259464835343,5.69674419663866));
#59904=CARTESIAN_POINT('Ctrl Pts',(1.88252298601309,20.8347457609889,5.66966644865797));
#59905=CARTESIAN_POINT('Ctrl Pts',(1.91281431352699,20.8446460331123,5.64327836389123));
#59906=CARTESIAN_POINT('Ctrl Pts',(1.92253441500524,20.8472499388906,5.63690645398473));
#59907=CARTESIAN_POINT('Ctrl Pts',(1.93813933311943,20.8501988666455,5.63122599523098));
#59908=CARTESIAN_POINT('Ctrl Pts',(1.94311288783775,20.8509861372018,5.62997943255931));
#59909=CARTESIAN_POINT('Ctrl Pts',(1.95140011063542,20.8520210777582,5.6289276697355));
#59910=CARTESIAN_POINT('Ctrl Pts',(1.95458052113192,20.8523545794652,5.6287598616145));
#59911=CARTESIAN_POINT('Ctrl Pts',(1.95776807072638,20.8526247727479,5.62882899907202));
#59912=CARTESIAN_POINT('',(1.65494820650842,22.3727683628749,9.20563530484314));
#59913=CARTESIAN_POINT('Origin',(1.65494820650842,23.0854404918828,6.7784969295689));
#59914=CARTESIAN_POINT('',(1.36757616935991,22.4233810776973,8.90802187107886));
#59915=CARTESIAN_POINT('Origin',(1.6653400148523,22.4584609113062,8.9183222395943));
#59916=CARTESIAN_POINT('Origin',(1.36757616935991,23.0515849268112,6.7685560387305));
#59917=CARTESIAN_POINT('Origin',(1.65494820650842,23.0854404918828,6.7784969295689));
#59918=CARTESIAN_POINT('Origin',(6.4980472271939,23.6560104598922,6.94603138825146));
#59919=CARTESIAN_POINT('',(11.664677238709,21.3918572850628,6.805215209861));
#59920=CARTESIAN_POINT('Ctrl Pts',(11.664677238709,21.3918572850628,6.805215209861));
#59921=CARTESIAN_POINT('Ctrl Pts',(8.45037669575292,21.1247507590271,6.71721389334346));
#59922=CARTESIAN_POINT('Ctrl Pts',(5.17722936343352,20.8528483573768,6.62730336128235));
#59923=CARTESIAN_POINT('Ctrl Pts',(1.95776807072638,20.5855189702533,6.53850782206133));
#59924=CARTESIAN_POINT('',(11.3203626311916,23.4156542242922,9.86626896342395));
#59925=CARTESIAN_POINT('Origin',(11.3203626311916,24.2241318908269,7.11284689157994));
#59926=CARTESIAN_POINT('',(11.664677238709,21.6751526289,5.84039987251778));
#59927=CARTESIAN_POINT('Origin',(11.3203626311916,24.2241318908269,7.11284689157994));
#59928=CARTESIAN_POINT('Ctrl Pts',(1.95776807072638,20.8526247727479,5.62882899907203));
#59929=CARTESIAN_POINT('Ctrl Pts',(5.17722935754855,21.1255230565072,5.69865861625942));
#59930=CARTESIAN_POINT('Ctrl Pts',(8.45037668926196,21.4028712159812,5.77002260020614));
#59931=CARTESIAN_POINT('Ctrl Pts',(11.664677238709,21.6751526289,5.84039987251777));
#59932=CARTESIAN_POINT('Origin',(11.3307544395355,24.2253561593642,7.11320636925698));
#59933=CARTESIAN_POINT('',(11.6285182850279,23.5364266063324,9.58925626669054));
#59934=CARTESIAN_POINT('Origin',(11.6285182850279,24.2604359929731,7.12350673777241));
#59935=CARTESIAN_POINT('Origin',(11.3307544395355,23.5013467727236,9.57895589817511));
#59936=CARTESIAN_POINT('Ctrl Pts',(11.664677238709,21.6751526289,5.84039987251778));
#59937=CARTESIAN_POINT('Ctrl Pts',(11.6681756837601,21.6754489800181,5.84047647114826));
#59938=CARTESIAN_POINT('Ctrl Pts',(11.6716557442405,21.6756623521125,5.84085486706167));
#59939=CARTESIAN_POINT('Ctrl Pts',(11.6751111337893,21.6757948999659,5.84152480494111));
#59940=CARTESIAN_POINT('Ctrl Pts',(11.6834492137325,21.6761147465654,5.84314140866026));
#59941=CARTESIAN_POINT('Ctrl Pts',(11.6912528317941,21.6759503372767,5.84637491140685));
#59942=CARTESIAN_POINT('Ctrl Pts',(11.7091239528621,21.6747209936006,5.85692922382961));
#59943=CARTESIAN_POINT('Ctrl Pts',(11.718489115776,21.6732669685549,5.86544860786681));
#59944=CARTESIAN_POINT('Ctrl Pts',(11.7423632180108,21.6681303692968,5.89238136827878));
#59945=CARTESIAN_POINT('Ctrl Pts',(11.7550185107735,21.6632424395397,5.91454378047491));
#59946=CARTESIAN_POINT('Ctrl Pts',(11.782945606649,21.6493229837906,5.97457704224723));
#59947=CARTESIAN_POINT('Ctrl Pts',(11.7977324484725,21.637177726309,6.02338974579153));
#59948=CARTESIAN_POINT('Ctrl Pts',(11.8194386441993,21.6078719961958,6.13462845786581));
#59949=CARTESIAN_POINT('Ctrl Pts',(11.825673894872,21.5920955534044,6.19191044279121));
#59950=CARTESIAN_POINT('Ctrl Pts',(11.8317749863308,21.5603242616104,6.30356890402402));
#59951=CARTESIAN_POINT('Ctrl Pts',(11.8316012176116,21.5432716658125,6.36154350871869));
#59952=CARTESIAN_POINT('Ctrl Pts',(11.824941361477,21.50960504634,6.47243556191222));
#59953=CARTESIAN_POINT('Ctrl Pts',(11.8183083548574,21.4918876839749,6.529013179409));
#59954=CARTESIAN_POINT('Ctrl Pts',(11.795821624489,21.4564286561113,6.637989474794));
#59955=CARTESIAN_POINT('Ctrl Pts',(11.7805655796944,21.4404704012147,6.68472301424652));
#59956=CARTESIAN_POINT('Ctrl Pts',(11.7536264417725,21.4211446949061,6.73846169515414));
#59957=CARTESIAN_POINT('Ctrl Pts',(11.7402881749119,21.412752167224,6.76120915401804));
#59958=CARTESIAN_POINT('Ctrl Pts',(11.7136982696185,21.4020408829817,6.78732748838213));
#59959=CARTESIAN_POINT('Ctrl Pts',(11.7035133274598,21.398679437698,6.79496994538257));
#59960=CARTESIAN_POINT('Ctrl Pts',(11.6842762528669,21.3943170183099,6.80313984330724));
#59961=CARTESIAN_POINT('Ctrl Pts',(11.6760378533014,21.3929463221456,6.80507051068837));
#59962=CARTESIAN_POINT('Ctrl Pts',(11.6665534479108,21.3920199943286,6.80524520977619));
#59963=CARTESIAN_POINT('Ctrl Pts',(11.6656136423373,21.3919350996656,6.80524084677671));
#59964=CARTESIAN_POINT('Ctrl Pts',(11.664677238709,21.3918572850628,6.805215209861));
#59965=CARTESIAN_POINT('Origin',(11.6285182850279,24.2604359929731,7.12350673777241));
#59966=CARTESIAN_POINT('Origin',(1.06052702375292,25.4510030262676,7.47308876036672));
#59967=CARTESIAN_POINT('Origin',(1.6653400148523,24.0613171698908,0.));
#59968=CARTESIAN_POINT('',(1.95776807072638,21.593771336803,0.47404141979407));
#59969=CARTESIAN_POINT('',(1.95776807072638,21.593771336803,-0.47404141979407));
#59970=CARTESIAN_POINT('Ctrl Pts',(1.95776807072638,21.593771336803,0.47404141979407));
#59971=CARTESIAN_POINT('Ctrl Pts',(1.9513477680545,21.5932099304462,0.474021710346213));
#59972=CARTESIAN_POINT('Ctrl Pts',(1.94501646552415,21.5926782047131,0.473007564236366));
#59973=CARTESIAN_POINT('Ctrl Pts',(1.92951932707503,21.591427238987,0.468186519780974));
#59974=CARTESIAN_POINT('Ctrl Pts',(1.92094790453061,21.5907814463352,0.463380674959194));
#59975=CARTESIAN_POINT('Ctrl Pts',(1.90068428386471,21.5893333422069,0.448036950371891));
#59976=CARTESIAN_POINT('Ctrl Pts',(1.88996070920461,21.5886516447309,0.435581293464837));
#59977=CARTESIAN_POINT('Ctrl Pts',(1.85988430203394,21.5868688155781,0.392217225062086));
#59978=CARTESIAN_POINT('Ctrl Pts',(1.84552319454968,21.5862561010085,0.354793494140223));
#59979=CARTESIAN_POINT('Ctrl Pts',(1.82174065150271,21.5852941592389,0.280937783836869));
#59980=CARTESIAN_POINT('Ctrl Pts',(1.81181923278667,21.585029713215,0.230359404109805));
#59981=CARTESIAN_POINT('Ctrl Pts',(1.79996844463622,21.5847372703622,0.1421502207605));
#59982=CARTESIAN_POINT('Ctrl Pts',(1.79660846342306,21.5846751446254,0.101128548750127));
#59983=CARTESIAN_POINT('Ctrl Pts',(1.79344073698656,21.5846159222426,0.0237247600543095));
#59984=CARTESIAN_POINT('Ctrl Pts',(1.79332003639192,21.5846139884599,-0.0138289841184048));
#59985=CARTESIAN_POINT('Ctrl Pts',(1.79594647664003,21.5846625069698,-0.0907225510804983));
#59986=CARTESIAN_POINT('Ctrl Pts',(1.79895084940664,21.5847168190493,-0.131181998465391));
#59987=CARTESIAN_POINT('Ctrl Pts',(1.80977106001214,21.5849749085674,-0.218244549032268));
#59988=CARTESIAN_POINT('Ctrl Pts',(1.81886112579735,21.5852081198308,-0.267828304153497));
#59989=CARTESIAN_POINT('Ctrl Pts',(1.84164209107167,21.5860852333224,-0.344658261472531));
#59990=CARTESIAN_POINT('Ctrl Pts',(1.85799718988476,21.586731148623,-0.39111526813368));
#59991=CARTESIAN_POINT('Ctrl Pts',(1.89263444116559,21.588821021946,-0.438752720199368));
#59992=CARTESIAN_POINT('Ctrl Pts',(1.90520057316188,21.5896217948898,-0.453157912546355));
#59993=CARTESIAN_POINT('Ctrl Pts',(1.92760472466551,21.5912873878866,-0.466915949380981));
#59994=CARTESIAN_POINT('Ctrl Pts',(1.9346104038645,21.591831536706,-0.470078655940862));
#59995=CARTESIAN_POINT('Ctrl Pts',(1.94721684091347,21.5928636195227,-0.473331333007928));
#59996=CARTESIAN_POINT('Ctrl Pts',(1.95246882049205,21.5933079579064,-0.474025151823304));
#59997=CARTESIAN_POINT('Ctrl Pts',(1.95776807072638,21.593771336803,-0.47404141979407));
#59998=CARTESIAN_POINT('',(1.65494820650842,24.0600412162663,2.52960515816076));
#59999=CARTESIAN_POINT('Origin',(1.65494820650842,24.0600412162663,-1.54893643002411E-16));
#60000=CARTESIAN_POINT('',(1.36757616935991,24.0247563668693,2.22978791005503));
#60001=CARTESIAN_POINT('Origin',(1.6653400148523,24.0613171698908,2.22978791005503));
#60002=CARTESIAN_POINT('Origin',(1.36757616935991,24.0247563668693,0.));
#60003=CARTESIAN_POINT('Origin',(1.65494820650842,24.0600412162663,-1.54893643002411E-16));
#60004=CARTESIAN_POINT('Origin',(6.4980472271939,24.6546990029305,0.));
#60005=CARTESIAN_POINT('',(11.664677238709,22.4425874385122,0.502773529288439));
#60006=CARTESIAN_POINT('Ctrl Pts',(11.664677238709,22.4425874385122,0.502773529288439));
#60007=CARTESIAN_POINT('Ctrl Pts',(8.45174540654375,22.1616274567787,0.493593399690554));
#60008=CARTESIAN_POINT('Ctrl Pts',(5.17782841008702,21.875340981737,0.48392656300278));
#60009=CARTESIAN_POINT('Ctrl Pts',(1.95776807072638,21.593771336803,0.474041419794075));
#60010=CARTESIAN_POINT('',(11.3203626311916,25.2468048823457,2.8696636114714));
#60011=CARTESIAN_POINT('Origin',(11.3203626311916,25.2468048823457,-1.75716217820904E-16));
#60012=CARTESIAN_POINT('',(11.664677238709,22.4425874385122,-0.50277352928844));
#60013=CARTESIAN_POINT('Origin',(11.3203626311916,25.2468048823457,-1.75716217820904E-16));
#60014=CARTESIAN_POINT('Ctrl Pts',(1.95776807072638,21.593771336803,-0.474041419794078));
#60015=CARTESIAN_POINT('Ctrl Pts',(5.17782840427536,21.8753409812288,-0.483926562984941));
#60016=CARTESIAN_POINT('Ctrl Pts',(8.4517454000289,22.161627456209,-0.493593399671942));
#60017=CARTESIAN_POINT('Ctrl Pts',(11.664677238709,22.4425874385122,-0.502773529288442));
#60018=CARTESIAN_POINT('Origin',(11.3307544395355,25.2480808359702,0.));
#60019=CARTESIAN_POINT('',(11.6285182850279,25.2846416389917,2.56984636336567));
#60020=CARTESIAN_POINT('Origin',(11.6285182850279,25.2846416389917,0.));
#60021=CARTESIAN_POINT('Origin',(11.3307544395355,25.2480808359702,2.56984636336567));
#60022=CARTESIAN_POINT('Ctrl Pts',(11.664677238709,22.4425874385122,-0.502773529288416));
#60023=CARTESIAN_POINT('Ctrl Pts',(11.6681753033367,22.4428933323889,-0.50278352411193));
#60024=CARTESIAN_POINT('Ctrl Pts',(11.6716553635686,22.4432046663249,-0.502480637546283));
#60025=CARTESIAN_POINT('Ctrl Pts',(11.6751111337893,22.4435206231749,-0.501875113202017));
#60026=CARTESIAN_POINT('Ctrl Pts',(11.6835623119454,22.4442933040705,-0.500394287283524));
#60027=CARTESIAN_POINT('Ctrl Pts',(11.691384091347,22.4450491314624,-0.497199786883766));
#60028=CARTESIAN_POINT('Ctrl Pts',(11.7094694893508,22.4468652011622,-0.486572040199507));
#60029=CARTESIAN_POINT('Ctrl Pts',(11.7189285997146,22.4478827563863,-0.47778287580148));
#60030=CARTESIAN_POINT('Ctrl Pts',(11.7437048785723,22.4506469894916,-0.449218987208357));
#60031=CARTESIAN_POINT('Ctrl Pts',(11.7567586963551,22.4522625711256,-0.425077089679939));
#60032=CARTESIAN_POINT('Ctrl Pts',(11.7862943788244,22.4560498423181,-0.357948221183821));
#60033=CARTESIAN_POINT('Ctrl Pts',(11.8016138506642,22.4582634908384,-0.301713314632985));
#60034=CARTESIAN_POINT('Ctrl Pts',(11.8195646608092,22.4609621241242,-0.195134214413052));
#60035=CARTESIAN_POINT('Ctrl Pts',(11.8242738201003,22.4617066134238,-0.151903163592294));
#60036=CARTESIAN_POINT('Ctrl Pts',(11.8295027526625,22.4625362310301,-0.0759831017663084));
#60037=CARTESIAN_POINT('Ctrl Pts',(11.830683585196,22.4627272832912,-0.0420217792038241));
#60038=CARTESIAN_POINT('Ctrl Pts',(11.8310447700704,22.46278539012,0.0250506013991047));
#60039=CARTESIAN_POINT('Ctrl Pts',(11.8301786225274,22.4626451514276,0.0587303495792302));
#60040=CARTESIAN_POINT('Ctrl Pts',(11.825990760224,22.4619778159673,0.132571716988474));
#60041=CARTESIAN_POINT('Ctrl Pts',(11.8220311067205,22.4613492475643,0.173539728186971));
#60042=CARTESIAN_POINT('Ctrl Pts',(11.8081497193984,22.4592328861399,0.268683426062675));
#60043=CARTESIAN_POINT('Ctrl Pts',(11.7954615897779,22.4573293352261,0.327557844264918));
#60044=CARTESIAN_POINT('Ctrl Pts',(11.7672407996649,22.4535873444032,0.403094447780868));
#60045=CARTESIAN_POINT('Ctrl Pts',(11.7555857098412,22.4520974558946,0.428285481038826));
#60046=CARTESIAN_POINT('Ctrl Pts',(11.7315700529649,22.4492776427903,0.46416117518514));
#60047=CARTESIAN_POINT('Ctrl Pts',(11.7196350773267,22.4479351247539,0.478241088357696));
#60048=CARTESIAN_POINT('Ctrl Pts',(11.6975720132429,22.4456574568071,0.494192277150456));
#60049=CARTESIAN_POINT('Ctrl Pts',(11.6885594272653,22.4447671654469,0.498754860639004));
#60050=CARTESIAN_POINT('Ctrl Pts',(11.6741930061583,22.4434324790847,0.502225072627091));
#60051=CARTESIAN_POINT('Ctrl Pts',(11.6694225684331,22.4430024014875,0.502787087852409));
#60052=CARTESIAN_POINT('Ctrl Pts',(11.664677238709,22.4425874385122,0.502773529288416));
#60053=CARTESIAN_POINT('Origin',(11.6285182850279,25.2846416389917,0.));
#60054=CARTESIAN_POINT('Origin',(1.06052702375292,26.5254709791062,0.));
#60055=CARTESIAN_POINT('Origin',(-0.688999999999999,0.,0.));
#60056=CARTESIAN_POINT('',(-0.888999999999999,-22.3743990607509,-2.74007361925941E-15));
#60057=CARTESIAN_POINT('',(-0.688999999999999,-22.5743990607509,-2.76456655524236E-15));
#60058=CARTESIAN_POINT('Origin',(-0.888999999999999,0.,0.));
#60059=CARTESIAN_POINT('Origin',(6.67356988158431,0.,0.));
#60060=CARTESIAN_POINT('',(6.67356988158431,-22.011553150687,-2.69563781102507E-15));
#60061=CARTESIAN_POINT('',(6.67356988158431,-22.011553150687,-2.69563781102507E-15));
#60062=CARTESIAN_POINT('Origin',(15.625,0.,0.));
#60063=CARTESIAN_POINT('',(15.875,-25.3846416389917,-3.10872201306938E-15));
#60064=CARTESIAN_POINT('Origin',(15.875,0.,0.));
#60065=CARTESIAN_POINT('',(15.625,-25.6346416389917,-3.13933818304807E-15));
#60066=CARTESIAN_POINT('Origin',(15.875,18.294,0.));
#60067=CARTESIAN_POINT('',(15.875,-18.294,-2.24036885436017E-15));
#60068=CARTESIAN_POINT('Origin',(15.875,0.,0.));
#60069=CARTESIAN_POINT('Origin',(15.475,0.,0.));
#60070=CARTESIAN_POINT('',(15.075,-17.494,-2.14239711042838E-15));
#60071=CARTESIAN_POINT('',(15.475,-17.894,-2.19138298239427E-15));
#60072=CARTESIAN_POINT('Origin',(15.075,0.,0.));
#60073=CARTESIAN_POINT('Origin',(7.393,0.,0.));
#60074=CARTESIAN_POINT('',(-0.288999999999999,-17.494,-2.14239711042838E-15));
#60075=CARTESIAN_POINT('',(7.393,-17.494,-2.14239711042838E-15));
#60076=CARTESIAN_POINT('Origin',(-0.288999999999999,0.,0.));
#60077=CARTESIAN_POINT('Origin',(-0.588999999999999,0.,0.));
#60078=CARTESIAN_POINT('',(-0.889,-18.094,-2.21587591837722E-15));
#60079=CARTESIAN_POINT('',(-0.588999999999999,-17.794,-2.1791365144028E-15));
#60080=CARTESIAN_POINT('Origin',(-0.888999999999999,0.,0.));
#60081=CARTESIAN_POINT('Origin',(-0.888999999999999,22.3743990607509,0.));
#60082=CARTESIAN_POINT('',(0.,0.,0.));
#60083=CARTESIAN_POINT('Origin',(0.4,0.,0.));
#60084=CARTESIAN_POINT('',(0.8,-25.146,-3.07949684113593E-15));
#60085=CARTESIAN_POINT('Origin',(0.8,0.,0.));
#60086=CARTESIAN_POINT('',(-4.85722573273506E-16,-24.346,-2.98152509720415E-15));
#60087=CARTESIAN_POINT('',(0.4,-24.746,-3.03051096917004E-15));
#60088=CARTESIAN_POINT('Origin',(0.,0.,0.));
#60089=CARTESIAN_POINT('Origin',(5.434,0.,0.));
#60090=CARTESIAN_POINT('',(10.068,-25.146,-3.07949684113593E-15));
#60091=CARTESIAN_POINT('Origin',(10.068,0.,0.));
#60092=CARTESIAN_POINT('',(5.434,-25.146,-3.07949684113593E-15));
#60093=CARTESIAN_POINT('Origin',(10.368,0.,0.));
#60094=CARTESIAN_POINT('',(10.668,-24.546,-3.00601803318709E-15));
#60095=CARTESIAN_POINT('Origin',(10.668,0.,0.));
#60096=CARTESIAN_POINT('',(10.368,-24.846,-3.04275743716151E-15));
#60097=CARTESIAN_POINT('Origin',(10.668,24.0881298772848,0.));
#60098=CARTESIAN_POINT('',(10.668,-24.0881298772848,-2.94994511516625E-15));
#60099=CARTESIAN_POINT('Origin',(10.668,0.,0.));
#60100=CARTESIAN_POINT('Origin',(10.518,0.,0.));
#60101=CARTESIAN_POINT('',(10.368,-23.7881298772848,-2.91320571119183E-15));
#60102=CARTESIAN_POINT('',(10.518,-23.9381298772848,-2.93157541317904E-15));
#60103=CARTESIAN_POINT('Origin',(10.368,0.,0.));
#60104=CARTESIAN_POINT('Origin',(5.434,0.,0.));
#60105=CARTESIAN_POINT('',(0.5,-22.2251922201623,-2.72180105128564E-15));
#60106=CARTESIAN_POINT('',(5.434,-23.0066610487235,-2.81750338123874E-15));
#60107=CARTESIAN_POINT('Origin',(0.5,0.,0.));
#60108=CARTESIAN_POINT('Origin',(0.25,0.,0.));
#60109=CARTESIAN_POINT('',(6.24500451351651E-16,-22.646,-2.7733351413491E-15));
#60110=CARTESIAN_POINT('',(0.25,-22.4355961100811,-2.74756809631737E-15));
#60111=CARTESIAN_POINT('Origin',(0.,0.,0.));
#60112=CARTESIAN_POINT('Origin',(0.,24.346,0.));
#60113=CARTESIAN_POINT('',(0.,0.,0.));
#60114=CARTESIAN_POINT('Origin',(11.0628466354112,0.,0.));
#60115=CARTESIAN_POINT('',(11.3128466354112,21.6856897166516,-2.65573104988001E-15));
#60116=CARTESIAN_POINT('',(11.3128466354112,-21.6856897166516,-2.65573104988001E-15));
#60117=CARTESIAN_POINT('Origin',(11.3128466354112,0.,0.));
#60118=CARTESIAN_POINT('Origin',(11.3128466354112,0.,0.));
#60119=CARTESIAN_POINT('',(10.8128466354112,21.1856897166516,2.59449870992264E-15));
#60120=CARTESIAN_POINT('',(11.0628466354112,21.4356897166516,2.62511487990132E-15));
#60121=CARTESIAN_POINT('Origin',(10.8128466354112,0.,0.));
#60122=CARTESIAN_POINT('Origin',(10.8128466354112,21.6856897166516,0.));
#60123=CARTESIAN_POINT('',(10.8128466354112,-18.5104574586244,-2.26687724774576E-15));
#60124=CARTESIAN_POINT('Origin',(10.8128466354112,0.,0.));
#60125=CARTESIAN_POINT('Origin',(12.2684233177056,0.,0.));
#60126=CARTESIAN_POINT('',(13.724,-21.6856897166516,-2.65573104988001E-15));
#60127=CARTESIAN_POINT('Origin',(13.724,0.,0.));
#60128=CARTESIAN_POINT('',(12.2684233177056,-21.6856897166516,-2.65573104988001E-15));
#60129=CARTESIAN_POINT('Origin',(0.938469106971115,0.,0.));
#60130=CARTESIAN_POINT('',(1.18846910697111,18.318471118769,-2.24336570208737E-15));
#60131=CARTESIAN_POINT('Origin',(1.18846910697111,0.,0.));
#60132=CARTESIAN_POINT('',(0.688469106971115,18.818471118769,2.30459804204474E-15));
#60133=CARTESIAN_POINT('',(0.938469106971115,18.568471118769,2.27398187206606E-15));
#60134=CARTESIAN_POINT('',(0.688469106971115,-18.818471118769,-2.30459804204474E-15));
#60135=CARTESIAN_POINT('Origin',(0.688469106971115,0.,0.));
#60136=CARTESIAN_POINT('Origin',(0.688469106971115,0.,0.));
#60137=CARTESIAN_POINT('Origin',(0.540234553485558,0.,0.));
#60138=CARTESIAN_POINT('',(-0.107999999999999,-18.818471118769,-2.30459804204474E-15));
#60139=CARTESIAN_POINT('',(0.540234553485558,-18.818471118769,-2.30459804204474E-15));
#60140=CARTESIAN_POINT('Origin',(-0.107999999999999,0.,0.));
#60141=CARTESIAN_POINT('Origin',(1.18846910697111,17.6684335313922,0.));
#60142=CARTESIAN_POINT('',(1.18846910697112,-17.6684335313922,-2.16375905701672E-15));
#60143=CARTESIAN_POINT('Origin',(1.18846910697111,0.,0.));
#60144=CARTESIAN_POINT('Origin',(1.63623295246351,19.0374307818588,-6.18563622669654));
#60145=CARTESIAN_POINT('',(1.90706327644678,16.998194874094,-5.04583540480242));
#60146=CARTESIAN_POINT('',(1.90706327644678,16.7176961632773,-5.90912166928202));
#60147=CARTESIAN_POINT('Ctrl Pts',(1.90706327644678,16.998194874094,-5.04583540480242));
#60148=CARTESIAN_POINT('Ctrl Pts',(1.90026014386187,16.9976225239768,-5.04567196333261));
#60149=CARTESIAN_POINT('Ctrl Pts',(1.89355517771136,16.9967539080906,-5.04653705369465));
#60150=CARTESIAN_POINT('Ctrl Pts',(1.87732280058894,16.9939422782635,-5.05101511023725));
#60151=CARTESIAN_POINT('Ctrl Pts',(1.86840987580573,16.9917638647486,-5.05560766488548));
#60152=CARTESIAN_POINT('Ctrl Pts',(1.84749974153913,16.9854633184885,-5.0703493038951));
#60153=CARTESIAN_POINT('Ctrl Pts',(1.83650132566886,16.9808716613314,-5.08235904211517));
#60154=CARTESIAN_POINT('Ctrl Pts',(1.81085694927963,16.9680241697425,-5.11736200897173));
#60155=CARTESIAN_POINT('Ctrl Pts',(1.79594323550036,16.9576102181456,-5.14737025660481));
#60156=CARTESIAN_POINT('Ctrl Pts',(1.76902539468004,16.930787168517,-5.2269875316408));
#60157=CARTESIAN_POINT('Ctrl Pts',(1.75949337448525,16.9155448309939,-5.27332224829203));
#60158=CARTESIAN_POINT('Ctrl Pts',(1.74741836256345,16.8870291804687,-5.36043234407666));
#60159=CARTESIAN_POINT('Ctrl Pts',(1.74418490387259,16.8726745751484,-5.40452184220164));
#60160=CARTESIAN_POINT('Ctrl Pts',(1.74230474178714,16.8447903345401,-5.49027879637633));
#60161=CARTESIAN_POINT('Ctrl Pts',(1.74356051202805,16.8306696144894,-5.53376566270212));
#60162=CARTESIAN_POINT('Ctrl Pts',(1.75089245923172,16.8026196377593,-5.62039732387137));
#60163=CARTESIAN_POINT('Ctrl Pts',(1.75736442403687,16.7879279245149,-5.66589231855628));
#60164=CARTESIAN_POINT('Ctrl Pts',(1.7794814507125,16.7577464575537,-5.76057523482478));
#60165=CARTESIAN_POINT('Ctrl Pts',(1.79536357091901,16.7443881182364,-5.80338352889019));
#60166=CARTESIAN_POINT('Ctrl Pts',(1.82385809603019,16.7297952066032,-5.85279728585448));
#60167=CARTESIAN_POINT('Ctrl Pts',(1.83844662203883,16.7236372532306,-5.87421791437456));
#60168=CARTESIAN_POINT('Ctrl Pts',(1.86612294570743,16.71853113804,-5.89600163036399));
#60169=CARTESIAN_POINT('Ctrl Pts',(1.87511027899095,16.7174688556406,-5.90137286939842));
#60170=CARTESIAN_POINT('Ctrl Pts',(1.88937385987909,16.7169970261612,-5.906455483394));
#60171=CARTESIAN_POINT('Ctrl Pts',(1.89395673353014,16.7170046598605,-5.90763715542277));
#60172=CARTESIAN_POINT('Ctrl Pts',(1.90144341423147,16.7172952459802,-5.90878057607792));
#60173=CARTESIAN_POINT('Ctrl Pts',(1.9042514539434,16.7174650761224,-5.90903727408001));
#60174=CARTESIAN_POINT('Ctrl Pts',(1.90706327644678,16.7176961632773,-5.90912166928202));
#60175=CARTESIAN_POINT('',(1.62584114411962,19.7629572175357,-3.94856638716317));
#60176=CARTESIAN_POINT('Origin',(1.62584114411962,19.0362172778497,-6.18524193534254));
#60177=CARTESIAN_POINT('',(1.33846910697111,19.6367507067188,-4.22280591656416));
#60178=CARTESIAN_POINT('Origin',(1.63623295246351,19.6715220966734,-4.23410382602581));
#60179=CARTESIAN_POINT('Origin',(1.33846910697111,19.0026593919041,-6.17433831723489));
#60180=CARTESIAN_POINT('Origin',(1.62584114411962,19.0362172778497,-6.18524193534254));
#60181=CARTESIAN_POINT('Origin',(5.83867335851287,19.5281709987517,-6.34508738889866));
#60182=CARTESIAN_POINT('',(10.3480326234796,17.7080825054385,-5.24947731735613));
#60183=CARTESIAN_POINT('Ctrl Pts',(10.3480326234796,17.7080825054385,-5.24947731735613));
#60184=CARTESIAN_POINT('Ctrl Pts',(7.54972025675579,17.4728227255228,-5.18170180546196));
#60185=CARTESIAN_POINT('Ctrl Pts',(4.7091881268347,17.233938697471,-5.11315489305578));
#60186=CARTESIAN_POINT('Ctrl Pts',(1.90706327644677,16.998194874094,-5.04583540480243));
#60187=CARTESIAN_POINT('',(10.0307219562183,20.8358167812138,-3.98623266785661));
#60188=CARTESIAN_POINT('Origin',(10.0307219562183,20.0176977116355,-6.50414425974677));
#60189=CARTESIAN_POINT('',(10.3480326234796,17.4117050340792,-6.16163338174817));
#60190=CARTESIAN_POINT('Origin',(10.0307219562183,20.0176977116355,-6.50414425974677));
#60191=CARTESIAN_POINT('Ctrl Pts',(1.90706327644678,16.7176961632773,-5.90912166928202));
#60192=CARTESIAN_POINT('Ctrl Pts',(4.70918812184411,16.9479863246852,-5.99322580178265));
#60193=CARTESIAN_POINT('Ctrl Pts',(7.54972025123709,17.1815384272226,-6.07818269341643));
#60194=CARTESIAN_POINT('Ctrl Pts',(10.3480326234796,17.4117050340792,-6.16163338174817));
#60195=CARTESIAN_POINT('Origin',(10.0411137645622,20.0189112156446,-6.50453855110077));
#60196=CARTESIAN_POINT('',(10.3388776100546,20.7791530503061,-4.28306801618089));
#60197=CARTESIAN_POINT('Origin',(10.3388776100546,20.0536826055992,-6.51583646056242));
#60198=CARTESIAN_POINT('Origin',(10.0411137645622,20.7443816603515,-4.27177010671924));
#60199=CARTESIAN_POINT('Ctrl Pts',(10.3480326234796,17.4117050340792,-6.16163338174817));
#60200=CARTESIAN_POINT('Ctrl Pts',(10.3515114639741,17.4119911754408,-6.16173712700433));
#60201=CARTESIAN_POINT('Ctrl Pts',(10.3549914179992,17.4123759675224,-6.16156241574048));
#60202=CARTESIAN_POINT('Ctrl Pts',(10.3584662558372,17.4128588642783,-6.1611090307738));
#60203=CARTESIAN_POINT('Ctrl Pts',(10.367223098271,17.4140757989961,-6.15996646789746));
#60204=CARTESIAN_POINT('Ctrl Pts',(10.3753630700178,17.4158312902421,-6.15713972282255));
#60205=CARTESIAN_POINT('Ctrl Pts',(10.3939290316259,17.4209477623239,-6.14753302482073));
#60206=CARTESIAN_POINT('Ctrl Pts',(10.4035780672154,17.4246680145472,-6.13952487259418));
#60207=CARTESIAN_POINT('Ctrl Pts',(10.4280013399752,17.435881088904,-6.11408837463523));
#60208=CARTESIAN_POINT('Ctrl Pts',(10.4407678160189,17.4444479537232,-6.09300205845743));
#60209=CARTESIAN_POINT('Ctrl Pts',(10.4685456259698,17.4667636690831,-6.03626400623244));
#60210=CARTESIAN_POINT('Ctrl Pts',(10.4828713837317,17.483834507896,-5.99063505235319));
#60211=CARTESIAN_POINT('Ctrl Pts',(10.5038238234649,17.5210208246161,-5.8867407161014));
#60212=CARTESIAN_POINT('Ctrl Pts',(10.5097149363751,17.5396167538765,-5.83272996465078));
#60213=CARTESIAN_POINT('Ctrl Pts',(10.5152093525458,17.5750286675881,-5.72672134143427));
#60214=CARTESIAN_POINT('Ctrl Pts',(10.5146501294348,17.5929043782428,-5.67139291388385));
#60215=CARTESIAN_POINT('Ctrl Pts',(10.5071723447785,17.6260374509827,-5.56539053344037));
#60216=CARTESIAN_POINT('Ctrl Pts',(10.5000174147823,17.6424047527202,-5.51115999516815));
#60217=CARTESIAN_POINT('Ctrl Pts',(10.4763655908937,17.6725219279294,-5.40677101623398));
#60218=CARTESIAN_POINT('Ctrl Pts',(10.4605419031701,17.6845328147317,-5.36240927189436));
#60219=CARTESIAN_POINT('Ctrl Pts',(10.4319469960435,17.6978522663517,-5.30950538071607));
#60220=CARTESIAN_POINT('Ctrl Pts',(10.4192298015583,17.7023303304535,-5.29065702126867));
#60221=CARTESIAN_POINT('Ctrl Pts',(10.3949786188434,17.7070402629162,-5.26742227944471));
#60222=CARTESIAN_POINT('Ctrl Pts',(10.3846960006404,17.708325726784,-5.25993527526374));
#60223=CARTESIAN_POINT('Ctrl Pts',(10.3651744504235,17.7090036066899,-5.2516475721963));
#60224=CARTESIAN_POINT('Ctrl Pts',(10.3566858346072,17.708809998398,-5.2496868993244));
#60225=CARTESIAN_POINT('Ctrl Pts',(10.3480326234796,17.7080825054385,-5.24947731735612));
#60226=CARTESIAN_POINT('Origin',(10.3388776100546,20.0536826055992,-6.51583646056242));
#60227=CARTESIAN_POINT('Origin',(1.05309141530195,21.2131190072776,-6.89256018399714));
#60228=CARTESIAN_POINT('Origin',(1.63623295246351,16.1942058835342,-11.7657792816622));
#60229=CARTESIAN_POINT('',(1.90706327644678,14.6069951093592,-10.0516057316823));
#60230=CARTESIAN_POINT('',(1.90706327644678,14.0734548558899,-10.7859608904011));
#60231=CARTESIAN_POINT('Ctrl Pts',(1.90706327644678,14.6069951093592,-10.0516057316823));
#60232=CARTESIAN_POINT('Ctrl Pts',(1.90025875963967,14.6065011777634,-10.0512733560803));
#60233=CARTESIAN_POINT('Ctrl Pts',(1.89355247274411,14.6054074046373,-10.0518279831358));
#60234=CARTESIAN_POINT('Ctrl Pts',(1.87725698375451,14.6013332347428,-10.0552320469979));
#60235=CARTESIAN_POINT('Ctrl Pts',(1.86829211419564,14.5978127562131,-10.0589614875639));
#60236=CARTESIAN_POINT('Ctrl Pts',(1.84706044348034,14.5870683867587,-10.0712702530576));
#60237=CARTESIAN_POINT('Ctrl Pts',(1.83585892185219,14.5787550531425,-10.0815819441629));
#60238=CARTESIAN_POINT('Ctrl Pts',(1.80877471345896,14.5541268705494,-10.1129760302166));
#60239=CARTESIAN_POINT('Ctrl Pts',(1.79294392498976,14.5329375758433,-10.1410429474192));
#60240=CARTESIAN_POINT('Ctrl Pts',(1.76567283597306,14.4785632453863,-10.2144033500531));
#60241=CARTESIAN_POINT('Ctrl Pts',(1.75650699269238,14.447966727982,-10.2562595787923));
#60242=CARTESIAN_POINT('Ctrl Pts',(1.74778527727017,14.4026186544864,-10.318451044181));
#60243=CARTESIAN_POINT('Ctrl Pts',(1.74564598164349,14.386295392045,-10.3408770076572));
#60244=CARTESIAN_POINT('Ctrl Pts',(1.74342903876679,14.3580271947085,-10.3797436057744));
#60245=CARTESIAN_POINT('Ctrl Pts',(1.74295490171614,14.3459008172422,-10.3964264560461));
#60246=CARTESIAN_POINT('Ctrl Pts',(1.74292857696574,14.3218037566107,-10.4295927678051));
#60247=CARTESIAN_POINT('Ctrl Pts',(1.74337239383366,14.3097358503654,-10.4462099845861));
#60248=CARTESIAN_POINT('Ctrl Pts',(1.74549594744651,14.281769432407,-10.484741737058));
#60249=CARTESIAN_POINT('Ctrl Pts',(1.74755180318315,14.2657028933416,-10.5068945909261));
#60250=CARTESIAN_POINT('Ctrl Pts',(1.75591196457144,14.2213535217086,-10.5681486124389));
#60251=CARTESIAN_POINT('Ctrl Pts',(1.76464297432536,14.1917029071061,-10.6092002023577));
#60252=CARTESIAN_POINT('Ctrl Pts',(1.79360739934014,14.1332147014387,-10.6912265321584));
#60253=CARTESIAN_POINT('Ctrl Pts',(1.81322842074495,14.1096237409606,-10.7250788098309));
#60254=CARTESIAN_POINT('Ctrl Pts',(1.84745113278872,14.0857929378121,-10.7612654174941));
#60255=CARTESIAN_POINT('Ctrl Pts',(1.8598043937786,14.0801722471147,-10.7703887241685));
#60256=CARTESIAN_POINT('Ctrl Pts',(1.8784660619361,14.0751582426553,-10.7796242046062));
#60257=CARTESIAN_POINT('Ctrl Pts',(1.88517766043029,14.0739697528522,-10.7821409674899));
#60258=CARTESIAN_POINT('Ctrl Pts',(1.89712731924284,14.0731201278109,-10.7849686486973));
#60259=CARTESIAN_POINT('Ctrl Pts',(1.90207774199917,14.0731114184848,-10.7856919622349));
#60260=CARTESIAN_POINT('Ctrl Pts',(1.90706327644678,14.0734548558899,-10.7859608904011));
#60261=CARTESIAN_POINT('',(1.62584114411962,17.5755151259486,-9.86239943185911));
#60262=CARTESIAN_POINT('Origin',(1.62584114411962,16.1931736153679,-11.7650292949391));
#60263=CARTESIAN_POINT('',(1.33846910697111,17.3707409263229,-10.0842167666784));
#60264=CARTESIAN_POINT('Origin',(1.63623295246351,17.4003192372954,-10.1057066675065));
#60265=CARTESIAN_POINT('Origin',(1.33846910697111,16.1646275725617,-11.7442893808342));
#60266=CARTESIAN_POINT('Origin',(1.62584114411962,16.1931736153679,-11.7650292949391));
#60267=CARTESIAN_POINT('Origin',(5.83867335851287,16.611654445725,-12.0690734153485));
#60268=CARTESIAN_POINT('',(10.3480326234796,15.2192095552406,-10.4646480417893));
#60269=CARTESIAN_POINT('Ctrl Pts',(10.3480326234796,15.2192095552406,-10.4646480417893));
#60270=CARTESIAN_POINT('Ctrl Pts',(7.54753623341465,15.0162497111978,-10.3273833808683));
#60271=CARTESIAN_POINT('Ctrl Pts',(4.70781617470128,14.8102983544992,-10.1884122025895));
#60272=CARTESIAN_POINT('Ctrl Pts',(1.90706327644678,14.6069951093592,-10.0516057316823));
#60273=CARTESIAN_POINT('',(10.0307219562183,18.584225684205,-10.2297540313114));
#60274=CARTESIAN_POINT('Origin',(10.0307219562183,17.0280707397496,-12.3716175623118));
#60275=CARTESIAN_POINT('',(10.3480326234796,14.655466104402,-11.2405743353076));
#60276=CARTESIAN_POINT('Origin',(10.0307219562183,17.0280707397496,-12.3716175623118));
#60277=CARTESIAN_POINT('Ctrl Pts',(1.90706327644677,14.0734548558899,-10.7859608904011));
#60278=CARTESIAN_POINT('Ctrl Pts',(4.70781616958245,14.2663896989247,-10.9370382417485));
#60279=CARTESIAN_POINT('Ctrl Pts',(7.54753622799763,14.4622016128173,-11.0899651657448));
#60280=CARTESIAN_POINT('Ctrl Pts',(10.3480326234796,14.655466104402,-11.2405743353076));
#60281=CARTESIAN_POINT('Origin',(10.0411137645622,17.0291030079158,-12.3723675490348));
#60282=CARTESIAN_POINT('',(10.3388776100546,18.4386081065242,-10.4945511677868));
#60283=CARTESIAN_POINT('Origin',(10.3388776100546,17.0586813188882,-12.3938574498629));
#60284=CARTESIAN_POINT('Origin',(10.0411137645622,18.4090297955518,-10.4730612669588));
#60285=CARTESIAN_POINT('Ctrl Pts',(10.3480326234796,14.655466104402,-11.2405743353076));
#60286=CARTESIAN_POINT('Ctrl Pts',(10.3515211595623,14.6557068510616,-11.2407619468765));
#60287=CARTESIAN_POINT('Ctrl Pts',(10.3550011198928,14.656127803182,-11.2407133851835));
#60288=CARTESIAN_POINT('Ctrl Pts',(10.3584662558372,14.6567254954937,-11.2404322010368));
#60289=CARTESIAN_POINT('Ctrl Pts',(10.3671694892744,14.658226693656,-11.2397259628669));
#60290=CARTESIAN_POINT('Ctrl Pts',(10.3753654465597,14.6607699081134,-11.2375879642563));
#60291=CARTESIAN_POINT('Ctrl Pts',(10.3941492137284,14.6687216746163,-11.2299109713814));
#60292=CARTESIAN_POINT('Ctrl Pts',(10.404002965845,14.6748808959337,-11.2232825987702));
#60293=CARTESIAN_POINT('Ctrl Pts',(10.4308436412037,14.695462505518,-11.2002100598276));
#60294=CARTESIAN_POINT('Ctrl Pts',(10.4443760953691,14.7123773258611,-11.1799381757228));
#60295=CARTESIAN_POINT('Ctrl Pts',(10.4751024728252,14.7571304838423,-11.1253565526294));
#60296=CARTESIAN_POINT('Ctrl Pts',(10.4913920727396,14.7969697951171,-11.0748241683199));
#60297=CARTESIAN_POINT('Ctrl Pts',(10.5062952995223,14.8615728881704,-10.9899781948953));
#60298=CARTESIAN_POINT('Ctrl Pts',(10.5095242362634,14.8818952699721,-10.9629200882245));
#60299=CARTESIAN_POINT('Ctrl Pts',(10.512859180135,14.9149069041019,-10.9184305611833));
#60300=CARTESIAN_POINT('Ctrl Pts',(10.5136719991087,14.9279744210183,-10.9006780007671));
#60301=CARTESIAN_POINT('Ctrl Pts',(10.514295657022,14.9525087414764,-10.8670882523062));
#60302=CARTESIAN_POINT('Ctrl Pts',(10.5142026737932,14.9640796299257,-10.8511355186813));
#60303=CARTESIAN_POINT('Ctrl Pts',(10.5131483322071,14.9893112870104,-10.8161050999279));
#60304=CARTESIAN_POINT('Ctrl Pts',(10.512009812725,15.0030451759508,-10.7968758883503));
#60305=CARTESIAN_POINT('Ctrl Pts',(10.5074172692912,15.0390378011655,-10.7460384791958));
#60306=CARTESIAN_POINT('Ctrl Pts',(10.5028514263372,15.0615825002595,-10.7137256630154));
#60307=CARTESIAN_POINT('Ctrl Pts',(10.4823258875197,15.1286103745233,-10.6159756467566));
#60308=CARTESIAN_POINT('Ctrl Pts',(10.4610892332281,15.1642626717183,-10.5615248358069));
#60309=CARTESIAN_POINT('Ctrl Pts',(10.4253700252923,15.1959357631409,-10.5103262009133));
#60310=CARTESIAN_POINT('Ctrl Pts',(10.4122912190471,15.2055154329319,-10.4944454192631));
#60311=CARTESIAN_POINT('Ctrl Pts',(10.3868737804665,15.2153586960742,-10.4762419431139));
#60312=CARTESIAN_POINT('Ctrl Pts',(10.3771760707494,15.2179090290457,-10.4710384088583));
#60313=CARTESIAN_POINT('Ctrl Pts',(10.3604838650279,15.2195700377639,-10.4660465521435));
#60314=CARTESIAN_POINT('Ctrl Pts',(10.35429238307,15.2196632176109,-10.4649548601736));
#60315=CARTESIAN_POINT('Ctrl Pts',(10.3480326234796,15.2192095552406,-10.4646480417893));
#60316=CARTESIAN_POINT('Origin',(10.3388776100546,17.0586813188882,-12.3938574498629));
#60317=CARTESIAN_POINT('Origin',(1.05309141530195,18.0449568312087,-13.110428553894));
#60318=CARTESIAN_POINT('Origin',(1.63623295246351,11.7657792816622,-16.1942058835342));
#60319=CARTESIAN_POINT('',(1.90706327644678,10.7859608904011,-14.0734548558899));
#60320=CARTESIAN_POINT('',(1.90706327644678,10.0516057316823,-14.6069951093593));
#60321=CARTESIAN_POINT('Ctrl Pts',(1.90706327644678,10.7859608904011,-14.0734548558899));
#60322=CARTESIAN_POINT('Ctrl Pts',(1.90025875961112,10.7855938432463,-14.0729861146486));
#60323=CARTESIAN_POINT('Ctrl Pts',(1.89355247269903,10.7843822139896,-14.0731756018473));
#60324=CARTESIAN_POINT('Ctrl Pts',(1.87725698375378,10.7794555345929,-14.0751540712246));
#60325=CARTESIAN_POINT('Ctrl Pts',(1.86829211419484,10.7749549000322,-14.0776130922831));
#60326=CARTESIAN_POINT('Ctrl Pts',(1.84706044347947,10.7609327797315,-14.0859992311584));
#60327=CARTESIAN_POINT('Ctrl Pts',(1.83585892185124,10.7498398418311,-14.0932372708109));
#60328=CARTESIAN_POINT('Ctrl Pts',(1.80877471345775,10.7167157421771,-14.1154842939643));
#60329=CARTESIAN_POINT('Ctrl Pts',(1.79294392498838,10.687890370975,-14.1356296662997));
#60330=CARTESIAN_POINT('Ctrl Pts',(1.76567283597227,10.6135076985461,-14.1885969630943));
#60331=CARTESIAN_POINT('Ctrl Pts',(1.75650699269191,10.5714743952927,-14.2189497583371));
#60332=CARTESIAN_POINT('Ctrl Pts',(1.74778527726998,10.5091275947838,-14.2640840313801));
#60333=CARTESIAN_POINT('Ctrl Pts',(1.74564598164336,10.4866732458425,-14.2803682245802));
#60334=CARTESIAN_POINT('Ctrl Pts',(1.74342903876675,10.4477781532305,-14.308597202608));
#60335=CARTESIAN_POINT('Ctrl Pts',(1.74295490171611,10.4310899986737,-14.3207162793519));
#60336=CARTESIAN_POINT('Ctrl Pts',(1.74292857696575,10.3979233781616,-14.3448129150226));
#60337=CARTESIAN_POINT('Ctrl Pts',(1.74337239383371,10.3813111149047,-14.3568876392085));
#60338=CARTESIAN_POINT('Ctrl Pts',(1.74549594744661,10.3428065045311,-14.3848914150601));
#60339=CARTESIAN_POINT('Ctrl Pts',(1.74755180318332,10.3206807095391,-14.4009951974742));
#60340=CARTESIAN_POINT('Ctrl Pts',(1.75591196457188,10.2595734170318,-14.4455465242593));
#60341=CARTESIAN_POINT('Ctrl Pts',(1.76464297432612,10.2186883678702,-14.4754263625507));
#60342=CARTESIAN_POINT('Ctrl Pts',(1.79360739934209,10.1377152488482,-14.5353641884944));
#60343=CARTESIAN_POINT('Ctrl Pts',(1.81322842074769,10.1048179830608,-14.560269610065));
#60344=CARTESIAN_POINT('Ctrl Pts',(1.8474511327924,10.0709712657025,-14.5873209959223));
#60345=CARTESIAN_POINT('Ctrl Pts',(1.85980439378186,10.0628064143825,-14.5942608872388));
#60346=CARTESIAN_POINT('Ctrl Pts',(1.87846606193842,10.0551838923632,-14.6014949385016));
#60347=CARTESIAN_POINT('Ctrl Pts',(1.88517766043213,10.0532758488899,-14.603521258695));
#60348=CARTESIAN_POINT('Ctrl Pts',(1.89712731918336,10.051594005919,-14.605947994744));
#60349=CARTESIAN_POINT('Ctrl Pts',(1.90207774195904,10.0513622066718,-14.6066332154768));
#60350=CARTESIAN_POINT('Ctrl Pts',(1.90706327644678,10.0516057316823,-14.6069951093592));
#60351=CARTESIAN_POINT('',(1.62584114411962,13.6676591580191,-14.8108321047873));
#60352=CARTESIAN_POINT('Origin',(1.62584114411962,11.7650292949391,-16.1931736153679));
#60353=CARTESIAN_POINT('',(1.33846910697111,13.4043619949899,-14.9585142188006));
#60354=CARTESIAN_POINT('Origin',(1.63623295246351,13.425851895818,-14.988092529773));
#60355=CARTESIAN_POINT('Origin',(1.33846910697111,11.7442893808342,-16.1646275725618));
#60356=CARTESIAN_POINT('Origin',(1.62584114411962,11.7650292949391,-16.1931736153679));
#60357=CARTESIAN_POINT('Origin',(5.83867335851287,12.0690734153485,-16.611654445725));
#60358=CARTESIAN_POINT('',(10.3480326234796,11.2405743353076,-14.655466104402));
#60359=CARTESIAN_POINT('Ctrl Pts',(10.3480326234796,11.2405743353076,-14.655466104402));
#60360=CARTESIAN_POINT('Ctrl Pts',(7.54753623341466,11.0899651660362,-14.4622016131911));
#60361=CARTESIAN_POINT('Ctrl Pts',(4.70781617470128,10.9370382420246,-14.2663896992774));
#60362=CARTESIAN_POINT('Ctrl Pts',(1.90706327644678,10.7859608904011,-14.0734548558899));
#60363=CARTESIAN_POINT('',(10.0307219562183,14.5134810933121,-15.4719157952941));
#60364=CARTESIAN_POINT('Origin',(10.0307219562183,12.3716175623118,-17.0280707397496));
#60365=CARTESIAN_POINT('',(10.3480326234796,10.4646480417893,-15.2192095552406));
#60366=CARTESIAN_POINT('Origin',(10.0307219562183,12.3716175623118,-17.0280707397496));
#60367=CARTESIAN_POINT('Ctrl Pts',(1.90706327644677,10.0516057316823,-14.6069951093592));
#60368=CARTESIAN_POINT('Ctrl Pts',(4.70781616958245,10.1884122023394,-14.8102983541277));
#60369=CARTESIAN_POINT('Ctrl Pts',(7.54753622799763,10.3273833806028,-15.0162497108052));
#60370=CARTESIAN_POINT('Ctrl Pts',(10.3480326234796,10.4646480417893,-15.2192095552406));
#60371=CARTESIAN_POINT('Origin',(10.0411137645622,12.3723675490348,-17.0291030079158));
#60372=CARTESIAN_POINT('',(10.3388776100546,14.2931637319389,-15.6787545312522));
#60373=CARTESIAN_POINT('Origin',(10.3388776100546,12.3938574498629,-17.0586813188882));
#60374=CARTESIAN_POINT('Origin',(10.0411137645622,14.2716738311109,-15.6491762202798));
#60375=CARTESIAN_POINT('Ctrl Pts',(10.3480326234796,10.4646480417893,-15.2192095552406));
#60376=CARTESIAN_POINT('Ctrl Pts',(10.3515211595624,10.4648190303056,-15.2194623792549));
#60377=CARTESIAN_POINT('Ctrl Pts',(10.3550011198928,10.4652343859512,-15.2195462756993));
#60378=CARTESIAN_POINT('Ctrl Pts',(10.3584662558372,10.4658897157988,-15.219463550766));
#60379=CARTESIAN_POINT('Ctrl Pts',(10.3671694892744,10.46753567969,-15.2192557740966));
#60380=CARTESIAN_POINT('Ctrl Pts',(10.3753654465597,10.4706150982766,-15.2180083130739));
#60381=CARTESIAN_POINT('Ctrl Pts',(10.3941492137284,10.4805499988893,-15.2131642899593));
#60382=CARTESIAN_POINT('Ctrl Pts',(10.404002965845,10.4884560462404,-15.2087636370542));
#60383=CARTESIAN_POINT('Ctrl Pts',(10.4308436412037,10.5151601267881,-15.1931804156785));
#60384=CARTESIAN_POINT('Ctrl Pts',(10.4443760953692,10.5375114335938,-15.1791276751458));
#60385=CARTESIAN_POINT('Ctrl Pts',(10.4751024728251,10.5969408652328,-15.1410469532011));
#60386=CARTESIAN_POINT('Ctrl Pts',(10.4913920727396,10.6504456673432,-15.1052988240478));
#60387=CARTESIAN_POINT('Ctrl Pts',(10.5062952995223,10.7381057076571,-15.0445689617834));
#60388=CARTESIAN_POINT('Ctrl Pts',(10.5095242362634,10.7657948560931,-15.0251151344584));
#60389=CARTESIAN_POINT('Ctrl Pts',(10.512859180135,10.8109388057734,-14.9930042358172));
#60390=CARTESIAN_POINT('Ctrl Pts',(10.5136719991087,10.8288525957508,-14.9801586323538));
#60391=CARTESIAN_POINT('Ctrl Pts',(10.514295657022,10.8625659242063,-14.9557944051666));
#60392=CARTESIAN_POINT('Ctrl Pts',(10.5142026737932,10.8785001588622,-14.9441980550706));
#60393=CARTESIAN_POINT('Ctrl Pts',(10.5131483322071,10.9133218854645,-14.918679157882));
#60394=CARTESIAN_POINT('Ctrl Pts',(10.512009812725,10.9323257432013,-14.9046350959894));
#60395=CARTESIAN_POINT('Ctrl Pts',(10.5074172692912,10.982266387329,-14.867408179605));
#60396=CARTESIAN_POINT('Ctrl Pts',(10.5028514263372,11.0136928796461,-14.8436435603699));
#60397=CARTESIAN_POINT('Ctrl Pts',(10.4823258875198,11.1076465924618,-14.7713905226839));
#60398=CARTESIAN_POINT('Ctrl Pts',(10.4610892332284,11.1583801679713,-14.7306218898341));
#60399=CARTESIAN_POINT('Ctrl Pts',(10.4253700252927,11.2043243162307,-14.6917166180072));
#60400=CARTESIAN_POINT('Ctrl Pts',(10.4122912190473,11.2183425550236,-14.6795733779006));
#60401=CARTESIAN_POINT('Ctrl Pts',(10.3868737804666,11.2333292380637,-14.6653025788806));
#60402=CARTESIAN_POINT('Ctrl Pts',(10.3771760707494,11.2373627293707,-14.6611418199486));
#60403=CARTESIAN_POINT('Ctrl Pts',(10.3604838650279,11.2404850110942,-14.6569075620133));
#60404=CARTESIAN_POINT('Ctrl Pts',(10.35429238307,11.2409109817661,-14.6558980954078));
#60405=CARTESIAN_POINT('Ctrl Pts',(10.3480326234796,11.2405743353076,-14.655466104402));
#60406=CARTESIAN_POINT('Origin',(10.3388776100546,12.3938574498629,-17.0586813188882));
#60407=CARTESIAN_POINT('Origin',(1.05309141530195,13.110428553894,-18.0449568312087));
#60408=CARTESIAN_POINT('Origin',(1.63623295246351,6.18563622669653,-19.0374307818588));
#60409=CARTESIAN_POINT('',(1.90706327644678,5.90912166928202,-16.7176961632773));
#60410=CARTESIAN_POINT('',(1.90706327644678,5.04583540480241,-16.998194874094));
#60411=CARTESIAN_POINT('Ctrl Pts',(1.90706327644678,5.90912166928201,-16.7176961632773));
#60412=CARTESIAN_POINT('Ctrl Pts',(1.9002601439292,5.90891747725266,-16.7171370538257));
#60413=CARTESIAN_POINT('Ctrl Pts',(1.8935551778176,5.90770704487272,-16.716942816161));
#60414=CARTESIAN_POINT('Ctrl Pts',(1.87732280058987,5.90243158644669,-16.7173002954459));
#60415=CARTESIAN_POINT('Ctrl Pts',(1.86840987580667,5.89743569235132,-16.7182373577841));
#60416=CARTESIAN_POINT('Ctrl Pts',(1.84749974154032,5.88180608769513,-16.7218050267902));
#60417=CARTESIAN_POINT('Ctrl Pts',(1.83650132567016,5.86939109701695,-16.7251494451272));
#60418=CARTESIAN_POINT('Ctrl Pts',(1.81085694928208,5.833521535894,-16.7353298338008));
#60419=CARTESIAN_POINT('Ctrl Pts',(1.79594323550271,5.80312318642244,-16.7445431753855));
#60420=CARTESIAN_POINT('Ctrl Pts',(1.76902539468131,5.72294526487886,-16.7696407324889));
#60421=CARTESIAN_POINT('Ctrl Pts',(1.75949337448621,5.67650047047182,-16.7845442855156));
#60422=CARTESIAN_POINT('Ctrl Pts',(1.74741836256394,5.58926584376222,-16.812676669263));
#60423=CARTESIAN_POINT('Ctrl Pts',(1.74418490387288,5.54515926519586,-16.8269787063902));
#60424=CARTESIAN_POINT('Ctrl Pts',(1.74230474178708,5.45939048648168,-16.8548265548082));
#60425=CARTESIAN_POINT('Ctrl Pts',(1.74356051202781,5.4159089215945,-16.8689635910091));
#60426=CARTESIAN_POINT('Ctrl Pts',(1.75089245923108,5.32933507280858,-16.8971914959595));
#60427=CARTESIAN_POINT('Ctrl Pts',(1.75736442403597,5.28389327657364,-16.9120469371971));
#60428=CARTESIAN_POINT('Ctrl Pts',(1.77948145071048,5.18955296706469,-16.9432828393365));
#60429=CARTESIAN_POINT('Ctrl Pts',(1.79536357091631,5.14706849481883,-16.9576377997399));
#60430=CARTESIAN_POINT('Ctrl Pts',(1.82385809602977,5.09851442742686,-16.9748765638372));
#60431=CARTESIAN_POINT('Ctrl Pts',(1.83844662204133,5.07756522074326,-16.9824854044486));
#60432=CARTESIAN_POINT('Ctrl Pts',(1.86612294571258,5.05694052510253,-16.9911586174827));
#60433=CARTESIAN_POINT('Ctrl Pts',(1.87511027899494,5.0519707075161,-16.9934563480593));
#60434=CARTESIAN_POINT('Ctrl Pts',(1.88937385988128,5.04758145200932,-16.9960621155412));
#60435=CARTESIAN_POINT('Ctrl Pts',(1.89395673353178,5.04662994623243,-16.9967628607251));
#60436=CARTESIAN_POINT('Ctrl Pts',(1.90144341439779,5.04587570170987,-16.9976700356524));
#60437=CARTESIAN_POINT('Ctrl Pts',(1.90425145406703,5.04576785233642,-16.9979583144138));
#60438=CARTESIAN_POINT('Ctrl Pts',(1.90706327644678,5.04583540480241,-16.998194874094));
#60439=CARTESIAN_POINT('',(1.62584114411962,8.42191748352189,-18.3094773381637));
#60440=CARTESIAN_POINT('Origin',(1.62584114411962,6.18524193534253,-19.0362172778497));
#60441=CARTESIAN_POINT('',(1.33846910697111,8.12587071790561,-18.3685680770895));
#60442=CARTESIAN_POINT('Origin',(1.63623295246351,8.13716862736726,-18.4033394670442));
#60443=CARTESIAN_POINT('Origin',(1.33846910697111,6.17433831723488,-19.0026593919042));
#60444=CARTESIAN_POINT('Origin',(1.62584114411962,6.18524193534253,-19.0362172778497));
#60445=CARTESIAN_POINT('Origin',(5.83867335851287,6.34508738889865,-19.5281709987517));
#60446=CARTESIAN_POINT('',(10.3480326234796,6.16163338174818,-17.4117050340792));
#60447=CARTESIAN_POINT('Ctrl Pts',(10.3480326234796,6.16163338174816,-17.4117050340792));
#60448=CARTESIAN_POINT('Ctrl Pts',(7.54972025675579,6.078182693581,-17.1815384276765));
#60449=CARTESIAN_POINT('Ctrl Pts',(4.7091881268347,5.99322580193244,-16.9479863250953));
#60450=CARTESIAN_POINT('Ctrl Pts',(1.90706327644678,5.90912166928201,-16.7176961632773));
#60451=CARTESIAN_POINT('',(10.0307219562183,9.02205585163692,-19.1995786420573));
#60452=CARTESIAN_POINT('Origin',(10.0307219562183,6.50414425974676,-20.0176977116355));
#60453=CARTESIAN_POINT('',(10.3480326234796,5.2494773173561,-17.7080825054385));
#60454=CARTESIAN_POINT('Origin',(10.0307219562183,6.50414425974676,-20.0176977116355));
#60455=CARTESIAN_POINT('Ctrl Pts',(1.90706327644677,5.04583540480242,-16.998194874094));
#60456=CARTESIAN_POINT('Ctrl Pts',(4.70918812184411,5.11315489293588,-17.2339386970511));
#60457=CARTESIAN_POINT('Ctrl Pts',(7.54972025123708,5.18170180532828,-17.4728227250588));
#60458=CARTESIAN_POINT('Ctrl Pts',(10.3480326234796,5.24947731735612,-17.7080825054385));
#60459=CARTESIAN_POINT('Origin',(10.0411137645622,6.50453855110076,-20.0189112156446));
#60460=CARTESIAN_POINT('',(10.3388776100546,8.74860490494394,-19.3282121608924));
#60461=CARTESIAN_POINT('Origin',(10.3388776100546,6.51583646056242,-20.0536826055992));
#60462=CARTESIAN_POINT('Origin',(10.0411137645622,8.73730699548229,-19.2934407709377));
#60463=CARTESIAN_POINT('Ctrl Pts',(10.3480326234796,5.24947731735612,-17.7080825054385));
#60464=CARTESIAN_POINT('Ctrl Pts',(10.3515114639741,5.24956157535323,-17.7083749785944));
#60465=CARTESIAN_POINT('Ctrl Pts',(10.3549914179992,5.24992909484554,-17.7085835892234));
#60466=CARTESIAN_POINT('Ctrl Pts',(10.3584662558372,5.25057973058011,-17.7087077679084));
#60467=CARTESIAN_POINT('Ctrl Pts',(10.367223098271,5.2522193796443,-17.7090207071676));
#60468=CARTESIAN_POINT('Ctrl Pts',(10.3753630700178,5.25553811631358,-17.7087794103521));
#60469=CARTESIAN_POINT('Ctrl Pts',(10.3939290316259,5.26631748509036,-17.7072720478088));
#60470=CARTESIAN_POINT('Ctrl Pts',(10.4035780672154,5.27498292572689,-17.705574721304));
#60471=CARTESIAN_POINT('Ctrl Pts',(10.4280013399751,5.30215236459277,-17.6996950906475));
#60472=CARTESIAN_POINT('Ctrl Pts',(10.4407678160189,5.32424702952846,-17.6942316042004));
#60473=CARTESIAN_POINT('Ctrl Pts',(10.4685456259701,5.38326592638977,-17.6789356068263));
#60474=CARTESIAN_POINT('Ctrl Pts',(10.4828713837318,5.4302145128124,-17.6659261793663));
#60475=CARTESIAN_POINT('Ctrl Pts',(10.5038238234649,5.53612436501362,-17.6349429829058));
#60476=CARTESIAN_POINT('Ctrl Pts',(10.5097149363751,5.59075039378809,-17.6182406825358));
#60477=CARTESIAN_POINT('Ctrl Pts',(10.5152093525458,5.6973277721556,-17.5845792171893));
#60478=CARTESIAN_POINT('Ctrl Pts',(10.5146501294348,5.75259648941307,-17.5665197371488));
#60479=CARTESIAN_POINT('Ctrl Pts',(10.5071723447785,5.85782934815576,-17.5310183201387));
#60480=CARTESIAN_POINT('Ctrl Pts',(10.5000174147823,5.91132323381314,-17.5123838347761));
#60481=CARTESIAN_POINT('Ctrl Pts',(10.4763655908937,6.01347812322461,-17.4753908390236));
#60482=CARTESIAN_POINT('Ctrl Pts',(10.4605419031703,6.05642735042498,-17.4590326714754));
#60483=CARTESIAN_POINT('Ctrl Pts',(10.4319469960435,6.10705647468785,-17.4387122071681));
#60484=CARTESIAN_POINT('Ctrl Pts',(10.4192298015583,6.12493725783482,-17.4312562494153));
#60485=CARTESIAN_POINT('Ctrl Pts',(10.3949786188434,6.14650298767116,-17.421409626235));
#60486=CARTESIAN_POINT('Ctrl Pts',(10.3846960006404,6.15331567799442,-17.4180488377084));
#60487=CARTESIAN_POINT('Ctrl Pts',(10.3651744504234,6.16041901843185,-17.4137258644339));
#60488=CARTESIAN_POINT('Ctrl Pts',(10.3566858346071,6.16189143600687,-17.4124167774369));
#60489=CARTESIAN_POINT('Ctrl Pts',(10.3480326234796,6.16163338174815,-17.4117050340792));
#60490=CARTESIAN_POINT('Origin',(10.3388776100546,6.51583646056242,-20.0536826055992));
#60491=CARTESIAN_POINT('Origin',(1.05309141530195,6.89256018399712,-21.2131190072776));
#60492=CARTESIAN_POINT('Origin',(1.63623295246351,-3.67708883828686E-15,
-20.0171393136753));
#60493=CARTESIAN_POINT('',(1.90706327644678,0.453856447902039,-17.7254928911647));
#60494=CARTESIAN_POINT('',(1.90706327644678,-0.453856447902044,-17.7254928911647));
#60495=CARTESIAN_POINT('Ctrl Pts',(1.90706327644678,0.45385644790203,-17.7254928911647));
#60496=CARTESIAN_POINT('Ctrl Pts',(1.90025953256256,0.453835022138929,-17.7248979942144));
#60497=CARTESIAN_POINT('Ctrl Pts',(1.89355398313235,0.452743661153183,-17.7243391729909));
#60498=CARTESIAN_POINT('Ctrl Pts',(1.87729436838704,0.447606881402708,-17.7230467959921));
#60499=CARTESIAN_POINT('Ctrl Pts',(1.86835902889014,0.442546314021896,-17.722392711458));
#60500=CARTESIAN_POINT('Ctrl Pts',(1.84731494010094,0.426450928593982,-17.7209473414007));
#60501=CARTESIAN_POINT('Ctrl Pts',(1.83623221810553,0.41344928658027,-17.7202879485127));
#60502=CARTESIAN_POINT('Ctrl Pts',(1.81006546585959,0.375219786705405,-17.7188609517426));
#60503=CARTESIAN_POINT('Ctrl Pts',(1.7948444517497,0.342313735271062,-17.7182253713052));
#60504=CARTESIAN_POINT('Ctrl Pts',(1.76839326635828,0.257598032772368,-17.717351777811));
#60505=CARTESIAN_POINT('Ctrl Pts',(1.7592161614996,0.210107900651409,-17.7171803340554));
#60506=CARTESIAN_POINT('Ctrl Pts',(1.74822227890756,0.126194388056534,-17.7169975657511));
#60507=CARTESIAN_POINT('Ctrl Pts',(1.74516474660436,0.0869626247327569,
-17.716966780863));
#60508=CARTESIAN_POINT('Ctrl Pts',(1.74251542765413,0.0122397150418686,
-17.7169388371718));
#60509=CARTESIAN_POINT('Ctrl Pts',(1.74267268152327,-0.0243528511786891,
-17.7169400569674));
#60510=CARTESIAN_POINT('Ctrl Pts',(1.74602547045575,-0.0996677434135249,
-17.71697649914));
#60511=CARTESIAN_POINT('Ctrl Pts',(1.74954197522153,-0.139554220968226,
-17.7170140039981));
#60512=CARTESIAN_POINT('Ctrl Pts',(1.76185308853241,-0.224756276798996,
-17.7172332241402));
#60513=CARTESIAN_POINT('Ctrl Pts',(1.77207894319219,-0.273353606336582,
-17.7174389665532));
#60514=CARTESIAN_POINT('Ctrl Pts',(1.7982477557649,-0.348923678359701,-17.7183749061735));
#60515=CARTESIAN_POINT('Ctrl Pts',(1.81321786098122,-0.382374164866885,
-17.7189861130437));
#60516=CARTESIAN_POINT('Ctrl Pts',(1.84564815302462,-0.424859842185331,
-17.7208443091635));
#60517=CARTESIAN_POINT('Ctrl Pts',(1.85822154357159,-0.436125221546959,
-17.7216651227597));
#60518=CARTESIAN_POINT('Ctrl Pts',(1.8772926198921,-0.447206202216732,-17.7230568968888));
#60519=CARTESIAN_POINT('Ctrl Pts',(1.88421421928191,-0.450152284723857,
-17.7235877581235));
#60520=CARTESIAN_POINT('Ctrl Pts',(1.8966397075418,-0.45319057567647,-17.7245977295869));
#60521=CARTESIAN_POINT('Ctrl Pts',(1.90183077502292,-0.453839970160096,
-17.7250353784787));
#60522=CARTESIAN_POINT('Ctrl Pts',(1.90706327644678,-0.453856447902034,
-17.7254928911647));
#60523=CARTESIAN_POINT('',(1.62584114411962,2.35177984678801,-20.0158633600508));
#60524=CARTESIAN_POINT('Origin',(1.62584114411962,-3.82085943249196E-15,
-20.0158633600508));
#60525=CARTESIAN_POINT('',(1.33846910697111,2.05196259868229,-19.9805785106537));
#60526=CARTESIAN_POINT('Origin',(1.63623295246351,2.05196259868229,-20.0171393136753));
#60527=CARTESIAN_POINT('Origin',(1.33846910697111,-3.67037272772767E-15,
-19.9805785106537));
#60528=CARTESIAN_POINT('Origin',(1.62584114411962,-3.82085943249196E-15,
-20.0158633600508));
#60529=CARTESIAN_POINT('Origin',(5.83867335851287,-3.77187554531221E-15,
-20.5331341136527));
#60530=CARTESIAN_POINT('',(10.3480326234796,0.479548822159042,-18.4635649605383));
#60531=CARTESIAN_POINT('Ctrl Pts',(10.3480326234796,0.479548822159038,-18.4635649605383));
#60532=CARTESIAN_POINT('Ctrl Pts',(7.55083071619378,0.471311164566918,-18.2189729292873));
#60533=CARTESIAN_POINT('Ctrl Pts',(4.70971831191321,0.462682327280518,-17.9705478141232));
#60534=CARTESIAN_POINT('Ctrl Pts',(1.90706327644678,0.453856447902024,-17.7254928911647));
#60535=CARTESIAN_POINT('',(10.0307219562183,2.64748892284414,-21.0478529600056));
#60536=CARTESIAN_POINT('Origin',(10.0307219562183,-4.0285398052162E-15,
-21.0478529600056));
#60537=CARTESIAN_POINT('',(10.3480326234796,-0.479548822159047,-18.4635649605383));
#60538=CARTESIAN_POINT('Origin',(10.0307219562183,-4.0285398052162E-15,
-21.0478529600056));
#60539=CARTESIAN_POINT('Ctrl Pts',(1.90706327644678,-0.453856447902027,
-17.7254928911647));
#60540=CARTESIAN_POINT('Ctrl Pts',(4.70971830698342,-0.462682327264996,
-17.9705478136921));
#60541=CARTESIAN_POINT('Ctrl Pts',(7.55083071063943,-0.471311164550564,
-18.2189729288016));
#60542=CARTESIAN_POINT('Ctrl Pts',(10.3480326234796,-0.479548822159041,
-18.4635649605383));
#60543=CARTESIAN_POINT('Origin',(10.0411137645622,-3.86666225233756E-15,
-21.0491289136301));
#60544=CARTESIAN_POINT('',(10.3388776100546,2.34767167473841,-21.0856897166516));
#60545=CARTESIAN_POINT('Origin',(10.3388776100546,-3.87337836289675E-15,
-21.0856897166516));
#60546=CARTESIAN_POINT('Origin',(10.0411137645622,2.34767167473841,-21.0491289136301));
#60547=CARTESIAN_POINT('Ctrl Pts',(10.3480326234796,-0.479548822159048,
-18.4635649605383));
#60548=CARTESIAN_POINT('Ctrl Pts',(10.3515043799367,-0.479559046355185,
-18.463868536752));
#60549=CARTESIAN_POINT('Ctrl Pts',(10.3549842920161,-0.479275189924437,
-18.4641804719486));
#60550=CARTESIAN_POINT('Ctrl Pts',(10.3584662558372,-0.47869358160788,-18.4645002849058));
#60551=CARTESIAN_POINT('Ctrl Pts',(10.3670410360545,-0.477261296913589,
-18.4652878651219));
#60552=CARTESIAN_POINT('Ctrl Pts',(10.3752404682198,-0.474083787713377,
-18.46608779957));
#60553=CARTESIAN_POINT('Ctrl Pts',(10.3939159291592,-0.4632713093104,-18.4679971841149));
#60554=CARTESIAN_POINT('Ctrl Pts',(10.4037620790052,-0.454395207725901,
-18.4690808995383));
#60555=CARTESIAN_POINT('Ctrl Pts',(10.4301534297193,-0.424234118800168,
-18.4721165427773));
#60556=CARTESIAN_POINT('Ctrl Pts',(10.4436201527526,-0.398508891735463,
-18.4738680701254));
#60557=CARTESIAN_POINT('Ctrl Pts',(10.4707559634892,-0.337044819567083,
-18.4775000338928));
#60558=CARTESIAN_POINT('Ctrl Pts',(10.4855434672333,-0.285219862910067,
-18.4797232784594));
#60559=CARTESIAN_POINT('Ctrl Pts',(10.503063797412,-0.184213295767446,-18.4824794109906));
#60560=CARTESIAN_POINT('Ctrl Pts',(10.5077954452097,-0.142902659146764,
-18.4832622430944));
#60561=CARTESIAN_POINT('Ctrl Pts',(10.5129524699051,-0.0690531837747938,
-18.4841201320625));
#60562=CARTESIAN_POINT('Ctrl Pts',(10.5141249106268,-0.0355299301020554,
-18.4843191140946));
#60563=CARTESIAN_POINT('Ctrl Pts',(10.5142094879025,0.0307774777111762,
-18.4843333798549));
#60564=CARTESIAN_POINT('Ctrl Pts',(10.5131850989077,0.064162825052976,-18.4841592802621));
#60565=CARTESIAN_POINT('Ctrl Pts',(10.5083046161227,0.137261078256548,-18.4833464708957));
#60566=CARTESIAN_POINT('Ctrl Pts',(10.503879825914,0.178099201717464,-18.4826118937437));
#60567=CARTESIAN_POINT('Ctrl Pts',(10.4867651973881,0.280116334659435,-18.479909817102));
#60568=CARTESIAN_POINT('Ctrl Pts',(10.4718859508697,0.334420796176041,-18.4776521193349));
#60569=CARTESIAN_POINT('Ctrl Pts',(10.4435576763643,0.398681362505802,-18.4738593034484));
#60570=CARTESIAN_POINT('Ctrl Pts',(10.4292853290429,0.426411149600926,-18.4719918118745));
#60571=CARTESIAN_POINT('Ctrl Pts',(10.4002072192656,0.457777203495769,-18.4686862833898));
#60572=CARTESIAN_POINT('Ctrl Pts',(10.3895121106101,0.466757785235072,-18.4675238404129));
#60573=CARTESIAN_POINT('Ctrl Pts',(10.3691517352141,0.476520858724239,-18.4654920629651));
#60574=CARTESIAN_POINT('Ctrl Pts',(10.3605255868115,0.478994932552591,-18.4646727052056));
#60575=CARTESIAN_POINT('Ctrl Pts',(10.350269709773,0.479524924856826,-18.4637613669848));
#60576=CARTESIAN_POINT('Ctrl Pts',(10.3491503490814,0.479552113820162,-18.4636626963416));
#60577=CARTESIAN_POINT('Ctrl Pts',(10.3480326234796,0.479548822159032,-18.4635649605383));
#60578=CARTESIAN_POINT('Origin',(10.3388776100546,-3.87337836289675E-15,
-21.0856897166516));
#60579=CARTESIAN_POINT('Origin',(1.05309141530195,-4.0973240570488E-15,
-22.3047932944232));
#60580=CARTESIAN_POINT('Origin',(1.63623295246351,-6.18563622669654,-19.0374307818588));
#60581=CARTESIAN_POINT('',(1.90706327644678,-5.04583540480242,-16.998194874094));
#60582=CARTESIAN_POINT('',(1.90706327644678,-5.90912166928202,-16.7176961632773));
#60583=CARTESIAN_POINT('Ctrl Pts',(1.90706327644678,-5.04583540480242,-16.998194874094));
#60584=CARTESIAN_POINT('Ctrl Pts',(1.90026014393011,-5.04567196333425,-16.9976225239826));
#60585=CARTESIAN_POINT('Ctrl Pts',(1.89355517781904,-5.04653705366502,-16.9967539081092));
#60586=CARTESIAN_POINT('Ctrl Pts',(1.8773228005899,-5.05101511023684,-16.9939422782637));
#60587=CARTESIAN_POINT('Ctrl Pts',(1.86840987580673,-5.05560766488491,-16.9917638647488));
#60588=CARTESIAN_POINT('Ctrl Pts',(1.84749974154032,-5.07034930389401,-16.985463318489));
#60589=CARTESIAN_POINT('Ctrl Pts',(1.83650132567015,-5.0823590421137,-16.9808716613319));
#60590=CARTESIAN_POINT('Ctrl Pts',(1.8108569492816,-5.1173620089685,-16.9680241697437));
#60591=CARTESIAN_POINT('Ctrl Pts',(1.79594323550237,-5.14737025660016,-16.9576102181472));
#60592=CARTESIAN_POINT('Ctrl Pts',(1.76902539468133,-5.22698753163545,-16.9307871685188));
#60593=CARTESIAN_POINT('Ctrl Pts',(1.75949337448622,-5.2733222482868,-16.9155448309956));
#60594=CARTESIAN_POINT('Ctrl Pts',(1.74741836256394,-5.3604323440714,-16.8870291804704));
#60595=CARTESIAN_POINT('Ctrl Pts',(1.74418490387289,-5.40452184219648,-16.8726745751501));
#60596=CARTESIAN_POINT('Ctrl Pts',(1.74230474178708,-5.49027879637103,-16.8447903345418));
#60597=CARTESIAN_POINT('Ctrl Pts',(1.7435605120278,-5.53376566269685,-16.8306696144911));
#60598=CARTESIAN_POINT('Ctrl Pts',(1.75089245923107,-5.62039732386611,-16.802619637761));
#60599=CARTESIAN_POINT('Ctrl Pts',(1.75736442403596,-5.66589231855089,-16.7879279245166));
#60600=CARTESIAN_POINT('Ctrl Pts',(1.77948145071066,-5.76057523481869,-16.7577464575557));
#60601=CARTESIAN_POINT('Ctrl Pts',(1.79536357091662,-5.80338352888467,-16.7443881182381));
#60602=CARTESIAN_POINT('Ctrl Pts',(1.82385809602968,-5.85279728585431,-16.7297952066033));
#60603=CARTESIAN_POINT('Ctrl Pts',(1.83844662204124,-5.87421791437851,-16.7236372532295));
#60604=CARTESIAN_POINT('Ctrl Pts',(1.86612294571257,-5.8960016303672,-16.7185311380393));
#60605=CARTESIAN_POINT('Ctrl Pts',(1.87511027899495,-5.90137286940024,-16.7174688556403));
#60606=CARTESIAN_POINT('Ctrl Pts',(1.88937385988138,-5.90645548339466,-16.7169970261612));
#60607=CARTESIAN_POINT('Ctrl Pts',(1.89395673353183,-5.9076371554231,-16.7170046598605));
#60608=CARTESIAN_POINT('Ctrl Pts',(1.90144341439914,-5.90878057610348,-16.7172952459867));
#60609=CARTESIAN_POINT('Ctrl Pts',(1.90425145406803,-5.90903727408375,-16.7174650761326));
#60610=CARTESIAN_POINT('Ctrl Pts',(1.90706327644678,-5.90912166928202,-16.7176961632773));
#60611=CARTESIAN_POINT('',(1.62584114411962,-3.94856638716317,-19.7629572175357));
#60612=CARTESIAN_POINT('Origin',(1.62584114411962,-6.18524193534253,-19.0362172778497));
#60613=CARTESIAN_POINT('',(1.33846910697111,-4.22280591656416,-19.6367507067188));
#60614=CARTESIAN_POINT('Origin',(1.63623295246351,-4.23410382602581,-19.6715220966734));
#60615=CARTESIAN_POINT('Origin',(1.33846910697111,-6.17433831723488,-19.0026593919041));
#60616=CARTESIAN_POINT('Origin',(1.62584114411962,-6.18524193534253,-19.0362172778497));
#60617=CARTESIAN_POINT('Origin',(5.83867335851287,-6.34508738889865,-19.5281709987517));
#60618=CARTESIAN_POINT('',(10.3480326234796,-5.24947731735612,-17.7080825054385));
#60619=CARTESIAN_POINT('Ctrl Pts',(10.3480326234796,-5.24947731735612,-17.7080825054385));
#60620=CARTESIAN_POINT('Ctrl Pts',(7.54972025675578,-5.18170180546195,-17.4728227255228));
#60621=CARTESIAN_POINT('Ctrl Pts',(4.7091881268347,-5.11315489305578,-17.233938697471));
#60622=CARTESIAN_POINT('Ctrl Pts',(1.90706327644678,-5.04583540480242,-16.998194874094));
#60623=CARTESIAN_POINT('',(10.0307219562183,-3.98623266785661,-20.8358167812138));
#60624=CARTESIAN_POINT('Origin',(10.0307219562183,-6.50414425974677,-20.0176977116355));
#60625=CARTESIAN_POINT('',(10.3480326234796,-6.16163338174817,-17.4117050340792));
#60626=CARTESIAN_POINT('Origin',(10.0307219562183,-6.50414425974677,-20.0176977116355));
#60627=CARTESIAN_POINT('Ctrl Pts',(1.90706327644678,-5.90912166928201,-16.7176961632773));
#60628=CARTESIAN_POINT('Ctrl Pts',(4.70918812184411,-5.99322580178265,-16.9479863246852));
#60629=CARTESIAN_POINT('Ctrl Pts',(7.54972025123709,-6.07818269341642,-17.1815384272226));
#60630=CARTESIAN_POINT('Ctrl Pts',(10.3480326234796,-6.16163338174816,-17.4117050340792));
#60631=CARTESIAN_POINT('Origin',(10.0411137645622,-6.50453855110077,-20.0189112156446));
#60632=CARTESIAN_POINT('',(10.3388776100546,-4.28306801618089,-20.7791530503061));
#60633=CARTESIAN_POINT('Origin',(10.3388776100546,-6.51583646056242,-20.0536826055992));
#60634=CARTESIAN_POINT('Origin',(10.0411137645622,-4.27177010671924,-20.7443816603515));
#60635=CARTESIAN_POINT('Ctrl Pts',(10.3480326234796,-6.16163338174817,-17.4117050340792));
#60636=CARTESIAN_POINT('Ctrl Pts',(10.3515114639741,-6.16173712700433,-17.4119911754408));
#60637=CARTESIAN_POINT('Ctrl Pts',(10.3549914179992,-6.16156241574048,-17.4123759675224));
#60638=CARTESIAN_POINT('Ctrl Pts',(10.3584662558372,-6.1611090307738,-17.4128588642783));
#60639=CARTESIAN_POINT('Ctrl Pts',(10.367223098271,-6.15996646789746,-17.4140757989961));
#60640=CARTESIAN_POINT('Ctrl Pts',(10.3753630700178,-6.15713972282256,-17.4158312902421));
#60641=CARTESIAN_POINT('Ctrl Pts',(10.3939290316259,-6.14753302482072,-17.4209477623239));
#60642=CARTESIAN_POINT('Ctrl Pts',(10.4035780672155,-6.13952487259413,-17.4246680145472));
#60643=CARTESIAN_POINT('Ctrl Pts',(10.4280013399752,-6.11408837463521,-17.435881088904));
#60644=CARTESIAN_POINT('Ctrl Pts',(10.4407678160189,-6.0930020584574,-17.4444479537232));
#60645=CARTESIAN_POINT('Ctrl Pts',(10.4685456259697,-6.03626400623269,-17.466763669083));
#60646=CARTESIAN_POINT('Ctrl Pts',(10.4828713837316,-5.99063505235357,-17.4838345078959));
#60647=CARTESIAN_POINT('Ctrl Pts',(10.5038238234649,-5.88674071610136,-17.5210208246161));
#60648=CARTESIAN_POINT('Ctrl Pts',(10.5097149363751,-5.83272996465075,-17.5396167538766));
#60649=CARTESIAN_POINT('Ctrl Pts',(10.5152093525458,-5.72672134143419,-17.5750286675881));
#60650=CARTESIAN_POINT('Ctrl Pts',(10.5146501294348,-5.67139291388379,-17.5929043782428));
#60651=CARTESIAN_POINT('Ctrl Pts',(10.5071723447785,-5.56539053344036,-17.6260374509827));
#60652=CARTESIAN_POINT('Ctrl Pts',(10.5000174147823,-5.51115999516812,-17.6424047527202));
#60653=CARTESIAN_POINT('Ctrl Pts',(10.4763655908937,-5.40677101623417,-17.6725219279293));
#60654=CARTESIAN_POINT('Ctrl Pts',(10.4605419031702,-5.36240927189448,-17.6845328147316));
#60655=CARTESIAN_POINT('Ctrl Pts',(10.4319469960435,-5.30950538071611,-17.6978522663517));
#60656=CARTESIAN_POINT('Ctrl Pts',(10.4192298015583,-5.29065702126865,-17.7023303304535));
#60657=CARTESIAN_POINT('Ctrl Pts',(10.3949786188433,-5.26742227944461,-17.7070402629162));
#60658=CARTESIAN_POINT('Ctrl Pts',(10.3846960006403,-5.25993527526373,-17.708325726784));
#60659=CARTESIAN_POINT('Ctrl Pts',(10.3651744504235,-5.25164757219633,-17.7090036066899));
#60660=CARTESIAN_POINT('Ctrl Pts',(10.3566858346072,-5.24968689932439,-17.708809998398));
#60661=CARTESIAN_POINT('Ctrl Pts',(10.3480326234796,-5.24947731735611,-17.7080825054385));
#60662=CARTESIAN_POINT('Origin',(10.3388776100546,-6.51583646056242,-20.0536826055992));
#60663=CARTESIAN_POINT('Origin',(1.05309141530195,-6.89256018399713,-21.2131190072776));
#60664=CARTESIAN_POINT('Origin',(1.63623295246351,-11.7657792816622,-16.1942058835342));
#60665=CARTESIAN_POINT('',(1.90706327644678,-10.0516057316823,-14.6069951093592));
#60666=CARTESIAN_POINT('',(1.90706327644678,-10.7859608904011,-14.0734548558899));
#60667=CARTESIAN_POINT('Ctrl Pts',(1.90706327644678,-10.0516057316823,-14.6069951093592));
#60668=CARTESIAN_POINT('Ctrl Pts',(1.9002587596252,-10.0512733560796,-14.6065011777624));
#60669=CARTESIAN_POINT('Ctrl Pts',(1.89355247272126,-10.0518279831406,-14.6054074046316));
#60670=CARTESIAN_POINT('Ctrl Pts',(1.87725698375413,-10.055232046998,-14.6013332347427));
#60671=CARTESIAN_POINT('Ctrl Pts',(1.86829211419521,-10.0589614875641,-14.5978127562129));
#60672=CARTESIAN_POINT('Ctrl Pts',(1.84706044347989,-10.0712702530579,-14.5870683867584));
#60673=CARTESIAN_POINT('Ctrl Pts',(1.83585892185168,-10.0815819441634,-14.5787550531421));
#60674=CARTESIAN_POINT('Ctrl Pts',(1.80877471345921,-10.1129760302165,-14.5541268705494));
#60675=CARTESIAN_POINT('Ctrl Pts',(1.79294392498965,-10.1410429474189,-14.5329375758434));
#60676=CARTESIAN_POINT('Ctrl Pts',(1.76567283597266,-10.2144033500548,-14.4785632453851));
#60677=CARTESIAN_POINT('Ctrl Pts',(1.75650699269214,-10.2562595787936,-14.4479667279811));
#60678=CARTESIAN_POINT('Ctrl Pts',(1.74778527727007,-10.3184510441819,-14.4026186544858));
#60679=CARTESIAN_POINT('Ctrl Pts',(1.74564598164342,-10.340877007658,-14.3862953920444));
#60680=CARTESIAN_POINT('Ctrl Pts',(1.74342903876676,-10.379743605775,-14.3580271947081));
#60681=CARTESIAN_POINT('Ctrl Pts',(1.74295490171613,-10.3964264560467,-14.3459008172418));
#60682=CARTESIAN_POINT('Ctrl Pts',(1.74292857696575,-10.4295927678057,-14.3218037566102));
#60683=CARTESIAN_POINT('Ctrl Pts',(1.74337239383368,-10.4462099845867,-14.309735850365));
#60684=CARTESIAN_POINT('Ctrl Pts',(1.74549594744656,-10.4847417370586,-14.2817694324065));
#60685=CARTESIAN_POINT('Ctrl Pts',(1.74755180318324,-10.506894590927,-14.265702893341));
#60686=CARTESIAN_POINT('Ctrl Pts',(1.75591196457166,-10.5681486124401,-14.2213535217076));
#60687=CARTESIAN_POINT('Ctrl Pts',(1.76464297432575,-10.6092002023594,-14.1917029071049));
#60688=CARTESIAN_POINT('Ctrl Pts',(1.79360739934097,-10.6912265321601,-14.1332147014375));
#60689=CARTESIAN_POINT('Ctrl Pts',(1.8132284207461,-10.7250788098328,-14.1096237409592));
#60690=CARTESIAN_POINT('Ctrl Pts',(1.84745113279066,-10.7612654174957,-14.085792937811));
#60691=CARTESIAN_POINT('Ctrl Pts',(1.85980439378031,-10.7703887241696,-14.0801722471141));
#60692=CARTESIAN_POINT('Ctrl Pts',(1.87846606193731,-10.7796242046067,-14.075158242655));
#60693=CARTESIAN_POINT('Ctrl Pts',(1.88517766043124,-10.7821409674902,-14.0739697528521));
#60694=CARTESIAN_POINT('Ctrl Pts',(1.89712731920749,-10.7849686486889,-14.0731201278134));
#60695=CARTESIAN_POINT('Ctrl Pts',(1.90207774197533,-10.7856919622337,-14.0731114184831));
#60696=CARTESIAN_POINT('Ctrl Pts',(1.90706327644678,-10.7859608904011,-14.0734548558899));
#60697=CARTESIAN_POINT('',(1.62584114411962,-9.86239943185911,-17.5755151259486));
#60698=CARTESIAN_POINT('Origin',(1.62584114411962,-11.7650292949391,-16.1931736153679));
#60699=CARTESIAN_POINT('',(1.33846910697111,-10.0842167666784,-17.3707409263229));
#60700=CARTESIAN_POINT('Origin',(1.63623295246351,-10.1057066675065,-17.4003192372954));
#60701=CARTESIAN_POINT('Origin',(1.33846910697111,-11.7442893808342,-16.1646275725617));
#60702=CARTESIAN_POINT('Origin',(1.62584114411962,-11.7650292949391,-16.1931736153679));
#60703=CARTESIAN_POINT('Origin',(5.83867335851287,-12.0690734153485,-16.611654445725));
#60704=CARTESIAN_POINT('',(10.3480326234796,-10.4646480417893,-15.2192095552406));
#60705=CARTESIAN_POINT('Ctrl Pts',(10.3480326234796,-10.4646480417893,-15.2192095552406));
#60706=CARTESIAN_POINT('Ctrl Pts',(7.54753623341466,-10.3273833808683,-15.0162497111978));
#60707=CARTESIAN_POINT('Ctrl Pts',(4.70781617470128,-10.1884122025895,-14.8102983544992));
#60708=CARTESIAN_POINT('Ctrl Pts',(1.90706327644678,-10.0516057316823,-14.6069951093592));
#60709=CARTESIAN_POINT('',(10.0307219562183,-10.2297540313114,-18.584225684205));
#60710=CARTESIAN_POINT('Origin',(10.0307219562183,-12.3716175623118,-17.0280707397496));
#60711=CARTESIAN_POINT('',(10.3480326234796,-11.2405743353076,-14.655466104402));
#60712=CARTESIAN_POINT('Origin',(10.0307219562183,-12.3716175623118,-17.0280707397496));
#60713=CARTESIAN_POINT('Ctrl Pts',(1.90706327644678,-10.7859608904011,-14.0734548558899));
#60714=CARTESIAN_POINT('Ctrl Pts',(4.70781616958245,-10.9370382417485,-14.2663896989247));
#60715=CARTESIAN_POINT('Ctrl Pts',(7.54753622799762,-11.0899651657448,-14.4622016128173));
#60716=CARTESIAN_POINT('Ctrl Pts',(10.3480326234796,-11.2405743353076,-14.655466104402));
#60717=CARTESIAN_POINT('Origin',(10.0411137645622,-12.3723675490348,-17.0291030079158));
#60718=CARTESIAN_POINT('',(10.3388776100546,-10.4945511677868,-18.4386081065242));
#60719=CARTESIAN_POINT('Origin',(10.3388776100546,-12.3938574498629,-17.0586813188882));
#60720=CARTESIAN_POINT('Origin',(10.0411137645622,-10.4730612669588,-18.4090297955518));
#60721=CARTESIAN_POINT('Ctrl Pts',(10.3480326234796,-11.2405743353076,-14.655466104402));
#60722=CARTESIAN_POINT('Ctrl Pts',(10.3515211595623,-11.2407619468765,-14.6557068510616));
#60723=CARTESIAN_POINT('Ctrl Pts',(10.3550011198928,-11.2407133851835,-14.656127803182));
#60724=CARTESIAN_POINT('Ctrl Pts',(10.3584662558372,-11.2404322010368,-14.6567254954937));
#60725=CARTESIAN_POINT('Ctrl Pts',(10.3671694892744,-11.2397259628669,-14.658226693656));
#60726=CARTESIAN_POINT('Ctrl Pts',(10.3753654465597,-11.2375879642563,-14.6607699081134));
#60727=CARTESIAN_POINT('Ctrl Pts',(10.3941492137284,-11.2299109713814,-14.6687216746163));
#60728=CARTESIAN_POINT('Ctrl Pts',(10.404002965845,-11.2232825987702,-14.6748808959337));
#60729=CARTESIAN_POINT('Ctrl Pts',(10.4308436412037,-11.2002100598277,-14.695462505518));
#60730=CARTESIAN_POINT('Ctrl Pts',(10.4443760953691,-11.1799381757228,-14.7123773258611));
#60731=CARTESIAN_POINT('Ctrl Pts',(10.4751024728255,-11.1253565526287,-14.7571304838428));
#60732=CARTESIAN_POINT('Ctrl Pts',(10.4913920727398,-11.0748241683189,-14.7969697951178));
#60733=CARTESIAN_POINT('Ctrl Pts',(10.5062952995223,-10.9899781948954,-14.8615728881703));
#60734=CARTESIAN_POINT('Ctrl Pts',(10.5095242362634,-10.9629200882247,-14.8818952699719));
#60735=CARTESIAN_POINT('Ctrl Pts',(10.512859180135,-10.9184305611832,-14.914906904102));
#60736=CARTESIAN_POINT('Ctrl Pts',(10.5136719991087,-10.9006780007669,-14.9279744210185));
#60737=CARTESIAN_POINT('Ctrl Pts',(10.514295657022,-10.8670882523061,-14.9525087414765));
#60738=CARTESIAN_POINT('Ctrl Pts',(10.5142026737932,-10.8511355186812,-14.9640796299257));
#60739=CARTESIAN_POINT('Ctrl Pts',(10.5131483322071,-10.816105099928,-14.9893112870103));
#60740=CARTESIAN_POINT('Ctrl Pts',(10.512009812725,-10.7968758883504,-15.0030451759508));
#60741=CARTESIAN_POINT('Ctrl Pts',(10.5074172692912,-10.7460384791957,-15.0390378011656));
#60742=CARTESIAN_POINT('Ctrl Pts',(10.5028514263372,-10.7137256630153,-15.0615825002595));
#60743=CARTESIAN_POINT('Ctrl Pts',(10.4823258875198,-10.6159756467573,-15.1286103745228));
#60744=CARTESIAN_POINT('Ctrl Pts',(10.4610892332284,-10.5615248358073,-15.164262671718));
#60745=CARTESIAN_POINT('Ctrl Pts',(10.4253700252928,-10.510326200914,-15.1959357631404));
#60746=CARTESIAN_POINT('Ctrl Pts',(10.4122912190474,-10.4944454192633,-15.2055154329317));
#60747=CARTESIAN_POINT('Ctrl Pts',(10.3868737804667,-10.476241943114,-15.2153586960742));
#60748=CARTESIAN_POINT('Ctrl Pts',(10.3771760707495,-10.4710384088583,-15.2179090290457));
#60749=CARTESIAN_POINT('Ctrl Pts',(10.3604838650278,-10.4660465521434,-15.219570037764));
#60750=CARTESIAN_POINT('Ctrl Pts',(10.35429238307,-10.4649548601736,-15.2196632176109));
#60751=CARTESIAN_POINT('Ctrl Pts',(10.3480326234796,-10.4646480417893,-15.2192095552406));
#60752=CARTESIAN_POINT('Origin',(10.3388776100546,-12.3938574498629,-17.0586813188882));
#60753=CARTESIAN_POINT('Origin',(1.05309141530195,-13.110428553894,-18.0449568312087));
#60754=CARTESIAN_POINT('Origin',(1.63623295246351,-16.1942058835342,-11.7657792816622));
#60755=CARTESIAN_POINT('',(1.90706327644678,-14.0734548558899,-10.7859608904011));
#60756=CARTESIAN_POINT('',(1.90706327644678,-14.6069951093592,-10.0516057316823));
#60757=CARTESIAN_POINT('Ctrl Pts',(1.90706327644678,-14.0734548558899,-10.7859608904011));
#60758=CARTESIAN_POINT('Ctrl Pts',(1.90025875961848,-14.0729861146492,-10.7855938432467));
#60759=CARTESIAN_POINT('Ctrl Pts',(1.89355247271066,-14.0731756018459,-10.7843822139931));
#60760=CARTESIAN_POINT('Ctrl Pts',(1.87725698375402,-14.0751540712246,-10.7794555345929));
#60761=CARTESIAN_POINT('Ctrl Pts',(1.86829211419516,-14.077613092283,-10.7749549000324));
#60762=CARTESIAN_POINT('Ctrl Pts',(1.84706044347966,-14.0859992311583,-10.7609327797316));
#60763=CARTESIAN_POINT('Ctrl Pts',(1.83585892185142,-14.0932372708109,-10.7498398418313));
#60764=CARTESIAN_POINT('Ctrl Pts',(1.80877471345869,-14.1154842939635,-10.7167157421783));
#60765=CARTESIAN_POINT('Ctrl Pts',(1.79294392498917,-14.1356296662984,-10.6878903709769));
#60766=CARTESIAN_POINT('Ctrl Pts',(1.76567283597247,-14.1885969630937,-10.6135076985469));
#60767=CARTESIAN_POINT('Ctrl Pts',(1.75650699269204,-14.2189497583366,-10.5714743952933));
#60768=CARTESIAN_POINT('Ctrl Pts',(1.74778527727004,-14.2640840313798,-10.5091275947843));
#60769=CARTESIAN_POINT('Ctrl Pts',(1.7456459816434,-14.2803682245799,-10.4866732458429));
#60770=CARTESIAN_POINT('Ctrl Pts',(1.74342903876677,-14.3085972026078,-10.4477781532309));
#60771=CARTESIAN_POINT('Ctrl Pts',(1.74295490171612,-14.3207162793517,-10.431089998674));
#60772=CARTESIAN_POINT('Ctrl Pts',(1.74292857696575,-14.3448129150223,-10.3979233781621));
#60773=CARTESIAN_POINT('Ctrl Pts',(1.7433723938337,-14.3568876392082,-10.3813111149051));
#60774=CARTESIAN_POINT('Ctrl Pts',(1.74549594744658,-14.3848914150599,-10.3428065045314));
#60775=CARTESIAN_POINT('Ctrl Pts',(1.74755180318328,-14.4009951974739,-10.3206807095395));
#60776=CARTESIAN_POINT('Ctrl Pts',(1.75591196457177,-14.4455465242589,-10.2595734170325));
#60777=CARTESIAN_POINT('Ctrl Pts',(1.76464297432594,-14.4754263625501,-10.2186883678711));
#60778=CARTESIAN_POINT('Ctrl Pts',(1.79360739934174,-14.5353641884939,-10.1377152488489));
#60779=CARTESIAN_POINT('Ctrl Pts',(1.81322842074722,-14.5602696100643,-10.1048179830617));
#60780=CARTESIAN_POINT('Ctrl Pts',(1.84745113279294,-14.5873209959229,-10.0709712657018));
#60781=CARTESIAN_POINT('Ctrl Pts',(1.85980439378218,-14.5942608872388,-10.0628064143825));
#60782=CARTESIAN_POINT('Ctrl Pts',(1.87846606193786,-14.6014949385014,-10.0551838923634));
#60783=CARTESIAN_POINT('Ctrl Pts',(1.88517766043167,-14.6035212586948,-10.05327584889));
#60784=CARTESIAN_POINT('Ctrl Pts',(1.89712731918627,-14.6059479947446,-10.0515940059186));
#60785=CARTESIAN_POINT('Ctrl Pts',(1.90207774196103,-14.6066332154769,-10.0513622066719));
#60786=CARTESIAN_POINT('Ctrl Pts',(1.90706327644678,-14.6069951093592,-10.0516057316823));
#60787=CARTESIAN_POINT('',(1.62584114411962,-14.8108321047873,-13.6676591580191));
#60788=CARTESIAN_POINT('Origin',(1.62584114411962,-16.1931736153679,-11.7650292949391));
#60789=CARTESIAN_POINT('',(1.33846910697111,-14.9585142188006,-13.4043619949899));
#60790=CARTESIAN_POINT('Origin',(1.63623295246351,-14.988092529773,-13.425851895818));
#60791=CARTESIAN_POINT('Origin',(1.33846910697111,-16.1646275725618,-11.7442893808342));
#60792=CARTESIAN_POINT('Origin',(1.62584114411962,-16.1931736153679,-11.7650292949391));
#60793=CARTESIAN_POINT('Origin',(5.83867335851287,-16.611654445725,-12.0690734153485));
#60794=CARTESIAN_POINT('',(10.3480326234796,-14.655466104402,-11.2405743353076));
#60795=CARTESIAN_POINT('Ctrl Pts',(10.3480326234796,-14.655466104402,-11.2405743353076));
#60796=CARTESIAN_POINT('Ctrl Pts',(7.54753623341466,-14.4622016131911,-11.0899651660361));
#60797=CARTESIAN_POINT('Ctrl Pts',(4.70781617470128,-14.2663896992774,-10.9370382420246));
#60798=CARTESIAN_POINT('Ctrl Pts',(1.90706327644678,-14.0734548558899,-10.7859608904011));
#60799=CARTESIAN_POINT('',(10.0307219562183,-15.4719157952941,-14.5134810933121));
#60800=CARTESIAN_POINT('Origin',(10.0307219562183,-17.0280707397496,-12.3716175623118));
#60801=CARTESIAN_POINT('',(10.3480326234796,-15.2192095552406,-10.4646480417893));
#60802=CARTESIAN_POINT('Origin',(10.0307219562183,-17.0280707397496,-12.3716175623118));
#60803=CARTESIAN_POINT('Ctrl Pts',(1.90706327644678,-14.6069951093592,-10.0516057316823));
#60804=CARTESIAN_POINT('Ctrl Pts',(4.70781616958245,-14.8102983541277,-10.1884122023394));
#60805=CARTESIAN_POINT('Ctrl Pts',(7.54753622799763,-15.0162497108052,-10.3273833806028));
#60806=CARTESIAN_POINT('Ctrl Pts',(10.3480326234796,-15.2192095552406,-10.4646480417893));
#60807=CARTESIAN_POINT('Origin',(10.0411137645622,-17.0291030079158,-12.3723675490348));
#60808=CARTESIAN_POINT('',(10.3388776100546,-15.6787545312522,-14.293163731939));
#60809=CARTESIAN_POINT('Origin',(10.3388776100546,-17.0586813188882,-12.3938574498629));
#60810=CARTESIAN_POINT('Origin',(10.0411137645622,-15.6491762202798,-14.2716738311109));
#60811=CARTESIAN_POINT('Ctrl Pts',(10.3480326234796,-15.2192095552406,-10.4646480417893));
#60812=CARTESIAN_POINT('Ctrl Pts',(10.3515211595623,-15.2194623792549,-10.4648190303056));
#60813=CARTESIAN_POINT('Ctrl Pts',(10.3550011198928,-15.2195462756993,-10.4652343859512));
#60814=CARTESIAN_POINT('Ctrl Pts',(10.3584662558372,-15.219463550766,-10.4658897157988));
#60815=CARTESIAN_POINT('Ctrl Pts',(10.3671694892744,-15.2192557740965,-10.46753567969));
#60816=CARTESIAN_POINT('Ctrl Pts',(10.3753654465596,-15.2180083130739,-10.4706150982766));
#60817=CARTESIAN_POINT('Ctrl Pts',(10.3941492137284,-15.2131642899593,-10.4805499988893));
#60818=CARTESIAN_POINT('Ctrl Pts',(10.4040029658451,-15.2087636370541,-10.4884560462405));
#60819=CARTESIAN_POINT('Ctrl Pts',(10.4308436412037,-15.1931804156785,-10.515160126788));
#60820=CARTESIAN_POINT('Ctrl Pts',(10.4443760953691,-15.1791276751458,-10.5375114335937));
#60821=CARTESIAN_POINT('Ctrl Pts',(10.4751024728251,-15.1410469532011,-10.5969408652328));
#60822=CARTESIAN_POINT('Ctrl Pts',(10.4913920727396,-15.1052988240478,-10.6504456673432));
#60823=CARTESIAN_POINT('Ctrl Pts',(10.5062952995223,-15.0445689617834,-10.7381057076571));
#60824=CARTESIAN_POINT('Ctrl Pts',(10.5095242362634,-15.0251151344584,-10.7657948560931));
#60825=CARTESIAN_POINT('Ctrl Pts',(10.512859180135,-14.9930042358172,-10.8109388057734));
#60826=CARTESIAN_POINT('Ctrl Pts',(10.5136719991087,-14.9801586323538,-10.8288525957508));
#60827=CARTESIAN_POINT('Ctrl Pts',(10.514295657022,-14.9557944051667,-10.8625659242062));
#60828=CARTESIAN_POINT('Ctrl Pts',(10.5142026737932,-14.9441980550707,-10.8785001588622));
#60829=CARTESIAN_POINT('Ctrl Pts',(10.5131483322071,-14.9186791578821,-10.9133218854645));
#60830=CARTESIAN_POINT('Ctrl Pts',(10.512009812725,-14.9046350959894,-10.9323257432013));
#60831=CARTESIAN_POINT('Ctrl Pts',(10.5074172692912,-14.867408179605,-10.982266387329));
#60832=CARTESIAN_POINT('Ctrl Pts',(10.5028514263372,-14.8436435603699,-11.0136928796461));
#60833=CARTESIAN_POINT('Ctrl Pts',(10.4823258875198,-14.7713905226837,-11.107646592462));
#60834=CARTESIAN_POINT('Ctrl Pts',(10.4610892332283,-14.730621889834,-11.1583801679714));
#60835=CARTESIAN_POINT('Ctrl Pts',(10.4253700252925,-14.691716618007,-11.204324316231));
#60836=CARTESIAN_POINT('Ctrl Pts',(10.4122912190472,-14.6795733779005,-11.2183425550237));
#60837=CARTESIAN_POINT('Ctrl Pts',(10.3868737804665,-14.6653025788806,-11.2333292380638));
#60838=CARTESIAN_POINT('Ctrl Pts',(10.3771760707494,-14.6611418199486,-11.2373627293707));
#60839=CARTESIAN_POINT('Ctrl Pts',(10.3604838650279,-14.6569075620133,-11.2404850110942));
#60840=CARTESIAN_POINT('Ctrl Pts',(10.35429238307,-14.6558980954078,-11.2409109817661));
#60841=CARTESIAN_POINT('Ctrl Pts',(10.3480326234796,-14.655466104402,-11.2405743353076));
#60842=CARTESIAN_POINT('Origin',(10.3388776100546,-17.0586813188882,-12.3938574498629));
#60843=CARTESIAN_POINT('Origin',(1.05309141530195,-18.0449568312087,-13.110428553894));
#60844=CARTESIAN_POINT('Origin',(1.63623295246351,-19.0374307818588,-6.18563622669653));
#60845=CARTESIAN_POINT('',(1.90706327644678,-16.7176961632773,-5.90912166928202));
#60846=CARTESIAN_POINT('',(1.90706327644678,-16.998194874094,-5.04583540480242));
#60847=CARTESIAN_POINT('Ctrl Pts',(1.90706327644678,-16.7176961632773,-5.90912166928201));
#60848=CARTESIAN_POINT('Ctrl Pts',(1.90026014389714,-16.717137053823,-5.90891747725169));
#60849=CARTESIAN_POINT('Ctrl Pts',(1.89355517776701,-16.7169428161621,-5.90770704485632));
#60850=CARTESIAN_POINT('Ctrl Pts',(1.87732280058942,-16.7173002954459,-5.90243158644649));
#60851=CARTESIAN_POINT('Ctrl Pts',(1.86840987580623,-16.7182373577841,-5.89743569235106));
#60852=CARTESIAN_POINT('Ctrl Pts',(1.84749974153975,-16.7218050267903,-5.8818060876946));
#60853=CARTESIAN_POINT('Ctrl Pts',(1.83650132566953,-16.7251494451274,-5.86939109701621));
#60854=CARTESIAN_POINT('Ctrl Pts',(1.81085694928113,-16.7353298338013,-5.83352153589242));
#60855=CARTESIAN_POINT('Ctrl Pts',(1.79594323550174,-16.7445431753862,-5.80312318642017));
#60856=CARTESIAN_POINT('Ctrl Pts',(1.7690253946807,-16.7696407324898,-5.72294526487633));
#60857=CARTESIAN_POINT('Ctrl Pts',(1.75949337448575,-16.7845442855164,-5.67650047046933));
#60858=CARTESIAN_POINT('Ctrl Pts',(1.74741836256371,-16.8126766692638,-5.58926584375973));
#60859=CARTESIAN_POINT('Ctrl Pts',(1.74418490387274,-16.826978706391,-5.54515926519339));
#60860=CARTESIAN_POINT('Ctrl Pts',(1.74230474178711,-16.854826554809,-5.45939048647927));
#60861=CARTESIAN_POINT('Ctrl Pts',(1.74356051202792,-16.8689635910099,-5.41590892159206));
#60862=CARTESIAN_POINT('Ctrl Pts',(1.75089245923138,-16.8971914959603,-5.32933507280615));
#60863=CARTESIAN_POINT('Ctrl Pts',(1.75736442403639,-16.912046937198,-5.28389327657113));
#60864=CARTESIAN_POINT('Ctrl Pts',(1.77948145071148,-16.9432828393377,-5.18955296706125));
#60865=CARTESIAN_POINT('Ctrl Pts',(1.79536357091766,-16.9576377997409,-5.14706849481589));
#60866=CARTESIAN_POINT('Ctrl Pts',(1.82385809602965,-16.974876563837,-5.09851442742741));
#60867=CARTESIAN_POINT('Ctrl Pts',(1.83844662203937,-16.9824854044475,-5.07756522074617));
#60868=CARTESIAN_POINT('Ctrl Pts',(1.86612294570897,-16.9911586174818,-5.05694052510463));
#60869=CARTESIAN_POINT('Ctrl Pts',(1.87511027899214,-16.9934563480587,-5.05197070751723));
#60870=CARTESIAN_POINT('Ctrl Pts',(1.88937385987974,-16.996062115541,-5.04758145200968));
#60871=CARTESIAN_POINT('Ctrl Pts',(1.89395673353061,-16.996762860725,-5.0466299462326));
#60872=CARTESIAN_POINT('Ctrl Pts',(1.90144341428987,-16.9976700356394,-5.04587570172071));
#60873=CARTESIAN_POINT('Ctrl Pts',(1.90425145398682,-16.9979583144071,-5.0457678523345));
#60874=CARTESIAN_POINT('Ctrl Pts',(1.90706327644678,-16.998194874094,-5.04583540480242));
#60875=CARTESIAN_POINT('',(1.62584114411962,-18.3094773381637,-8.42191748352189));
#60876=CARTESIAN_POINT('Origin',(1.62584114411962,-19.0362172778497,-6.18524193534253));
#60877=CARTESIAN_POINT('',(1.33846910697111,-18.3685680770895,-8.12587071790561));
#60878=CARTESIAN_POINT('Origin',(1.63623295246351,-18.4033394670442,-8.13716862736726));
#60879=CARTESIAN_POINT('Origin',(1.33846910697111,-19.0026593919042,-6.17433831723488));
#60880=CARTESIAN_POINT('Origin',(1.62584114411962,-19.0362172778497,-6.18524193534253));
#60881=CARTESIAN_POINT('Origin',(5.83867335851287,-19.5281709987517,-6.34508738889865));
#60882=CARTESIAN_POINT('',(10.3480326234796,-17.4117050340792,-6.16163338174818));
#60883=CARTESIAN_POINT('Ctrl Pts',(10.3480326234796,-17.4117050340792,-6.16163338174816));
#60884=CARTESIAN_POINT('Ctrl Pts',(7.54972025675579,-17.1815384276765,-6.078182693581));
#60885=CARTESIAN_POINT('Ctrl Pts',(4.7091881268347,-16.9479863250953,-5.99322580193243));
#60886=CARTESIAN_POINT('Ctrl Pts',(1.90706327644678,-16.7176961632773,-5.90912166928201));
#60887=CARTESIAN_POINT('',(10.0307219562183,-19.1995786420573,-9.02205585163692));
#60888=CARTESIAN_POINT('Origin',(10.0307219562183,-20.0176977116355,-6.50414425974676));
#60889=CARTESIAN_POINT('',(10.3480326234796,-17.7080825054385,-5.2494773173561));
#60890=CARTESIAN_POINT('Origin',(10.0307219562183,-20.0176977116355,-6.50414425974676));
#60891=CARTESIAN_POINT('Ctrl Pts',(1.90706327644677,-16.998194874094,-5.04583540480242));
#60892=CARTESIAN_POINT('Ctrl Pts',(4.70918812184411,-17.2339386970511,-5.11315489293588));
#60893=CARTESIAN_POINT('Ctrl Pts',(7.54972025123708,-17.4728227250588,-5.18170180532828));
#60894=CARTESIAN_POINT('Ctrl Pts',(10.3480326234796,-17.7080825054385,-5.24947731735612));
#60895=CARTESIAN_POINT('Origin',(10.0411137645622,-20.0189112156446,-6.50453855110076));
#60896=CARTESIAN_POINT('',(10.3388776100546,-19.3282121608924,-8.74860490494395));
#60897=CARTESIAN_POINT('Origin',(10.3388776100546,-20.0536826055992,-6.51583646056242));
#60898=CARTESIAN_POINT('Origin',(10.0411137645622,-19.2934407709377,-8.73730699548229));
#60899=CARTESIAN_POINT('Ctrl Pts',(10.3480326234796,-17.7080825054385,-5.24947731735613));
#60900=CARTESIAN_POINT('Ctrl Pts',(10.3515114639741,-17.7083749785944,-5.24956157535324));
#60901=CARTESIAN_POINT('Ctrl Pts',(10.3549914179992,-17.7085835892234,-5.24992909484554));
#60902=CARTESIAN_POINT('Ctrl Pts',(10.3584662558372,-17.7087077679084,-5.25057973058011));
#60903=CARTESIAN_POINT('Ctrl Pts',(10.367223098271,-17.7090207071676,-5.2522193796443));
#60904=CARTESIAN_POINT('Ctrl Pts',(10.3753630700179,-17.708779410352,-5.25553811631361));
#60905=CARTESIAN_POINT('Ctrl Pts',(10.3939290316259,-17.7072720478088,-5.26631748509035));
#60906=CARTESIAN_POINT('Ctrl Pts',(10.4035780672154,-17.705574721304,-5.27498292572684));
#60907=CARTESIAN_POINT('Ctrl Pts',(10.4280013399751,-17.6996950906475,-5.30215236459276));
#60908=CARTESIAN_POINT('Ctrl Pts',(10.4407678160189,-17.6942316042004,-5.32424702952846));
#60909=CARTESIAN_POINT('Ctrl Pts',(10.4685456259701,-17.6789356068263,-5.38326592638971));
#60910=CARTESIAN_POINT('Ctrl Pts',(10.4828713837318,-17.6659261793664,-5.43021451281232));
#60911=CARTESIAN_POINT('Ctrl Pts',(10.5038238234649,-17.6349429829058,-5.53612436501357));
#60912=CARTESIAN_POINT('Ctrl Pts',(10.5097149363751,-17.6182406825358,-5.59075039378804));
#60913=CARTESIAN_POINT('Ctrl Pts',(10.5152093525458,-17.5845792171893,-5.6973277721556));
#60914=CARTESIAN_POINT('Ctrl Pts',(10.5146501294348,-17.5665197371488,-5.75259648941304));
#60915=CARTESIAN_POINT('Ctrl Pts',(10.5071723447785,-17.5310183201387,-5.85782934815568));
#60916=CARTESIAN_POINT('Ctrl Pts',(10.5000174147823,-17.5123838347761,-5.91132323381308));
#60917=CARTESIAN_POINT('Ctrl Pts',(10.4763655908938,-17.4753908390237,-6.01347812322457));
#60918=CARTESIAN_POINT('Ctrl Pts',(10.4605419031703,-17.4590326714754,-6.05642735042495));
#60919=CARTESIAN_POINT('Ctrl Pts',(10.4319469960435,-17.4387122071681,-6.10705647468782));
#60920=CARTESIAN_POINT('Ctrl Pts',(10.4192298015583,-17.4312562494153,-6.12493725783481));
#60921=CARTESIAN_POINT('Ctrl Pts',(10.3949786188434,-17.421409626235,-6.14650298767117));
#60922=CARTESIAN_POINT('Ctrl Pts',(10.3846960006404,-17.4180488377084,-6.15331567799441));
#60923=CARTESIAN_POINT('Ctrl Pts',(10.3651744504234,-17.4137258644339,-6.16041901843185));
#60924=CARTESIAN_POINT('Ctrl Pts',(10.3566858346071,-17.4124167774369,-6.16189143600688));
#60925=CARTESIAN_POINT('Ctrl Pts',(10.3480326234796,-17.4117050340792,-6.16163338174816));
#60926=CARTESIAN_POINT('Origin',(10.3388776100546,-20.0536826055992,-6.51583646056242));
#60927=CARTESIAN_POINT('Origin',(1.05309141530195,-21.2131190072776,-6.89256018399713));
#60928=CARTESIAN_POINT('Origin',(1.63623295246351,-20.0171393136753,2.45139255885791E-15));
#60929=CARTESIAN_POINT('',(1.90706327644678,-17.7254928911647,-0.45385644790204));
#60930=CARTESIAN_POINT('',(1.74294142833529,-17.7169435737505,-2.14581750869533E-15));
#60931=CARTESIAN_POINT('Ctrl Pts',(1.90706327644678,-17.7254928911647,-0.453856447902031));
#60932=CARTESIAN_POINT('Ctrl Pts',(1.90025953246662,-17.724897994206,-0.453835022138628));
#60933=CARTESIAN_POINT('Ctrl Pts',(1.89355398298092,-17.7243391729788,-0.452743661105513));
#60934=CARTESIAN_POINT('Ctrl Pts',(1.87729436838523,-17.7230467959919,-0.447606881401877));
#60935=CARTESIAN_POINT('Ctrl Pts',(1.86835902888825,-17.7223927114579,-0.442546314020724));
#60936=CARTESIAN_POINT('Ctrl Pts',(1.84731494009872,-17.7209473414005,-0.426450928591829));
#60937=CARTESIAN_POINT('Ctrl Pts',(1.83623221810314,-17.7202879485126,-0.413449286577364));
#60938=CARTESIAN_POINT('Ctrl Pts',(1.81006546585599,-17.7188609517425,-0.375219786699082));
#60939=CARTESIAN_POINT('Ctrl Pts',(1.79484445174597,-17.7182253713051,-0.342313735261879));
#60940=CARTESIAN_POINT('Ctrl Pts',(1.76839326635594,-17.7173517778109,-0.257598032761879));
#60941=CARTESIAN_POINT('Ctrl Pts',(1.75921616149792,-17.7171803340553,-0.210107900641706));
#60942=CARTESIAN_POINT('Ctrl Pts',(1.74822227890673,-17.7169975657511,-0.126194388047674));
#60943=CARTESIAN_POINT('Ctrl Pts',(1.74516474660383,-17.716966780863,-0.0869626247243486));
#60944=CARTESIAN_POINT('Ctrl Pts',(1.74322632212065,-17.7169463353311,-0.0322901899044937));
#60945=CARTESIAN_POINT('Ctrl Pts',(1.74294142833529,-17.7169435737505,-0.0161499715374775));
#60946=CARTESIAN_POINT('Ctrl Pts',(1.74294142833529,-17.7169435737505,-2.12193519356389E-15));
#60947=CARTESIAN_POINT('',(1.62584114411962,-20.0158633600508,-2.35177984678801));
#60948=CARTESIAN_POINT('Origin',(1.62584114411962,-20.0158633600508,2.59524128268911E-15));
#60949=CARTESIAN_POINT('',(1.33846910697111,-19.9805785106537,-2.05196259868229));
#60950=CARTESIAN_POINT('Origin',(1.63623295246351,-20.0171393136753,-2.05196259868229));
#60951=CARTESIAN_POINT('Origin',(1.33846910697111,-19.9805785106537,2.44691515181845E-15));
#60952=CARTESIAN_POINT('',(1.90706327644678,-17.7254928911647,0.453856447902042));
#60953=CARTESIAN_POINT('Origin',(1.62584114411962,-20.0158633600508,2.59524128268911E-15));
#60954=CARTESIAN_POINT('Ctrl Pts',(1.74294142833529,-17.7169435737505,-2.12193519356389E-15));
#60955=CARTESIAN_POINT('Ctrl Pts',(1.74294142833529,-17.7169435737505,0.0201863215634263));
#60956=CARTESIAN_POINT('Ctrl Pts',(1.74338651205543,-17.7169478157426,0.0403878807305028));
#60957=CARTESIAN_POINT('Ctrl Pts',(1.74602547045637,-17.71697649914,0.0996677434220068));
#60958=CARTESIAN_POINT('Ctrl Pts',(1.74954197522247,-17.7170140039981,0.139554220977233));
#60959=CARTESIAN_POINT('Ctrl Pts',(1.76185308853428,-17.7172332241403,0.22475627680889));
#60960=CARTESIAN_POINT('Ctrl Pts',(1.77207894319479,-17.7174389665533,0.273353606347227));
#60961=CARTESIAN_POINT('Ctrl Pts',(1.79824775576829,-17.7183749061737,0.348923678367247));
#60962=CARTESIAN_POINT('Ctrl Pts',(1.8132178609837,-17.7189861130439,0.382374164870467));
#60963=CARTESIAN_POINT('Ctrl Pts',(1.8456481530249,-17.7208443091635,0.424859842185486));
#60964=CARTESIAN_POINT('Ctrl Pts',(1.85822154357183,-17.7216651227597,0.436125221547159));
#60965=CARTESIAN_POINT('Ctrl Pts',(1.87729261989249,-17.7230568968888,0.447206202216915));
#60966=CARTESIAN_POINT('Ctrl Pts',(1.88421421928237,-17.7235877581235,0.450152284724024));
#60967=CARTESIAN_POINT('Ctrl Pts',(1.89663970733258,-17.7245977295699,0.453190575625263));
#60968=CARTESIAN_POINT('Ctrl Pts',(1.90183077488345,-17.7250353784665,0.453839970159655));
#60969=CARTESIAN_POINT('Ctrl Pts',(1.90706327644678,-17.7254928911647,0.453856447902032));
#60970=CARTESIAN_POINT('Origin',(5.83867335851287,-20.5331341136527,2.51458369687481E-15));
#60971=CARTESIAN_POINT('',(10.3480326234796,-18.4635649605383,-0.479548822159046));
#60972=CARTESIAN_POINT('Ctrl Pts',(10.3480326234796,-18.4635649605383,-0.479548822159038));
#60973=CARTESIAN_POINT('Ctrl Pts',(7.55083071619378,-18.2189729292873,-0.471311164566919));
#60974=CARTESIAN_POINT('Ctrl Pts',(4.70971831191321,-17.9705478141232,-0.462682327280518));
#60975=CARTESIAN_POINT('Ctrl Pts',(1.90706327644678,-17.7254928911647,-0.453856447902025));
#60976=CARTESIAN_POINT('',(10.0307219562183,-21.0478529600056,-2.64748892284414));
#60977=CARTESIAN_POINT('Origin',(10.0307219562183,-21.0478529600056,2.73973051739646E-15));
#60978=CARTESIAN_POINT('',(10.3480326234796,-18.4635649605383,0.479548822159051));
#60979=CARTESIAN_POINT('Origin',(10.0307219562183,-21.0478529600056,2.73973051739646E-15));
#60980=CARTESIAN_POINT('Ctrl Pts',(1.90706327644678,-17.7254928911647,0.453856447902027));
#60981=CARTESIAN_POINT('Ctrl Pts',(4.70971830698341,-17.9705478136921,0.462682327264996));
#60982=CARTESIAN_POINT('Ctrl Pts',(7.55083071063942,-18.2189729288016,0.471311164550564));
#60983=CARTESIAN_POINT('Ctrl Pts',(10.3480326234796,-18.4635649605383,0.479548822159041));
#60984=CARTESIAN_POINT('Origin',(10.0411137645622,-21.0491289136301,2.57777483489171E-15));
#60985=CARTESIAN_POINT('',(10.3388776100546,-21.0856897166516,-2.34767167473842));
#60986=CARTESIAN_POINT('Origin',(10.3388776100546,-21.0856897166516,2.58225224193117E-15));
#60987=CARTESIAN_POINT('Origin',(10.0411137645622,-21.0491289136301,-2.34767167473842));
#60988=CARTESIAN_POINT('',(10.5141690094812,-18.4843265523066,-4.2099725767245E-15));
#60989=CARTESIAN_POINT('Ctrl Pts',(10.5141690094812,-18.4843265523066,-6.15626801878132E-15));
#60990=CARTESIAN_POINT('Ctrl Pts',(10.5141690094812,-18.4843265523066,-0.0320800754047132));
#60991=CARTESIAN_POINT('Ctrl Pts',(10.5131416010228,-18.4841520360016,-0.0648143219529833));
#60992=CARTESIAN_POINT('Ctrl Pts',(10.5083046161227,-18.4833464708957,-0.137261078256609));
#60993=CARTESIAN_POINT('Ctrl Pts',(10.503879825914,-18.4826118937437,-0.178099201717497));
#60994=CARTESIAN_POINT('Ctrl Pts',(10.4867651973882,-18.479909817102,-0.28011633465905));
#60995=CARTESIAN_POINT('Ctrl Pts',(10.4718859508698,-18.4776521193349,-0.334420796175788));
#60996=CARTESIAN_POINT('Ctrl Pts',(10.4435576763644,-18.4738593034484,-0.398681362505428));
#60997=CARTESIAN_POINT('Ctrl Pts',(10.429285329043,-18.4719918118745,-0.42641114960078));
#60998=CARTESIAN_POINT('Ctrl Pts',(10.4002072192657,-18.4686862833898,-0.457777203495678));
#60999=CARTESIAN_POINT('Ctrl Pts',(10.3895121106101,-18.4675238404129,-0.466757785235065));
#61000=CARTESIAN_POINT('Ctrl Pts',(10.3691517352141,-18.4654920629651,-0.476520858724267));
#61001=CARTESIAN_POINT('Ctrl Pts',(10.3605255868115,-18.4646727052056,-0.478994932552589));
#61002=CARTESIAN_POINT('Ctrl Pts',(10.350269709773,-18.4637613669848,-0.479524924856822));
#61003=CARTESIAN_POINT('Ctrl Pts',(10.3491503490814,-18.4636626963416,-0.479552113820164));
#61004=CARTESIAN_POINT('Ctrl Pts',(10.3480326234796,-18.4635649605383,-0.479548822159035));
#61005=CARTESIAN_POINT('Ctrl Pts',(10.3480326234796,-18.4635649605383,0.479548822159041));
#61006=CARTESIAN_POINT('Ctrl Pts',(10.3515043799367,-18.463868536752,0.479559046355178));
#61007=CARTESIAN_POINT('Ctrl Pts',(10.3549842920161,-18.4641804719486,0.479275189924436));
#61008=CARTESIAN_POINT('Ctrl Pts',(10.3584662558372,-18.4645002849058,0.478693581607878));
#61009=CARTESIAN_POINT('Ctrl Pts',(10.3670410360545,-18.4652878651219,0.477261296913587));
#61010=CARTESIAN_POINT('Ctrl Pts',(10.3752404682198,-18.46608779957,0.47408378771337));
#61011=CARTESIAN_POINT('Ctrl Pts',(10.3939159291592,-18.4679971841149,0.463271309310396));
#61012=CARTESIAN_POINT('Ctrl Pts',(10.4037620790052,-18.4690808995383,0.454395207725895));
#61013=CARTESIAN_POINT('Ctrl Pts',(10.4301534297193,-18.4721165427773,0.424234118800152));
#61014=CARTESIAN_POINT('Ctrl Pts',(10.4436201527526,-18.4738680701254,0.398508891735444));
#61015=CARTESIAN_POINT('Ctrl Pts',(10.4707559634892,-18.4775000338928,0.337044819567124));
#61016=CARTESIAN_POINT('Ctrl Pts',(10.4855434672333,-18.4797232784594,0.285219862910135));
#61017=CARTESIAN_POINT('Ctrl Pts',(10.503063797412,-18.4824794109906,0.184213295767431));
#61018=CARTESIAN_POINT('Ctrl Pts',(10.5077954452097,-18.4832622430944,0.14290265914675));
#61019=CARTESIAN_POINT('Ctrl Pts',(10.5129524699051,-18.4841201320625,0.0690531837747819));
#61020=CARTESIAN_POINT('Ctrl Pts',(10.5141249106268,-18.4843191140946,0.0355299301020449));
#61021=CARTESIAN_POINT('Ctrl Pts',(10.5141686022426,-18.4843264836169,0.00127631103831961));
#61022=CARTESIAN_POINT('Ctrl Pts',(10.5141690094812,-18.4843265523066,0.000638285004289643));
#61023=CARTESIAN_POINT('Ctrl Pts',(10.5141690094812,-18.4843265523066,-6.15626801878132E-15));
#61024=CARTESIAN_POINT('Origin',(10.3388776100546,-21.0856897166516,2.58225224193117E-15));
#61025=CARTESIAN_POINT('Origin',(1.05309141530195,-22.3047932944232,2.73154937136587E-15));
#61026=CARTESIAN_POINT('Origin',(1.63623295246351,-19.0374307818588,6.18563622669654));
#61027=CARTESIAN_POINT('',(1.90706327644678,-16.998194874094,5.04583540480241));
#61028=CARTESIAN_POINT('',(1.90706327644678,-16.7176961632773,5.90912166928203));
#61029=CARTESIAN_POINT('Ctrl Pts',(1.90706327644678,-16.998194874094,5.04583540480242));
#61030=CARTESIAN_POINT('Ctrl Pts',(1.90026014392336,-16.997622523982,5.04567196333409));
#61031=CARTESIAN_POINT('Ctrl Pts',(1.89355517780839,-16.9967539081074,5.04653705366796));
#61032=CARTESIAN_POINT('Ctrl Pts',(1.87732280058979,-16.9939422782637,5.05101511023688));
#61033=CARTESIAN_POINT('Ctrl Pts',(1.8684098758066,-16.9917638647488,5.055607664885));
#61034=CARTESIAN_POINT('Ctrl Pts',(1.84749974154022,-16.9854633184889,5.07034930389412));
#61035=CARTESIAN_POINT('Ctrl Pts',(1.83650132567004,-16.9808716613319,5.08235904211383));
#61036=CARTESIAN_POINT('Ctrl Pts',(1.81085694928172,-16.9680241697437,5.11736200896841));
#61037=CARTESIAN_POINT('Ctrl Pts',(1.79594323550239,-16.9576102181473,5.14737025659996));
#61038=CARTESIAN_POINT('Ctrl Pts',(1.76902539468121,-16.9307871685186,5.22698753163597));
#61039=CARTESIAN_POINT('Ctrl Pts',(1.75949337448613,-16.9155448309955,5.27332224828729));
#61040=CARTESIAN_POINT('Ctrl Pts',(1.74741836256389,-16.8870291804702,5.3604323440719));
#61041=CARTESIAN_POINT('Ctrl Pts',(1.74418490387285,-16.87267457515,5.40452184219696));
#61042=CARTESIAN_POINT('Ctrl Pts',(1.74230474178709,-16.8447903345416,5.49027879637163));
#61043=CARTESIAN_POINT('Ctrl Pts',(1.74356051202783,-16.8306696144909,5.5337656626974));
#61044=CARTESIAN_POINT('Ctrl Pts',(1.75089245923113,-16.8026196377608,5.62039732386659));
#61045=CARTESIAN_POINT('Ctrl Pts',(1.75736442403604,-16.7879279245165,5.66589231855141));
#61046=CARTESIAN_POINT('Ctrl Pts',(1.77948145071089,-16.7577464575554,5.76057523481948));
#61047=CARTESIAN_POINT('Ctrl Pts',(1.79536357091692,-16.7443881182379,5.80338352888534));
#61048=CARTESIAN_POINT('Ctrl Pts',(1.82385809602949,-16.7297952066034,5.85279728585391));
#61049=CARTESIAN_POINT('Ctrl Pts',(1.83844662204035,-16.7236372532299,5.87421791437717));
#61050=CARTESIAN_POINT('Ctrl Pts',(1.8661229457109,-16.7185311380395,5.89600163036614));
#61051=CARTESIAN_POINT('Ctrl Pts',(1.87511027899366,-16.7174688556404,5.90137286939966));
#61052=CARTESIAN_POINT('Ctrl Pts',(1.88937385988069,-16.7169970261612,5.90645548339447));
#61053=CARTESIAN_POINT('Ctrl Pts',(1.8939567335313,-16.7170046598605,5.907637155423));
#61054=CARTESIAN_POINT('Ctrl Pts',(1.90144341435482,-16.717295245985,5.90878057609673));
#61055=CARTESIAN_POINT('Ctrl Pts',(1.9042514540351,-16.7174650761299,5.90903727408275));
#61056=CARTESIAN_POINT('Ctrl Pts',(1.90706327644678,-16.7176961632773,5.90912166928201));
#61057=CARTESIAN_POINT('',(1.62584114411962,-19.7629572175357,3.94856638716317));
#61058=CARTESIAN_POINT('Origin',(1.62584114411962,-19.0362172778497,6.18524193534253));
#61059=CARTESIAN_POINT('',(1.33846910697111,-19.6367507067188,4.22280591656415));
#61060=CARTESIAN_POINT('Origin',(1.63623295246351,-19.6715220966734,4.23410382602581));
#61061=CARTESIAN_POINT('Origin',(1.33846910697111,-19.0026593919041,6.17433831723488));
#61062=CARTESIAN_POINT('Origin',(1.62584114411962,-19.0362172778497,6.18524193534253));
#61063=CARTESIAN_POINT('Origin',(5.83867335851287,-19.5281709987517,6.34508738889865));
#61064=CARTESIAN_POINT('',(10.3480326234796,-17.7080825054385,5.24947731735612));
#61065=CARTESIAN_POINT('Ctrl Pts',(10.3480326234796,-17.7080825054385,5.24947731735612));
#61066=CARTESIAN_POINT('Ctrl Pts',(7.54972025675578,-17.4728227255228,5.18170180546195));
#61067=CARTESIAN_POINT('Ctrl Pts',(4.7091881268347,-17.233938697471,5.11315489305578));
#61068=CARTESIAN_POINT('Ctrl Pts',(1.90706327644678,-16.998194874094,5.04583540480242));
#61069=CARTESIAN_POINT('',(10.0307219562183,-20.8358167812138,3.98623266785661));
#61070=CARTESIAN_POINT('Origin',(10.0307219562183,-20.0176977116355,6.50414425974677));
#61071=CARTESIAN_POINT('',(10.3480326234796,-17.4117050340792,6.16163338174817));
#61072=CARTESIAN_POINT('Origin',(10.0307219562183,-20.0176977116355,6.50414425974677));
#61073=CARTESIAN_POINT('Ctrl Pts',(1.90706327644678,-16.7176961632773,5.90912166928202));
#61074=CARTESIAN_POINT('Ctrl Pts',(4.70918812184411,-16.9479863246852,5.99322580178265));
#61075=CARTESIAN_POINT('Ctrl Pts',(7.54972025123709,-17.1815384272226,6.07818269341643));
#61076=CARTESIAN_POINT('Ctrl Pts',(10.3480326234796,-17.4117050340792,6.16163338174817));
#61077=CARTESIAN_POINT('Origin',(10.0411137645622,-20.0189112156446,6.50453855110077));
#61078=CARTESIAN_POINT('',(10.3388776100546,-20.7791530503061,4.28306801618089));
#61079=CARTESIAN_POINT('Origin',(10.3388776100546,-20.0536826055992,6.51583646056242));
#61080=CARTESIAN_POINT('Origin',(10.0411137645622,-20.7443816603515,4.27177010671924));
#61081=CARTESIAN_POINT('Ctrl Pts',(10.3480326234796,-17.4117050340792,6.16163338174817));
#61082=CARTESIAN_POINT('Ctrl Pts',(10.3515114639741,-17.4119911754408,6.16173712700432));
#61083=CARTESIAN_POINT('Ctrl Pts',(10.3549914179992,-17.4123759675224,6.16156241574048));
#61084=CARTESIAN_POINT('Ctrl Pts',(10.3584662558372,-17.4128588642783,6.1611090307738));
#61085=CARTESIAN_POINT('Ctrl Pts',(10.367223098271,-17.4140757989961,6.15996646789746));
#61086=CARTESIAN_POINT('Ctrl Pts',(10.3753630700178,-17.415831290242,6.15713972282257));
#61087=CARTESIAN_POINT('Ctrl Pts',(10.3939290316259,-17.4209477623239,6.14753302482073));
#61088=CARTESIAN_POINT('Ctrl Pts',(10.4035780672154,-17.4246680145472,6.13952487259415));
#61089=CARTESIAN_POINT('Ctrl Pts',(10.4280013399751,-17.435881088904,6.11408837463524));
#61090=CARTESIAN_POINT('Ctrl Pts',(10.4407678160189,-17.4444479537232,6.09300205845744));
#61091=CARTESIAN_POINT('Ctrl Pts',(10.4685456259696,-17.4667636690829,6.03626400623286));
#61092=CARTESIAN_POINT('Ctrl Pts',(10.4828713837316,-17.4838345078958,5.99063505235381));
#61093=CARTESIAN_POINT('Ctrl Pts',(10.5038238234649,-17.5210208246161,5.88674071610147));
#61094=CARTESIAN_POINT('Ctrl Pts',(10.5097149363751,-17.5396167538765,5.83272996465087));
#61095=CARTESIAN_POINT('Ctrl Pts',(10.5152093525458,-17.575028667588,5.72672134143434));
#61096=CARTESIAN_POINT('Ctrl Pts',(10.5146501294348,-17.5929043782428,5.67139291388392));
#61097=CARTESIAN_POINT('Ctrl Pts',(10.5071723447786,-17.6260374509827,5.56539053344041));
#61098=CARTESIAN_POINT('Ctrl Pts',(10.5000174147823,-17.6424047527201,5.5111599951682));
#61099=CARTESIAN_POINT('Ctrl Pts',(10.4763655908936,-17.6725219279295,5.40677101623364));
#61100=CARTESIAN_POINT('Ctrl Pts',(10.46054190317,-17.6845328147317,5.36240927189414));
#61101=CARTESIAN_POINT('Ctrl Pts',(10.4319469960435,-17.6978522663516,5.30950538071614));
#61102=CARTESIAN_POINT('Ctrl Pts',(10.4192298015583,-17.7023303304535,5.29065702126868));
#61103=CARTESIAN_POINT('Ctrl Pts',(10.3949786188433,-17.7070402629162,5.26742227944468));
#61104=CARTESIAN_POINT('Ctrl Pts',(10.3846960006404,-17.708325726784,5.25993527526374));
#61105=CARTESIAN_POINT('Ctrl Pts',(10.3651744504235,-17.7090036066899,5.25164757219631));
#61106=CARTESIAN_POINT('Ctrl Pts',(10.3566858346072,-17.708809998398,5.24968689932439));
#61107=CARTESIAN_POINT('Ctrl Pts',(10.3480326234796,-17.7080825054385,5.2494773173561));
#61108=CARTESIAN_POINT('Origin',(10.3388776100546,-20.0536826055992,6.51583646056242));
#61109=CARTESIAN_POINT('Origin',(1.05309141530195,-21.2131190072776,6.89256018399713));
#61110=CARTESIAN_POINT('Origin',(1.63623295246351,-16.1942058835342,11.7657792816622));
#61111=CARTESIAN_POINT('',(1.90706327644678,-14.6069951093592,10.0516057316823));
#61112=CARTESIAN_POINT('',(1.90706327644678,-14.0734548558899,10.7859608904011));
#61113=CARTESIAN_POINT('Ctrl Pts',(1.90706327644678,-14.6069951093592,10.0516057316823));
#61114=CARTESIAN_POINT('Ctrl Pts',(1.90025875958221,-14.6065011777593,10.0512733560775));
#61115=CARTESIAN_POINT('Ctrl Pts',(1.89355247265338,-14.6054074046147,10.0518279831547));
#61116=CARTESIAN_POINT('Ctrl Pts',(1.87725698375305,-14.6013332347423,10.0552320469984));
#61117=CARTESIAN_POINT('Ctrl Pts',(1.86829211419405,-14.5978127562124,10.0589614875646));
#61118=CARTESIAN_POINT('Ctrl Pts',(1.84706044347858,-14.5870683867576,10.0712702530589));
#61119=CARTESIAN_POINT('Ctrl Pts',(1.83585892185028,-14.578755053141,10.0815819441647));
#61120=CARTESIAN_POINT('Ctrl Pts',(1.80877471345631,-14.5541268705464,10.1129760302204));
#61121=CARTESIAN_POINT('Ctrl Pts',(1.79294392498685,-14.532937575839,10.1410429474249));
#61122=CARTESIAN_POINT('Ctrl Pts',(1.76567283597146,-14.4785632453815,10.2144033500597));
#61123=CARTESIAN_POINT('Ctrl Pts',(1.75650699269145,-14.4479667279783,10.2562595787974));
#61124=CARTESIAN_POINT('Ctrl Pts',(1.74778527726981,-14.4026186544839,10.3184510441844));
#61125=CARTESIAN_POINT('Ctrl Pts',(1.74564598164325,-14.3862953920429,10.3408770076601));
#61126=CARTESIAN_POINT('Ctrl Pts',(1.7434290387667,-14.3580271947068,10.3797436057767));
#61127=CARTESIAN_POINT('Ctrl Pts',(1.74295490171609,-14.3459008172406,10.3964264560483));
#61128=CARTESIAN_POINT('Ctrl Pts',(1.74292857696577,-14.3218037566088,10.4295927678078));
#61129=CARTESIAN_POINT('Ctrl Pts',(1.74337239383376,-14.3097358503636,10.4462099845887));
#61130=CARTESIAN_POINT('Ctrl Pts',(1.74549594744673,-14.281769432405,10.4847417370608));
#61131=CARTESIAN_POINT('Ctrl Pts',(1.7475518031835,-14.2657028933392,10.5068945909295));
#61132=CARTESIAN_POINT('Ctrl Pts',(1.75591196457232,-14.221353521705,10.5681486124438));
#61133=CARTESIAN_POINT('Ctrl Pts',(1.76464297432689,-14.1917029071014,10.6092002023642));
#61134=CARTESIAN_POINT('Ctrl Pts',(1.79360739934438,-14.1332147014319,10.6912265321679));
#61135=CARTESIAN_POINT('Ctrl Pts',(1.81322842075095,-14.1096237409542,10.7250788098401));
#61136=CARTESIAN_POINT('Ctrl Pts',(1.84745113279526,-14.0857929378087,10.7612654174994));
#61137=CARTESIAN_POINT('Ctrl Pts',(1.85980439378448,-14.0801722471125,10.7703887241722));
#61138=CARTESIAN_POINT('Ctrl Pts',(1.87846606194046,-14.0751582426545,10.7796242046079));
#61139=CARTESIAN_POINT('Ctrl Pts',(1.88517766043384,-14.0739697528518,10.782140967491));
#61140=CARTESIAN_POINT('Ctrl Pts',(1.89712731913029,-14.073120127819,10.7849686486705));
#61141=CARTESIAN_POINT('Ctrl Pts',(1.90207774192321,-14.0731114184795,10.7856919622308));
#61142=CARTESIAN_POINT('Ctrl Pts',(1.90706327644678,-14.0734548558899,10.7859608904011));
#61143=CARTESIAN_POINT('',(1.62584114411962,-17.5755151259486,9.86239943185911));
#61144=CARTESIAN_POINT('Origin',(1.62584114411962,-16.1931736153679,11.7650292949391));
#61145=CARTESIAN_POINT('',(1.33846910697111,-17.3707409263229,10.0842167666784));
#61146=CARTESIAN_POINT('Origin',(1.63623295246351,-17.4003192372954,10.1057066675065));
#61147=CARTESIAN_POINT('Origin',(1.33846910697111,-16.1646275725617,11.7442893808342));
#61148=CARTESIAN_POINT('Origin',(1.62584114411962,-16.1931736153679,11.7650292949391));
#61149=CARTESIAN_POINT('Origin',(5.83867335851287,-16.611654445725,12.0690734153485));
#61150=CARTESIAN_POINT('',(10.3480326234796,-15.2192095552406,10.4646480417893));
#61151=CARTESIAN_POINT('Ctrl Pts',(10.3480326234796,-15.2192095552406,10.4646480417893));
#61152=CARTESIAN_POINT('Ctrl Pts',(7.54753623341465,-15.0162497111978,10.3273833808683));
#61153=CARTESIAN_POINT('Ctrl Pts',(4.70781617470128,-14.8102983544992,10.1884122025895));
#61154=CARTESIAN_POINT('Ctrl Pts',(1.90706327644678,-14.6069951093592,10.0516057316823));
#61155=CARTESIAN_POINT('',(10.0307219562183,-18.584225684205,10.2297540313114));
#61156=CARTESIAN_POINT('Origin',(10.0307219562183,-17.0280707397496,12.3716175623118));
#61157=CARTESIAN_POINT('',(10.3480326234796,-14.655466104402,11.2405743353076));
#61158=CARTESIAN_POINT('Origin',(10.0307219562183,-17.0280707397496,12.3716175623118));
#61159=CARTESIAN_POINT('Ctrl Pts',(1.90706327644678,-14.0734548558899,10.7859608904011));
#61160=CARTESIAN_POINT('Ctrl Pts',(4.70781616958245,-14.2663896989247,10.9370382417485));
#61161=CARTESIAN_POINT('Ctrl Pts',(7.54753622799762,-14.4622016128173,11.0899651657448));
#61162=CARTESIAN_POINT('Ctrl Pts',(10.3480326234796,-14.655466104402,11.2405743353076));
#61163=CARTESIAN_POINT('Origin',(10.0411137645622,-17.0291030079158,12.3723675490348));
#61164=CARTESIAN_POINT('',(10.3388776100546,-18.4386081065242,10.4945511677868));
#61165=CARTESIAN_POINT('Origin',(10.3388776100546,-17.0586813188882,12.3938574498629));
#61166=CARTESIAN_POINT('Origin',(10.0411137645622,-18.4090297955518,10.4730612669588));
#61167=CARTESIAN_POINT('Ctrl Pts',(10.3480326234796,-14.655466104402,11.2405743353076));
#61168=CARTESIAN_POINT('Ctrl Pts',(10.3515211595623,-14.6557068510616,11.2407619468765));
#61169=CARTESIAN_POINT('Ctrl Pts',(10.3550011198928,-14.656127803182,11.2407133851835));
#61170=CARTESIAN_POINT('Ctrl Pts',(10.3584662558372,-14.6567254954937,11.2404322010368));
#61171=CARTESIAN_POINT('Ctrl Pts',(10.3671694892744,-14.658226693656,11.2397259628669));
#61172=CARTESIAN_POINT('Ctrl Pts',(10.3753654465597,-14.6607699081134,11.2375879642563));
#61173=CARTESIAN_POINT('Ctrl Pts',(10.3941492137284,-14.6687216746163,11.2299109713814));
#61174=CARTESIAN_POINT('Ctrl Pts',(10.404002965845,-14.6748808959337,11.2232825987702));
#61175=CARTESIAN_POINT('Ctrl Pts',(10.4308436412033,-14.6954625055177,11.2002100598279));
#61176=CARTESIAN_POINT('Ctrl Pts',(10.4443760953687,-14.7123773258605,11.1799381757235));
#61177=CARTESIAN_POINT('Ctrl Pts',(10.4751024728252,-14.7571304838424,11.1253565526293));
#61178=CARTESIAN_POINT('Ctrl Pts',(10.4913920727396,-14.7969697951172,11.0748241683197));
#61179=CARTESIAN_POINT('Ctrl Pts',(10.5062952995223,-14.8615728881704,10.9899781948953));
#61180=CARTESIAN_POINT('Ctrl Pts',(10.5095242362634,-14.881895269972,10.9629200882246));
#61181=CARTESIAN_POINT('Ctrl Pts',(10.512859180135,-14.914906904102,10.9184305611832));
#61182=CARTESIAN_POINT('Ctrl Pts',(10.5136719991087,-14.9279744210184,10.9006780007669));
#61183=CARTESIAN_POINT('Ctrl Pts',(10.514295657022,-14.9525087414765,10.8670882523061));
#61184=CARTESIAN_POINT('Ctrl Pts',(10.5142026737932,-14.9640796299258,10.8511355186811));
#61185=CARTESIAN_POINT('Ctrl Pts',(10.5131483322071,-14.9893112870103,10.816105099928));
#61186=CARTESIAN_POINT('Ctrl Pts',(10.512009812725,-15.0030451759508,10.7968758883503));
#61187=CARTESIAN_POINT('Ctrl Pts',(10.5074172692912,-15.0390378011656,10.7460384791957));
#61188=CARTESIAN_POINT('Ctrl Pts',(10.5028514263372,-15.0615825002596,10.7137256630153));
#61189=CARTESIAN_POINT('Ctrl Pts',(10.4823258875197,-15.1286103745232,10.6159756467568));
#61190=CARTESIAN_POINT('Ctrl Pts',(10.4610892332281,-15.1642626717183,10.5615248358069));
#61191=CARTESIAN_POINT('Ctrl Pts',(10.4253700252925,-15.1959357631408,10.5103262009135));
#61192=CARTESIAN_POINT('Ctrl Pts',(10.4122912190471,-15.2055154329318,10.4944454192631));
#61193=CARTESIAN_POINT('Ctrl Pts',(10.3868737804665,-15.2153586960743,10.4762419431138));
#61194=CARTESIAN_POINT('Ctrl Pts',(10.3771760707493,-15.2179090290457,10.4710384088582));
#61195=CARTESIAN_POINT('Ctrl Pts',(10.3604838650278,-15.2195700377639,10.4660465521435));
#61196=CARTESIAN_POINT('Ctrl Pts',(10.35429238307,-15.2196632176109,10.4649548601736));
#61197=CARTESIAN_POINT('Ctrl Pts',(10.3480326234796,-15.2192095552406,10.4646480417893));
#61198=CARTESIAN_POINT('Origin',(10.3388776100546,-17.0586813188882,12.3938574498629));
#61199=CARTESIAN_POINT('Origin',(1.05309141530195,-18.0449568312087,13.110428553894));
#61200=CARTESIAN_POINT('Origin',(1.63623295246351,-11.7657792816622,16.1942058835342));
#61201=CARTESIAN_POINT('',(1.90706327644678,-10.7859608904011,14.0734548558899));
#61202=CARTESIAN_POINT('',(1.90706327644678,-10.0516057316823,14.6069951093592));
#61203=CARTESIAN_POINT('Ctrl Pts',(1.90706327644678,-10.7859608904011,14.0734548558899));
#61204=CARTESIAN_POINT('Ctrl Pts',(1.90025875962456,-10.785593843247,14.0729861146496));
#61205=CARTESIAN_POINT('Ctrl Pts',(1.89355247272025,-10.7843822139959,14.0731756018448));
#61206=CARTESIAN_POINT('Ctrl Pts',(1.87725698375415,-10.779455534593,14.0751540712245));
#61207=CARTESIAN_POINT('Ctrl Pts',(1.86829211419528,-10.7749549000324,14.0776130922829));
#61208=CARTESIAN_POINT('Ctrl Pts',(1.84706044347986,-10.7609327797318,14.0859992311582));
#61209=CARTESIAN_POINT('Ctrl Pts',(1.83585892185164,-10.7498398418315,14.0932372708107));
#61210=CARTESIAN_POINT('Ctrl Pts',(1.8087747134592,-10.716715742179,14.115484293963));
#61211=CARTESIAN_POINT('Ctrl Pts',(1.79294392498963,-10.6878903709779,14.1356296662977));
#61212=CARTESIAN_POINT('Ctrl Pts',(1.76567283597264,-10.6135076985476,14.1885969630932));
#61213=CARTESIAN_POINT('Ctrl Pts',(1.75650699269213,-10.5714743952939,14.2189497583362));
#61214=CARTESIAN_POINT('Ctrl Pts',(1.74778527727007,-10.5091275947847,14.2640840313795));
#61215=CARTESIAN_POINT('Ctrl Pts',(1.74564598164342,-10.4866732458432,14.2803682245796));
#61216=CARTESIAN_POINT('Ctrl Pts',(1.74342903876677,-10.447778153231,14.3085972026077));
#61217=CARTESIAN_POINT('Ctrl Pts',(1.74295490171613,-10.4310899986741,14.3207162793516));
#61218=CARTESIAN_POINT('Ctrl Pts',(1.74292857696575,-10.3979233781624,14.3448129150221));
#61219=CARTESIAN_POINT('Ctrl Pts',(1.74337239383369,-10.3813111149053,14.356887639208));
#61220=CARTESIAN_POINT('Ctrl Pts',(1.74549594744657,-10.3428065045316,14.3848914150597));
#61221=CARTESIAN_POINT('Ctrl Pts',(1.74755180318325,-10.3206807095399,14.4009951974737));
#61222=CARTESIAN_POINT('Ctrl Pts',(1.75591196457167,-10.2595734170331,14.4455465242584));
#61223=CARTESIAN_POINT('Ctrl Pts',(1.76464297432576,-10.2186883678718,14.4754263625496));
#61224=CARTESIAN_POINT('Ctrl Pts',(1.79360739934107,-10.1377152488505,14.5353641884927));
#61225=CARTESIAN_POINT('Ctrl Pts',(1.81322842074624,-10.1048179830629,14.5602696100633));
#61226=CARTESIAN_POINT('Ctrl Pts',(1.84745113278966,-10.0709712657048,14.5873209959204));
#61227=CARTESIAN_POINT('Ctrl Pts',(1.85980439377954,-10.0628064143836,14.5942608872378));
#61228=CARTESIAN_POINT('Ctrl Pts',(1.87846606193735,-10.0551838923635,14.6014949385012));
#61229=CARTESIAN_POINT('Ctrl Pts',(1.88517766043127,-10.0532758488901,14.6035212586947));
#61230=CARTESIAN_POINT('Ctrl Pts',(1.89712731921794,-10.0515940059141,14.6059479947511));
#61231=CARTESIAN_POINT('Ctrl Pts',(1.90207774198235,-10.051362206673,14.6066332154785));
#61232=CARTESIAN_POINT('Ctrl Pts',(1.90706327644678,-10.0516057316823,14.6069951093592));
#61233=CARTESIAN_POINT('',(1.62584114411962,-13.6676591580191,14.8108321047873));
#61234=CARTESIAN_POINT('Origin',(1.62584114411962,-11.7650292949391,16.1931736153679));
#61235=CARTESIAN_POINT('',(1.33846910697111,-13.4043619949899,14.9585142188006));
#61236=CARTESIAN_POINT('Origin',(1.63623295246351,-13.425851895818,14.988092529773));
#61237=CARTESIAN_POINT('Origin',(1.33846910697111,-11.7442893808342,16.1646275725618));
#61238=CARTESIAN_POINT('Origin',(1.62584114411962,-11.7650292949391,16.1931736153679));
#61239=CARTESIAN_POINT('Origin',(5.83867335851287,-12.0690734153485,16.611654445725));
#61240=CARTESIAN_POINT('',(10.3480326234796,-11.2405743353076,14.655466104402));
#61241=CARTESIAN_POINT('Ctrl Pts',(10.3480326234796,-11.2405743353076,14.655466104402));
#61242=CARTESIAN_POINT('Ctrl Pts',(7.54753623341465,-11.0899651660361,14.4622016131911));
#61243=CARTESIAN_POINT('Ctrl Pts',(4.70781617470128,-10.9370382420246,14.2663896992774));
#61244=CARTESIAN_POINT('Ctrl Pts',(1.90706327644678,-10.7859608904011,14.0734548558899));
#61245=CARTESIAN_POINT('',(10.0307219562183,-14.5134810933121,15.4719157952941));
#61246=CARTESIAN_POINT('Origin',(10.0307219562183,-12.3716175623118,17.0280707397496));
#61247=CARTESIAN_POINT('',(10.3480326234796,-10.4646480417893,15.2192095552406));
#61248=CARTESIAN_POINT('Origin',(10.0307219562183,-12.3716175623118,17.0280707397496));
#61249=CARTESIAN_POINT('Ctrl Pts',(1.90706327644678,-10.0516057316823,14.6069951093592));
#61250=CARTESIAN_POINT('Ctrl Pts',(4.70781616958245,-10.1884122023394,14.8102983541277));
#61251=CARTESIAN_POINT('Ctrl Pts',(7.54753622799762,-10.3273833806028,15.0162497108052));
#61252=CARTESIAN_POINT('Ctrl Pts',(10.3480326234796,-10.4646480417893,15.2192095552406));
#61253=CARTESIAN_POINT('Origin',(10.0411137645622,-12.3723675490348,17.0291030079158));
#61254=CARTESIAN_POINT('',(10.3388776100546,-14.293163731939,15.6787545312522));
#61255=CARTESIAN_POINT('Origin',(10.3388776100546,-12.3938574498629,17.0586813188882));
#61256=CARTESIAN_POINT('Origin',(10.0411137645622,-14.2716738311109,15.6491762202798));
#61257=CARTESIAN_POINT('Ctrl Pts',(10.3480326234796,-10.4646480417893,15.2192095552406));
#61258=CARTESIAN_POINT('Ctrl Pts',(10.3515211595624,-10.4648190303056,15.2194623792549));
#61259=CARTESIAN_POINT('Ctrl Pts',(10.3550011198929,-10.4652343859512,15.2195462756993));
#61260=CARTESIAN_POINT('Ctrl Pts',(10.3584662558372,-10.4658897157988,15.219463550766));
#61261=CARTESIAN_POINT('Ctrl Pts',(10.3671694892744,-10.46753567969,15.2192557740965));
#61262=CARTESIAN_POINT('Ctrl Pts',(10.3753654465596,-10.4706150982766,15.2180083130739));
#61263=CARTESIAN_POINT('Ctrl Pts',(10.3941492137284,-10.4805499988893,15.2131642899593));
#61264=CARTESIAN_POINT('Ctrl Pts',(10.4040029658451,-10.4884560462405,15.2087636370541));
#61265=CARTESIAN_POINT('Ctrl Pts',(10.4308436412037,-10.5151601267881,15.1931804156785));
#61266=CARTESIAN_POINT('Ctrl Pts',(10.4443760953692,-10.5375114335939,15.1791276751457));
#61267=CARTESIAN_POINT('Ctrl Pts',(10.4751024728252,-10.596940865233,15.1410469532009));
#61268=CARTESIAN_POINT('Ctrl Pts',(10.4913920727396,-10.6504456673436,15.1052988240475));
#61269=CARTESIAN_POINT('Ctrl Pts',(10.5062952995223,-10.7381057076571,15.0445689617835));
#61270=CARTESIAN_POINT('Ctrl Pts',(10.5095242362634,-10.7657948560931,15.0251151344585));
#61271=CARTESIAN_POINT('Ctrl Pts',(10.512859180135,-10.8109388057733,14.9930042358172));
#61272=CARTESIAN_POINT('Ctrl Pts',(10.5136719991087,-10.8288525957507,14.9801586323539));
#61273=CARTESIAN_POINT('Ctrl Pts',(10.514295657022,-10.8625659242064,14.9557944051666));
#61274=CARTESIAN_POINT('Ctrl Pts',(10.5142026737932,-10.8785001588622,14.9441980550706));
#61275=CARTESIAN_POINT('Ctrl Pts',(10.5131483322071,-10.9133218854643,14.9186791578822));
#61276=CARTESIAN_POINT('Ctrl Pts',(10.512009812725,-10.9323257432012,14.9046350959895));
#61277=CARTESIAN_POINT('Ctrl Pts',(10.5074172692912,-10.9822663873291,14.8674081796049));
#61278=CARTESIAN_POINT('Ctrl Pts',(10.5028514263372,-11.0136928796462,14.8436435603699));
#61279=CARTESIAN_POINT('Ctrl Pts',(10.4823258875198,-11.1076465924618,14.7713905226839));
#61280=CARTESIAN_POINT('Ctrl Pts',(10.4610892332283,-11.1583801679713,14.7306218898341));
#61281=CARTESIAN_POINT('Ctrl Pts',(10.4253700252924,-11.2043243162311,14.6917166180069));
#61282=CARTESIAN_POINT('Ctrl Pts',(10.4122912190471,-11.2183425550237,14.6795733779005));
#61283=CARTESIAN_POINT('Ctrl Pts',(10.3868737804665,-11.2333292380637,14.6653025788806));
#61284=CARTESIAN_POINT('Ctrl Pts',(10.3771760707494,-11.2373627293707,14.6611418199486));
#61285=CARTESIAN_POINT('Ctrl Pts',(10.3604838650279,-11.2404850110942,14.6569075620133));
#61286=CARTESIAN_POINT('Ctrl Pts',(10.35429238307,-11.2409109817661,14.6558980954078));
#61287=CARTESIAN_POINT('Ctrl Pts',(10.3480326234796,-11.2405743353076,14.655466104402));
#61288=CARTESIAN_POINT('Origin',(10.3388776100546,-12.3938574498629,17.0586813188882));
#61289=CARTESIAN_POINT('Origin',(1.05309141530195,-13.110428553894,18.0449568312087));
#61290=CARTESIAN_POINT('Origin',(1.63623295246351,-6.18563622669653,19.0374307818588));
#61291=CARTESIAN_POINT('',(1.90706327644678,-5.90912166928202,16.7176961632773));
#61292=CARTESIAN_POINT('',(1.90706327644678,-5.04583540480242,16.998194874094));
#61293=CARTESIAN_POINT('Ctrl Pts',(1.90706327644678,-5.90912166928201,16.7176961632773));
#61294=CARTESIAN_POINT('Ctrl Pts',(1.90026014393042,-5.9089174772527,16.7171370538258));
#61295=CARTESIAN_POINT('Ctrl Pts',(1.89355517781953,-5.90770704487335,16.716942816161));
#61296=CARTESIAN_POINT('Ctrl Pts',(1.87732280058988,-5.9024315864467,16.7173002954459));
#61297=CARTESIAN_POINT('Ctrl Pts',(1.86840987580669,-5.89743569235133,16.7182373577841));
#61298=CARTESIAN_POINT('Ctrl Pts',(1.84749974154035,-5.88180608769516,16.7218050267902));
#61299=CARTESIAN_POINT('Ctrl Pts',(1.8365013256702,-5.86939109701701,16.7251494451272));
#61300=CARTESIAN_POINT('Ctrl Pts',(1.81085694928166,-5.83352153589342,16.735329833801));
#61301=CARTESIAN_POINT('Ctrl Pts',(1.79594323550241,-5.80312318642153,16.7445431753858));
#61302=CARTESIAN_POINT('Ctrl Pts',(1.76902539468134,-5.72294526487896,16.7696407324889));
#61303=CARTESIAN_POINT('Ctrl Pts',(1.75949337448623,-5.67650047047193,16.7845442855155));
#61304=CARTESIAN_POINT('Ctrl Pts',(1.74741836256394,-5.5892658437623,16.8126766692629));
#61305=CARTESIAN_POINT('Ctrl Pts',(1.74418490387289,-5.5451592651959,16.8269787063902));
#61306=CARTESIAN_POINT('Ctrl Pts',(1.74230474178708,-5.45939048648195,16.8548265548082));
#61307=CARTESIAN_POINT('Ctrl Pts',(1.74356051202779,-5.41590892159468,16.868963591009));
#61308=CARTESIAN_POINT('Ctrl Pts',(1.75089245923106,-5.32933507280867,16.8971914959594));
#61309=CARTESIAN_POINT('Ctrl Pts',(1.75736442403595,-5.28389327657374,16.9120469371971));
#61310=CARTESIAN_POINT('Ctrl Pts',(1.77948145071086,-5.189552967063,16.9432828393371));
#61311=CARTESIAN_POINT('Ctrl Pts',(1.79536357091694,-5.1470684948178,16.9576377997402));
#61312=CARTESIAN_POINT('Ctrl Pts',(1.82385809602975,-5.09851442742689,16.9748765638372));
#61313=CARTESIAN_POINT('Ctrl Pts',(1.83844662204133,-5.07756522074329,16.9824854044486));
#61314=CARTESIAN_POINT('Ctrl Pts',(1.86612294571246,-5.05694052510263,16.9911586174827));
#61315=CARTESIAN_POINT('Ctrl Pts',(1.87511027899488,-5.05197070751612,16.9934563480593));
#61316=CARTESIAN_POINT('Ctrl Pts',(1.88937385988138,-5.04758145200929,16.9960621155412));
#61317=CARTESIAN_POINT('Ctrl Pts',(1.89395673353182,-5.04662994623244,16.9967628607251));
#61318=CARTESIAN_POINT('Ctrl Pts',(1.9014434143977,-5.04587570170989,16.9976700356524));
#61319=CARTESIAN_POINT('Ctrl Pts',(1.90425145406696,-5.04576785233642,16.9979583144138));
#61320=CARTESIAN_POINT('Ctrl Pts',(1.90706327644678,-5.04583540480242,16.998194874094));
#61321=CARTESIAN_POINT('',(1.62584114411962,-8.42191748352189,18.3094773381637));
#61322=CARTESIAN_POINT('Origin',(1.62584114411962,-6.18524193534253,19.0362172778497));
#61323=CARTESIAN_POINT('',(1.33846910697111,-8.12587071790561,18.3685680770895));
#61324=CARTESIAN_POINT('Origin',(1.63623295246351,-8.13716862736726,18.4033394670442));
#61325=CARTESIAN_POINT('Origin',(1.33846910697111,-6.17433831723488,19.0026593919042));
#61326=CARTESIAN_POINT('Origin',(1.62584114411962,-6.18524193534253,19.0362172778497));
#61327=CARTESIAN_POINT('Origin',(5.83867335851287,-6.34508738889865,19.5281709987517));
#61328=CARTESIAN_POINT('',(10.3480326234796,-6.16163338174817,17.4117050340792));
#61329=CARTESIAN_POINT('Ctrl Pts',(10.3480326234796,-6.16163338174816,17.4117050340792));
#61330=CARTESIAN_POINT('Ctrl Pts',(7.54972025675578,-6.078182693581,17.1815384276765));
#61331=CARTESIAN_POINT('Ctrl Pts',(4.7091881268347,-5.99322580193244,16.9479863250953));
#61332=CARTESIAN_POINT('Ctrl Pts',(1.90706327644678,-5.90912166928201,16.7176961632773));
#61333=CARTESIAN_POINT('',(10.0307219562183,-9.02205585163692,19.1995786420573));
#61334=CARTESIAN_POINT('Origin',(10.0307219562183,-6.50414425974676,20.0176977116355));
#61335=CARTESIAN_POINT('',(10.3480326234796,-5.24947731735611,17.7080825054385));
#61336=CARTESIAN_POINT('Origin',(10.0307219562183,-6.50414425974676,20.0176977116355));
#61337=CARTESIAN_POINT('Ctrl Pts',(1.90706327644677,-5.04583540480243,16.998194874094));
#61338=CARTESIAN_POINT('Ctrl Pts',(4.70918812184411,-5.11315489293588,17.2339386970511));
#61339=CARTESIAN_POINT('Ctrl Pts',(7.54972025123708,-5.18170180532829,17.4728227250588));
#61340=CARTESIAN_POINT('Ctrl Pts',(10.3480326234796,-5.24947731735612,17.7080825054385));
#61341=CARTESIAN_POINT('Origin',(10.0411137645622,-6.50453855110077,20.0189112156446));
#61342=CARTESIAN_POINT('',(10.3388776100546,-8.74860490494395,19.3282121608924));
#61343=CARTESIAN_POINT('Origin',(10.3388776100546,-6.51583646056242,20.0536826055992));
#61344=CARTESIAN_POINT('Origin',(10.0411137645622,-8.73730699548229,19.2934407709377));
#61345=CARTESIAN_POINT('Ctrl Pts',(10.3480326234796,-5.24947731735611,17.7080825054385));
#61346=CARTESIAN_POINT('Ctrl Pts',(10.3515114639741,-5.24956157535323,17.7083749785944));
#61347=CARTESIAN_POINT('Ctrl Pts',(10.3549914179992,-5.24992909484554,17.7085835892234));
#61348=CARTESIAN_POINT('Ctrl Pts',(10.3584662558372,-5.25057973058011,17.7087077679084));
#61349=CARTESIAN_POINT('Ctrl Pts',(10.367223098271,-5.25221937964431,17.7090207071676));
#61350=CARTESIAN_POINT('Ctrl Pts',(10.3753630700179,-5.25553811631364,17.708779410352));
#61351=CARTESIAN_POINT('Ctrl Pts',(10.3939290316258,-5.26631748509036,17.7072720478088));
#61352=CARTESIAN_POINT('Ctrl Pts',(10.4035780672154,-5.27498292572683,17.705574721304));
#61353=CARTESIAN_POINT('Ctrl Pts',(10.4280013399751,-5.30215236459277,17.6996950906475));
#61354=CARTESIAN_POINT('Ctrl Pts',(10.4407678160189,-5.3242470295285,17.6942316042003));
#61355=CARTESIAN_POINT('Ctrl Pts',(10.46854562597,-5.38326592638951,17.6789356068263));
#61356=CARTESIAN_POINT('Ctrl Pts',(10.4828713837318,-5.43021451281203,17.6659261793664));
#61357=CARTESIAN_POINT('Ctrl Pts',(10.5038238234649,-5.53612436501356,17.6349429829058));
#61358=CARTESIAN_POINT('Ctrl Pts',(10.5097149363751,-5.59075039378798,17.6182406825359));
#61359=CARTESIAN_POINT('Ctrl Pts',(10.5152093525458,-5.69732777215565,17.5845792171893));
#61360=CARTESIAN_POINT('Ctrl Pts',(10.5146501294348,-5.75259648941307,17.5665197371488));
#61361=CARTESIAN_POINT('Ctrl Pts',(10.5071723447786,-5.85782934815563,17.5310183201387));
#61362=CARTESIAN_POINT('Ctrl Pts',(10.5000174147823,-5.91132323381308,17.5123838347761));
#61363=CARTESIAN_POINT('Ctrl Pts',(10.4763655908934,-6.01347812322609,17.4753908390231));
#61364=CARTESIAN_POINT('Ctrl Pts',(10.4605419031697,-6.05642735042589,17.459032671475));
#61365=CARTESIAN_POINT('Ctrl Pts',(10.4319469960435,-6.10705647468779,17.4387122071682));
#61366=CARTESIAN_POINT('Ctrl Pts',(10.4192298015583,-6.12493725783481,17.4312562494153));
#61367=CARTESIAN_POINT('Ctrl Pts',(10.3949786188433,-6.14650298767119,17.421409626235));
#61368=CARTESIAN_POINT('Ctrl Pts',(10.3846960006404,-6.15331567799441,17.4180488377084));
#61369=CARTESIAN_POINT('Ctrl Pts',(10.3651744504234,-6.16041901843181,17.4137258644339));
#61370=CARTESIAN_POINT('Ctrl Pts',(10.3566858346072,-6.16189143600687,17.4124167774369));
#61371=CARTESIAN_POINT('Ctrl Pts',(10.3480326234796,-6.16163338174815,17.4117050340792));
#61372=CARTESIAN_POINT('Origin',(10.3388776100546,-6.51583646056242,20.0536826055992));
#61373=CARTESIAN_POINT('Origin',(1.05309141530195,-6.89256018399713,21.2131190072776));
#61374=CARTESIAN_POINT('Origin',(1.63623295246351,1.22569627942895E-15,
20.0171393136753));
#61375=CARTESIAN_POINT('',(1.90706327644678,-0.453856447902044,17.7254928911647));
#61376=CARTESIAN_POINT('',(1.90706327644678,0.453856447902047,17.7254928911647));
#61377=CARTESIAN_POINT('Ctrl Pts',(1.90706327644678,-0.453856447902034,
17.7254928911647));
#61378=CARTESIAN_POINT('Ctrl Pts',(1.90025953256256,-0.453835022138933,
17.7248979942144));
#61379=CARTESIAN_POINT('Ctrl Pts',(1.89355398313235,-0.452743661153185,
17.7243391729909));
#61380=CARTESIAN_POINT('Ctrl Pts',(1.87729436838704,-0.44760688140271,17.7230467959921));
#61381=CARTESIAN_POINT('Ctrl Pts',(1.86835902889014,-0.442546314021897,
17.722392711458));
#61382=CARTESIAN_POINT('Ctrl Pts',(1.84731494010094,-0.426450928593983,
17.7209473414007));
#61383=CARTESIAN_POINT('Ctrl Pts',(1.83623221810553,-0.41344928658027,17.7202879485127));
#61384=CARTESIAN_POINT('Ctrl Pts',(1.81006546585961,-0.375219786705435,
17.7188609517426));
#61385=CARTESIAN_POINT('Ctrl Pts',(1.79484445174972,-0.342313735271107,
17.7182253713052));
#61386=CARTESIAN_POINT('Ctrl Pts',(1.76839326635828,-0.257598032772368,
17.717351777811));
#61387=CARTESIAN_POINT('Ctrl Pts',(1.7592161614996,-0.21010790065141,17.7171803340554));
#61388=CARTESIAN_POINT('Ctrl Pts',(1.74822227890756,-0.126194388056563,
17.7169975657511));
#61389=CARTESIAN_POINT('Ctrl Pts',(1.74516474660436,-0.0869626247328285,
17.716966780863));
#61390=CARTESIAN_POINT('Ctrl Pts',(1.74251542765412,-0.0122397150417835,
17.7169388371718));
#61391=CARTESIAN_POINT('Ctrl Pts',(1.74267268152327,0.0243528511787307,
17.7169400569674));
#61392=CARTESIAN_POINT('Ctrl Pts',(1.74602547045575,0.0996677434135183,
17.71697649914));
#61393=CARTESIAN_POINT('Ctrl Pts',(1.74954197522153,0.139554220968224,17.7170140039981));
#61394=CARTESIAN_POINT('Ctrl Pts',(1.76185308853241,0.224756276798993,17.7172332241402));
#61395=CARTESIAN_POINT('Ctrl Pts',(1.77207894319219,0.273353606336582,17.7174389665532));
#61396=CARTESIAN_POINT('Ctrl Pts',(1.79824775576491,0.348923678359703,17.7183749061735));
#61397=CARTESIAN_POINT('Ctrl Pts',(1.81321786098122,0.382374164866884,17.7189861130437));
#61398=CARTESIAN_POINT('Ctrl Pts',(1.84564815302405,0.424859842184585,17.7208443091634));
#61399=CARTESIAN_POINT('Ctrl Pts',(1.85822154357118,0.436125221546705,17.7216651227597));
#61400=CARTESIAN_POINT('Ctrl Pts',(1.87729261989199,0.447206202216652,17.7230568968888));
#61401=CARTESIAN_POINT('Ctrl Pts',(1.88421421928185,0.450152284723852,17.7235877581235));
#61402=CARTESIAN_POINT('Ctrl Pts',(1.89663970754184,0.453190575676487,17.7245977295869));
#61403=CARTESIAN_POINT('Ctrl Pts',(1.90183077502295,0.453839970160099,17.7250353784787));
#61404=CARTESIAN_POINT('Ctrl Pts',(1.90706327644678,0.453856447902037,17.7254928911647));
#61405=CARTESIAN_POINT('',(1.62584114411962,-2.35177984678802,20.0158633600508));
#61406=CARTESIAN_POINT('Origin',(1.62584114411962,1.36962313288626E-15,
20.0158633600508));
#61407=CARTESIAN_POINT('',(1.33846910697111,-2.05196259868229,19.9805785106537));
#61408=CARTESIAN_POINT('Origin',(1.63623295246351,-2.05196259868229,20.0171393136753));
#61409=CARTESIAN_POINT('Origin',(1.33846910697111,1.22345757590922E-15,
19.9805785106537));
#61410=CARTESIAN_POINT('Origin',(1.62584114411962,1.36962313288626E-15,
20.0158633600508));
#61411=CARTESIAN_POINT('Origin',(5.83867335851287,1.2572918484374E-15,20.5331341136527));
#61412=CARTESIAN_POINT('',(10.3480326234796,-0.479548822159047,18.4635649605383));
#61413=CARTESIAN_POINT('Ctrl Pts',(10.3480326234796,-0.479548822159038,
18.4635649605383));
#61414=CARTESIAN_POINT('Ctrl Pts',(7.55083071619378,-0.471311164566919,
18.2189729292873));
#61415=CARTESIAN_POINT('Ctrl Pts',(4.7097183119132,-0.462682327280518,17.9705478141232));
#61416=CARTESIAN_POINT('Ctrl Pts',(1.90706327644678,-0.453856447902024,
17.7254928911647));
#61417=CARTESIAN_POINT('',(10.0307219562183,-2.64748892284414,21.0478529600056));
#61418=CARTESIAN_POINT('Origin',(10.0307219562183,1.45092122957671E-15,
21.0478529600056));
#61419=CARTESIAN_POINT('',(10.3480326234796,0.47954882215905,18.4635649605383));
#61420=CARTESIAN_POINT('Origin',(10.0307219562183,1.45092122957671E-15,
21.0478529600056));
#61421=CARTESIAN_POINT('Ctrl Pts',(1.90706327644678,0.453856447902028,17.7254928911647));
#61422=CARTESIAN_POINT('Ctrl Pts',(4.70971830698341,0.462682327264997,17.9705478136921));
#61423=CARTESIAN_POINT('Ctrl Pts',(7.55083071063942,0.471311164550565,18.2189729288016));
#61424=CARTESIAN_POINT('Ctrl Pts',(10.3480326234796,0.479548822159042,18.4635649605383));
#61425=CARTESIAN_POINT('Origin',(10.0411137645622,1.28888741744585E-15,
21.0491289136301));
#61426=CARTESIAN_POINT('',(10.3388776100546,-2.34767167473842,21.0856897166516));
#61427=CARTESIAN_POINT('Origin',(10.3388776100546,1.29112612096558E-15,
21.0856897166516));
#61428=CARTESIAN_POINT('Origin',(10.0411137645622,-2.34767167473842,21.0491289136301));
#61429=CARTESIAN_POINT('Ctrl Pts',(10.3480326234796,0.47954882215904,18.4635649605383));
#61430=CARTESIAN_POINT('Ctrl Pts',(10.3515043799367,0.479559046355177,18.463868536752));
#61431=CARTESIAN_POINT('Ctrl Pts',(10.3549842920161,0.479275189924435,18.4641804719486));
#61432=CARTESIAN_POINT('Ctrl Pts',(10.3584662558372,0.478693581607878,18.4645002849058));
#61433=CARTESIAN_POINT('Ctrl Pts',(10.3670410360545,0.477261296913587,18.4652878651219));
#61434=CARTESIAN_POINT('Ctrl Pts',(10.3752404682198,0.474083787713375,18.46608779957));
#61435=CARTESIAN_POINT('Ctrl Pts',(10.3939159291592,0.463271309310395,18.4679971841149));
#61436=CARTESIAN_POINT('Ctrl Pts',(10.4037620790052,0.454395207725889,18.4690808995383));
#61437=CARTESIAN_POINT('Ctrl Pts',(10.4301534297193,0.424234118800146,18.4721165427773));
#61438=CARTESIAN_POINT('Ctrl Pts',(10.4436201527526,0.398508891735436,18.4738680701254));
#61439=CARTESIAN_POINT('Ctrl Pts',(10.4707559634892,0.337044819567114,18.4775000338928));
#61440=CARTESIAN_POINT('Ctrl Pts',(10.4855434672333,0.28521986291012,18.4797232784594));
#61441=CARTESIAN_POINT('Ctrl Pts',(10.503063797412,0.184213295767423,18.4824794109906));
#61442=CARTESIAN_POINT('Ctrl Pts',(10.5077954452097,0.14290265914674,18.4832622430944));
#61443=CARTESIAN_POINT('Ctrl Pts',(10.5129524699051,0.0690531837747757,
18.4841201320625));
#61444=CARTESIAN_POINT('Ctrl Pts',(10.5141249106268,0.0355299301020397,
18.4843191140946));
#61445=CARTESIAN_POINT('Ctrl Pts',(10.5142094879025,-0.0307774777111863,
18.4843333798549));
#61446=CARTESIAN_POINT('Ctrl Pts',(10.5131850989077,-0.0641628250529937,
18.4841592802621));
#61447=CARTESIAN_POINT('Ctrl Pts',(10.5083046161227,-0.137261078256542,
18.4833464708957));
#61448=CARTESIAN_POINT('Ctrl Pts',(10.503879825914,-0.178099201717482,18.4826118937437));
#61449=CARTESIAN_POINT('Ctrl Pts',(10.4867651973882,-0.280116334659332,
18.479909817102));
#61450=CARTESIAN_POINT('Ctrl Pts',(10.4718859508697,-0.334420796175981,
18.4776521193349));
#61451=CARTESIAN_POINT('Ctrl Pts',(10.4435576763644,-0.398681362505448,
18.4738593034484));
#61452=CARTESIAN_POINT('Ctrl Pts',(10.429285329043,-0.426411149600798,18.4719918118745));
#61453=CARTESIAN_POINT('Ctrl Pts',(10.4002072192657,-0.4577772034957,18.4686862833898));
#61454=CARTESIAN_POINT('Ctrl Pts',(10.3895121106101,-0.466757785235074,
18.4675238404129));
#61455=CARTESIAN_POINT('Ctrl Pts',(10.3691517352141,-0.47652085872427,18.4654920629651));
#61456=CARTESIAN_POINT('Ctrl Pts',(10.3605255868115,-0.478994932552596,
18.4646727052056));
#61457=CARTESIAN_POINT('Ctrl Pts',(10.350269709773,-0.479524924856829,18.4637613669848));
#61458=CARTESIAN_POINT('Ctrl Pts',(10.3491503490814,-0.479552113820166,
18.4636626963416));
#61459=CARTESIAN_POINT('Ctrl Pts',(10.3480326234796,-0.479548822159036,
18.4635649605383));
#61460=CARTESIAN_POINT('Origin',(10.3388776100546,1.29112612096558E-15,
21.0856897166516));
#61461=CARTESIAN_POINT('Origin',(1.05309141530195,1.36577468568293E-15,
22.3047932944232));
#61462=CARTESIAN_POINT('Origin',(1.63623295246351,6.18563622669654,19.0374307818588));
#61463=CARTESIAN_POINT('',(1.90706327644678,5.04583540480242,16.998194874094));
#61464=CARTESIAN_POINT('',(1.90706327644678,5.90912166928202,16.7176961632773));
#61465=CARTESIAN_POINT('Ctrl Pts',(1.90706327644678,5.04583540480242,16.998194874094));
#61466=CARTESIAN_POINT('Ctrl Pts',(1.90026014393029,5.04567196333426,16.9976225239826));
#61467=CARTESIAN_POINT('Ctrl Pts',(1.89355517781933,5.04653705366496,16.9967539081093));
#61468=CARTESIAN_POINT('Ctrl Pts',(1.87732280058991,5.05101511023685,16.9939422782637));
#61469=CARTESIAN_POINT('Ctrl Pts',(1.86840987580674,5.05560766488492,16.9917638647488));
#61470=CARTESIAN_POINT('Ctrl Pts',(1.84749974154034,5.07034930389402,16.985463318489));
#61471=CARTESIAN_POINT('Ctrl Pts',(1.83650132567019,5.08235904211366,16.980871661332));
#61472=CARTESIAN_POINT('Ctrl Pts',(1.81085694928173,5.11736200896834,16.9680241697438));
#61473=CARTESIAN_POINT('Ctrl Pts',(1.79594323550246,5.1473702565999,16.9576102181473));
#61474=CARTESIAN_POINT('Ctrl Pts',(1.76902539468134,5.22698753163543,16.9307871685188));
#61475=CARTESIAN_POINT('Ctrl Pts',(1.75949337448623,5.27332224828677,16.9155448309957));
#61476=CARTESIAN_POINT('Ctrl Pts',(1.74741836256394,5.36043234407138,16.8870291804704));
#61477=CARTESIAN_POINT('Ctrl Pts',(1.74418490387289,5.40452184219647,16.8726745751501));
#61478=CARTESIAN_POINT('Ctrl Pts',(1.74230474178709,5.49027879637106,16.8447903345418));
#61479=CARTESIAN_POINT('Ctrl Pts',(1.7435605120278,5.53376566269685,16.8306696144911));
#61480=CARTESIAN_POINT('Ctrl Pts',(1.75089245923107,5.62039732386606,16.802619637761));
#61481=CARTESIAN_POINT('Ctrl Pts',(1.75736442403595,5.66589231855086,16.7879279245166));
#61482=CARTESIAN_POINT('Ctrl Pts',(1.77948145071066,5.76057523481867,16.7577464575557));
#61483=CARTESIAN_POINT('Ctrl Pts',(1.79536357091661,5.80338352888465,16.7443881182381));
#61484=CARTESIAN_POINT('Ctrl Pts',(1.82385809602974,5.85279728585439,16.7297952066032));
#61485=CARTESIAN_POINT('Ctrl Pts',(1.83844662204132,5.87421791437856,16.7236372532295));
#61486=CARTESIAN_POINT('Ctrl Pts',(1.86612294571255,5.89600163036716,16.7185311380393));
#61487=CARTESIAN_POINT('Ctrl Pts',(1.87511027899494,5.90137286940023,16.7174688556404));
#61488=CARTESIAN_POINT('Ctrl Pts',(1.88937385988136,5.90645548339465,16.7169970261612));
#61489=CARTESIAN_POINT('Ctrl Pts',(1.89395673353182,5.90763715542309,16.7170046598605));
#61490=CARTESIAN_POINT('Ctrl Pts',(1.90144341439934,5.9087805761035,16.7172952459867));
#61491=CARTESIAN_POINT('Ctrl Pts',(1.90425145406818,5.90903727408375,16.7174650761326));
#61492=CARTESIAN_POINT('Ctrl Pts',(1.90706327644678,5.90912166928202,16.7176961632773));
#61493=CARTESIAN_POINT('',(1.62584114411962,3.94856638716317,19.7629572175357));
#61494=CARTESIAN_POINT('Origin',(1.62584114411962,6.18524193534253,19.0362172778497));
#61495=CARTESIAN_POINT('',(1.33846910697111,4.22280591656415,19.6367507067188));
#61496=CARTESIAN_POINT('Origin',(1.63623295246351,4.23410382602581,19.6715220966734));
#61497=CARTESIAN_POINT('Origin',(1.33846910697111,6.17433831723488,19.0026593919042));
#61498=CARTESIAN_POINT('Origin',(1.62584114411962,6.18524193534253,19.0362172778497));
#61499=CARTESIAN_POINT('Origin',(5.83867335851287,6.34508738889865,19.5281709987517));
#61500=CARTESIAN_POINT('',(10.3480326234796,5.24947731735612,17.7080825054385));
#61501=CARTESIAN_POINT('Ctrl Pts',(10.3480326234796,5.24947731735613,17.7080825054385));
#61502=CARTESIAN_POINT('Ctrl Pts',(7.54972025675578,5.18170180546196,17.4728227255228));
#61503=CARTESIAN_POINT('Ctrl Pts',(4.7091881268347,5.11315489305578,17.233938697471));
#61504=CARTESIAN_POINT('Ctrl Pts',(1.90706327644678,5.04583540480243,16.998194874094));
#61505=CARTESIAN_POINT('',(10.0307219562183,3.9862326678566,20.8358167812138));
#61506=CARTESIAN_POINT('Origin',(10.0307219562183,6.50414425974677,20.0176977116355));
#61507=CARTESIAN_POINT('',(10.3480326234796,6.16163338174817,17.4117050340792));
#61508=CARTESIAN_POINT('Origin',(10.0307219562183,6.50414425974677,20.0176977116355));
#61509=CARTESIAN_POINT('Ctrl Pts',(1.90706327644678,5.90912166928201,16.7176961632773));
#61510=CARTESIAN_POINT('Ctrl Pts',(4.70918812184411,5.99322580178265,16.9479863246852));
#61511=CARTESIAN_POINT('Ctrl Pts',(7.54972025123708,6.07818269341642,17.1815384272226));
#61512=CARTESIAN_POINT('Ctrl Pts',(10.3480326234796,6.16163338174816,17.4117050340792));
#61513=CARTESIAN_POINT('Origin',(10.0411137645622,6.50453855110077,20.0189112156446));
#61514=CARTESIAN_POINT('',(10.3388776100546,4.28306801618089,20.7791530503061));
#61515=CARTESIAN_POINT('Origin',(10.3388776100546,6.51583646056242,20.0536826055992));
#61516=CARTESIAN_POINT('Origin',(10.0411137645622,4.27177010671924,20.7443816603515));
#61517=CARTESIAN_POINT('Ctrl Pts',(10.3480326234796,6.16163338174815,17.4117050340792));
#61518=CARTESIAN_POINT('Ctrl Pts',(10.3515114639741,6.16173712700431,17.4119911754408));
#61519=CARTESIAN_POINT('Ctrl Pts',(10.3549914179992,6.16156241574046,17.4123759675224));
#61520=CARTESIAN_POINT('Ctrl Pts',(10.3584662558372,6.16110903077378,17.4128588642783));
#61521=CARTESIAN_POINT('Ctrl Pts',(10.367223098271,6.15996646789744,17.4140757989961));
#61522=CARTESIAN_POINT('Ctrl Pts',(10.3753630700178,6.15713972282256,17.415831290242));
#61523=CARTESIAN_POINT('Ctrl Pts',(10.3939290316259,6.14753302482072,17.4209477623239));
#61524=CARTESIAN_POINT('Ctrl Pts',(10.4035780672154,6.13952487259415,17.4246680145472));
#61525=CARTESIAN_POINT('Ctrl Pts',(10.4280013399752,6.11408837463521,17.435881088904));
#61526=CARTESIAN_POINT('Ctrl Pts',(10.4407678160189,6.09300205845735,17.4444479537233));
#61527=CARTESIAN_POINT('Ctrl Pts',(10.4685456259697,6.03626400623263,17.466763669083));
#61528=CARTESIAN_POINT('Ctrl Pts',(10.4828713837316,5.99063505235348,17.4838345078959));
#61529=CARTESIAN_POINT('Ctrl Pts',(10.5038238234649,5.88674071610145,17.5210208246161));
#61530=CARTESIAN_POINT('Ctrl Pts',(10.5097149363751,5.83272996465091,17.5396167538765));
#61531=CARTESIAN_POINT('Ctrl Pts',(10.5152093525458,5.72672134143426,17.5750286675881));
#61532=CARTESIAN_POINT('Ctrl Pts',(10.5146501294348,5.67139291388386,17.5929043782428));
#61533=CARTESIAN_POINT('Ctrl Pts',(10.5071723447785,5.56539053344041,17.6260374509827));
#61534=CARTESIAN_POINT('Ctrl Pts',(10.5000174147823,5.51115999516818,17.6424047527202));
#61535=CARTESIAN_POINT('Ctrl Pts',(10.4763655908935,5.40677101623327,17.6725219279296));
#61536=CARTESIAN_POINT('Ctrl Pts',(10.4605419031699,5.36240927189391,17.6845328147318));
#61537=CARTESIAN_POINT('Ctrl Pts',(10.4319469960435,5.3095053807161,17.6978522663517));
#61538=CARTESIAN_POINT('Ctrl Pts',(10.4192298015583,5.29065702126869,17.7023303304535));
#61539=CARTESIAN_POINT('Ctrl Pts',(10.3949786188434,5.26742227944473,17.7070402629162));
#61540=CARTESIAN_POINT('Ctrl Pts',(10.3846960006404,5.25993527526376,17.708325726784));
#61541=CARTESIAN_POINT('Ctrl Pts',(10.3651744504234,5.2516475721963,17.7090036066899));
#61542=CARTESIAN_POINT('Ctrl Pts',(10.3566858346072,5.24968689932441,17.708809998398));
#61543=CARTESIAN_POINT('Ctrl Pts',(10.3480326234796,5.24947731735612,17.7080825054385));
#61544=CARTESIAN_POINT('Origin',(10.3388776100546,6.51583646056242,20.0536826055992));
#61545=CARTESIAN_POINT('Origin',(1.05309141530195,6.89256018399713,21.2131190072776));
#61546=CARTESIAN_POINT('Origin',(1.63623295246351,11.7657792816622,16.1942058835342));
#61547=CARTESIAN_POINT('',(1.90706327644678,10.0516057316823,14.6069951093592));
#61548=CARTESIAN_POINT('',(1.90706327644678,10.7859608904011,14.0734548558899));
#61549=CARTESIAN_POINT('Ctrl Pts',(1.90706327644678,10.0516057316823,14.6069951093592));
#61550=CARTESIAN_POINT('Ctrl Pts',(1.90025875960789,10.0512733560788,14.6065011777611));
#61551=CARTESIAN_POINT('Ctrl Pts',(1.89355247269393,10.0518279831462,14.6054074046248));
#61552=CARTESIAN_POINT('Ctrl Pts',(1.87725698375373,10.0552320469981,14.6013332347425));
#61553=CARTESIAN_POINT('Ctrl Pts',(1.86829211419482,10.0589614875642,14.5978127562127));
#61554=CARTESIAN_POINT('Ctrl Pts',(1.84706044347936,10.0712702530583,14.587068386758));
#61555=CARTESIAN_POINT('Ctrl Pts',(1.83585892185112,10.0815819441639,14.5787550531416));
#61556=CARTESIAN_POINT('Ctrl Pts',(1.80877471345797,10.1129760302182,14.5541268705482));
#61557=CARTESIAN_POINT('Ctrl Pts',(1.79294392498847,10.1410429474215,14.5329375758416));
#61558=CARTESIAN_POINT('Ctrl Pts',(1.76567283597218,10.2144033500568,14.4785632453837));
#61559=CARTESIAN_POINT('Ctrl Pts',(1.75650699269186,10.2562595787951,14.44796672798));
#61560=CARTESIAN_POINT('Ctrl Pts',(1.74778527726996,10.318451044183,14.402618654485));
#61561=CARTESIAN_POINT('Ctrl Pts',(1.74564598164335,10.340877007659,14.3862953920437));
#61562=CARTESIAN_POINT('Ctrl Pts',(1.74342903876675,10.3797436057755,14.3580271947077));
#61563=CARTESIAN_POINT('Ctrl Pts',(1.74295490171611,10.396426456047,14.3459008172415));
#61564=CARTESIAN_POINT('Ctrl Pts',(1.74292857696576,10.4295927678065,14.3218037566096));
#61565=CARTESIAN_POINT('Ctrl Pts',(1.74337239383371,10.4462099845875,14.3097358503644));
#61566=CARTESIAN_POINT('Ctrl Pts',(1.74549594744663,10.4847417370596,14.2817694324059));
#61567=CARTESIAN_POINT('Ctrl Pts',(1.74755180318335,10.506894590928,14.2657028933402));
#61568=CARTESIAN_POINT('Ctrl Pts',(1.75591196457193,10.5681486124416,14.2213535217066));
#61569=CARTESIAN_POINT('Ctrl Pts',(1.76464297432621,10.6092002023613,14.1917029071035));
#61570=CARTESIAN_POINT('Ctrl Pts',(1.79360739934227,10.691226532163,14.1332147014354));
#61571=CARTESIAN_POINT('Ctrl Pts',(1.81322842074793,10.7250788098356,14.1096237409573));
#61572=CARTESIAN_POINT('Ctrl Pts',(1.8474511327919,10.7612654174966,14.0857929378105));
#61573=CARTESIAN_POINT('Ctrl Pts',(1.85980439378151,10.7703887241704,14.0801722471136));
#61574=CARTESIAN_POINT('Ctrl Pts',(1.87846606193859,10.7796242046072,14.0751582426548));
#61575=CARTESIAN_POINT('Ctrl Pts',(1.88517766043229,10.7821409674905,14.073969752852));
#61576=CARTESIAN_POINT('Ctrl Pts',(1.89712731919191,10.7849686486851,14.0731201278146));
#61577=CARTESIAN_POINT('Ctrl Pts',(1.90207774196477,10.7856919622331,14.0731114184824));
#61578=CARTESIAN_POINT('Ctrl Pts',(1.90706327644678,10.7859608904011,14.0734548558899));
#61579=CARTESIAN_POINT('',(1.62584114411962,9.86239943185911,17.5755151259486));
#61580=CARTESIAN_POINT('Origin',(1.62584114411962,11.7650292949391,16.1931736153679));
#61581=CARTESIAN_POINT('',(1.33846910697111,10.0842167666784,17.3707409263229));
#61582=CARTESIAN_POINT('Origin',(1.63623295246351,10.1057066675065,17.4003192372954));
#61583=CARTESIAN_POINT('Origin',(1.33846910697111,11.7442893808342,16.1646275725617));
#61584=CARTESIAN_POINT('Origin',(1.62584114411962,11.7650292949391,16.1931736153679));
#61585=CARTESIAN_POINT('Origin',(5.83867335851287,12.0690734153485,16.611654445725));
#61586=CARTESIAN_POINT('',(10.3480326234796,10.4646480417893,15.2192095552406));
#61587=CARTESIAN_POINT('Ctrl Pts',(10.3480326234796,10.4646480417893,15.2192095552406));
#61588=CARTESIAN_POINT('Ctrl Pts',(7.54753623341465,10.3273833808683,15.0162497111978));
#61589=CARTESIAN_POINT('Ctrl Pts',(4.70781617470128,10.1884122025895,14.8102983544992));
#61590=CARTESIAN_POINT('Ctrl Pts',(1.90706327644678,10.0516057316823,14.6069951093592));
#61591=CARTESIAN_POINT('',(10.0307219562183,10.2297540313114,18.584225684205));
#61592=CARTESIAN_POINT('Origin',(10.0307219562183,12.3716175623118,17.0280707397496));
#61593=CARTESIAN_POINT('',(10.3480326234796,11.2405743353076,14.655466104402));
#61594=CARTESIAN_POINT('Origin',(10.0307219562183,12.3716175623118,17.0280707397496));
#61595=CARTESIAN_POINT('Ctrl Pts',(1.90706327644677,10.7859608904011,14.0734548558899));
#61596=CARTESIAN_POINT('Ctrl Pts',(4.70781616958245,10.9370382417485,14.2663896989247));
#61597=CARTESIAN_POINT('Ctrl Pts',(7.54753622799762,11.0899651657448,14.4622016128173));
#61598=CARTESIAN_POINT('Ctrl Pts',(10.3480326234796,11.2405743353076,14.655466104402));
#61599=CARTESIAN_POINT('Origin',(10.0411137645622,12.3723675490348,17.0291030079158));
#61600=CARTESIAN_POINT('',(10.3388776100546,10.4945511677868,18.4386081065242));
#61601=CARTESIAN_POINT('Origin',(10.3388776100546,12.3938574498629,17.0586813188882));
#61602=CARTESIAN_POINT('Origin',(10.0411137645622,10.4730612669588,18.4090297955518));
#61603=CARTESIAN_POINT('Ctrl Pts',(10.3480326234796,11.2405743353076,14.655466104402));
#61604=CARTESIAN_POINT('Ctrl Pts',(10.3515211595623,11.2407619468765,14.6557068510616));
#61605=CARTESIAN_POINT('Ctrl Pts',(10.3550011198928,11.2407133851835,14.656127803182));
#61606=CARTESIAN_POINT('Ctrl Pts',(10.3584662558372,11.2404322010368,14.6567254954937));
#61607=CARTESIAN_POINT('Ctrl Pts',(10.3671694892744,11.2397259628669,14.658226693656));
#61608=CARTESIAN_POINT('Ctrl Pts',(10.3753654465597,11.2375879642563,14.6607699081134));
#61609=CARTESIAN_POINT('Ctrl Pts',(10.3941492137284,11.2299109713814,14.6687216746163));
#61610=CARTESIAN_POINT('Ctrl Pts',(10.404002965845,11.2232825987702,14.6748808959337));
#61611=CARTESIAN_POINT('Ctrl Pts',(10.4308436412036,11.2002100598277,14.695462505518));
#61612=CARTESIAN_POINT('Ctrl Pts',(10.4443760953691,11.1799381757229,14.7123773258611));
#61613=CARTESIAN_POINT('Ctrl Pts',(10.4751024728256,11.1253565526287,14.7571304838428));
#61614=CARTESIAN_POINT('Ctrl Pts',(10.4913920727398,11.0748241683188,14.7969697951179));
#61615=CARTESIAN_POINT('Ctrl Pts',(10.5062952995223,10.9899781948954,14.8615728881703));
#61616=CARTESIAN_POINT('Ctrl Pts',(10.5095242362634,10.9629200882247,14.8818952699719));
#61617=CARTESIAN_POINT('Ctrl Pts',(10.512859180135,10.9184305611831,14.9149069041021));
#61618=CARTESIAN_POINT('Ctrl Pts',(10.5136719991087,10.9006780007667,14.9279744210186));
#61619=CARTESIAN_POINT('Ctrl Pts',(10.514295657022,10.8670882523063,14.9525087414763));
#61620=CARTESIAN_POINT('Ctrl Pts',(10.5142026737932,10.8511355186813,14.9640796299257));
#61621=CARTESIAN_POINT('Ctrl Pts',(10.5131483322071,10.8161050999278,14.9893112870104));
#61622=CARTESIAN_POINT('Ctrl Pts',(10.512009812725,10.7968758883502,15.0030451759509));
#61623=CARTESIAN_POINT('Ctrl Pts',(10.5074172692912,10.7460384791957,15.0390378011655));
#61624=CARTESIAN_POINT('Ctrl Pts',(10.5028514263372,10.7137256630153,15.0615825002596));
#61625=CARTESIAN_POINT('Ctrl Pts',(10.4823258875198,10.615975646757,15.128610374523));
#61626=CARTESIAN_POINT('Ctrl Pts',(10.4610892332282,10.561524835807,15.1642626717182));
#61627=CARTESIAN_POINT('Ctrl Pts',(10.4253700252926,10.5103262009137,15.1959357631406));
#61628=CARTESIAN_POINT('Ctrl Pts',(10.4122912190472,10.4944454192632,15.2055154329318));
#61629=CARTESIAN_POINT('Ctrl Pts',(10.3868737804665,10.4762419431139,15.2153586960742));
#61630=CARTESIAN_POINT('Ctrl Pts',(10.3771760707494,10.4710384088583,15.2179090290457));
#61631=CARTESIAN_POINT('Ctrl Pts',(10.3604838650278,10.4660465521434,15.2195700377639));
#61632=CARTESIAN_POINT('Ctrl Pts',(10.35429238307,10.4649548601736,15.2196632176109));
#61633=CARTESIAN_POINT('Ctrl Pts',(10.3480326234796,10.4646480417893,15.2192095552406));
#61634=CARTESIAN_POINT('Origin',(10.3388776100546,12.3938574498629,17.0586813188882));
#61635=CARTESIAN_POINT('Origin',(1.05309141530195,13.110428553894,18.0449568312087));
#61636=CARTESIAN_POINT('Origin',(1.63623295246351,16.1942058835342,11.7657792816622));
#61637=CARTESIAN_POINT('',(1.90706327644678,14.0734548558899,10.7859608904011));
#61638=CARTESIAN_POINT('',(1.90706327644678,14.6069951093592,10.0516057316823));
#61639=CARTESIAN_POINT('Ctrl Pts',(1.90706327644678,14.0734548558899,10.7859608904011));
#61640=CARTESIAN_POINT('Ctrl Pts',(1.90025875962072,14.0729861146493,10.7855938432468));
#61641=CARTESIAN_POINT('Ctrl Pts',(1.89355247271419,14.0731756018455,10.7843822139941));
#61642=CARTESIAN_POINT('Ctrl Pts',(1.87725698375408,14.0751540712245,10.779455534593));
#61643=CARTESIAN_POINT('Ctrl Pts',(1.86829211419522,14.0776130922829,10.7749549000324));
#61644=CARTESIAN_POINT('Ctrl Pts',(1.84706044347974,14.0859992311583,10.7609327797317));
#61645=CARTESIAN_POINT('Ctrl Pts',(1.83585892185151,14.0932372708108,10.7498398418314));
#61646=CARTESIAN_POINT('Ctrl Pts',(1.80877471345856,14.1154842939635,10.7167157421782));
#61647=CARTESIAN_POINT('Ctrl Pts',(1.79294392498912,14.1356296662986,10.6878903709767));
#61648=CARTESIAN_POINT('Ctrl Pts',(1.76567283597254,14.1885969630935,10.6135076985472));
#61649=CARTESIAN_POINT('Ctrl Pts',(1.75650699269207,14.2189497583364,10.5714743952936));
#61650=CARTESIAN_POINT('Ctrl Pts',(1.74778527727003,14.2640840313797,10.5091275947844));
#61651=CARTESIAN_POINT('Ctrl Pts',(1.7456459816434,14.2803682245799,10.4866732458429));
#61652=CARTESIAN_POINT('Ctrl Pts',(1.74342903876676,14.3085972026078,10.4477781532308));
#61653=CARTESIAN_POINT('Ctrl Pts',(1.74295490171613,14.3207162793518,10.4310899986739));
#61654=CARTESIAN_POINT('Ctrl Pts',(1.74292857696576,14.3448129150219,10.3979233781626));
#61655=CARTESIAN_POINT('Ctrl Pts',(1.74337239383368,14.356887639208,10.3813111149054));
#61656=CARTESIAN_POINT('Ctrl Pts',(1.74549594744658,14.38489141506,10.3428065045313));
#61657=CARTESIAN_POINT('Ctrl Pts',(1.74755180318328,14.4009951974739,10.3206807095396));
#61658=CARTESIAN_POINT('Ctrl Pts',(1.75591196457173,14.4455465242587,10.2595734170327));
#61659=CARTESIAN_POINT('Ctrl Pts',(1.76464297432586,14.4754263625499,10.2186883678714));
#61660=CARTESIAN_POINT('Ctrl Pts',(1.79360739934126,14.535364188493,10.1377152488502));
#61661=CARTESIAN_POINT('Ctrl Pts',(1.81322842074649,14.5602696100637,10.1048179830625));
#61662=CARTESIAN_POINT('Ctrl Pts',(1.84745113279067,14.5873209959212,10.0709712657039));
#61663=CARTESIAN_POINT('Ctrl Pts',(1.85980439378038,14.5942608872381,10.0628064143832));
#61664=CARTESIAN_POINT('Ctrl Pts',(1.87846606193765,14.6014949385013,10.0551838923634));
#61665=CARTESIAN_POINT('Ctrl Pts',(1.88517766043151,14.6035212586948,10.05327584889));
#61666=CARTESIAN_POINT('Ctrl Pts',(1.89712731920684,14.6059479947488,10.0515940059157));
#61667=CARTESIAN_POINT('Ctrl Pts',(1.90207774197487,14.6066332154779,10.0513622066726));
#61668=CARTESIAN_POINT('Ctrl Pts',(1.90706327644678,14.6069951093592,10.0516057316823));
#61669=CARTESIAN_POINT('',(1.62584114411962,14.8108321047873,13.6676591580191));
#61670=CARTESIAN_POINT('Origin',(1.62584114411962,16.1931736153679,11.7650292949391));
#61671=CARTESIAN_POINT('',(1.33846910697111,14.9585142188006,13.4043619949899));
#61672=CARTESIAN_POINT('Origin',(1.63623295246351,14.988092529773,13.425851895818));
#61673=CARTESIAN_POINT('Origin',(1.33846910697111,16.1646275725617,11.7442893808342));
#61674=CARTESIAN_POINT('Origin',(1.62584114411962,16.1931736153679,11.7650292949391));
#61675=CARTESIAN_POINT('Origin',(5.83867335851287,16.611654445725,12.0690734153485));
#61676=CARTESIAN_POINT('',(10.3480326234796,14.655466104402,11.2405743353076));
#61677=CARTESIAN_POINT('Ctrl Pts',(10.3480326234796,14.655466104402,11.2405743353076));
#61678=CARTESIAN_POINT('Ctrl Pts',(7.54753623341465,14.4622016131911,11.0899651660362));
#61679=CARTESIAN_POINT('Ctrl Pts',(4.70781617470128,14.2663896992774,10.9370382420246));
#61680=CARTESIAN_POINT('Ctrl Pts',(1.90706327644678,14.0734548558899,10.7859608904011));
#61681=CARTESIAN_POINT('',(10.0307219562183,15.4719157952941,14.5134810933121));
#61682=CARTESIAN_POINT('Origin',(10.0307219562183,17.0280707397496,12.3716175623118));
#61683=CARTESIAN_POINT('',(10.3480326234796,15.2192095552406,10.4646480417893));
#61684=CARTESIAN_POINT('Origin',(10.0307219562183,17.0280707397496,12.3716175623118));
#61685=CARTESIAN_POINT('Ctrl Pts',(1.90706327644678,14.6069951093592,10.0516057316823));
#61686=CARTESIAN_POINT('Ctrl Pts',(4.70781616958245,14.8102983541277,10.1884122023394));
#61687=CARTESIAN_POINT('Ctrl Pts',(7.54753622799762,15.0162497108052,10.3273833806028));
#61688=CARTESIAN_POINT('Ctrl Pts',(10.3480326234796,15.2192095552406,10.4646480417893));
#61689=CARTESIAN_POINT('Origin',(10.0411137645622,17.0291030079158,12.3723675490348));
#61690=CARTESIAN_POINT('',(10.3388776100546,15.6787545312522,14.293163731939));
#61691=CARTESIAN_POINT('Origin',(10.3388776100546,17.0586813188882,12.3938574498629));
#61692=CARTESIAN_POINT('Origin',(10.0411137645622,15.6491762202798,14.2716738311109));
#61693=CARTESIAN_POINT('Ctrl Pts',(10.3480326234796,15.2192095552406,10.4646480417893));
#61694=CARTESIAN_POINT('Ctrl Pts',(10.3515211595623,15.2194623792549,10.4648190303056));
#61695=CARTESIAN_POINT('Ctrl Pts',(10.3550011198928,15.2195462756993,10.4652343859512));
#61696=CARTESIAN_POINT('Ctrl Pts',(10.3584662558372,15.219463550766,10.4658897157988));
#61697=CARTESIAN_POINT('Ctrl Pts',(10.3671694892744,15.2192557740966,10.46753567969));
#61698=CARTESIAN_POINT('Ctrl Pts',(10.3753654465597,15.2180083130739,10.4706150982766));
#61699=CARTESIAN_POINT('Ctrl Pts',(10.3941492137284,15.2131642899593,10.4805499988893));
#61700=CARTESIAN_POINT('Ctrl Pts',(10.404002965845,15.2087636370542,10.4884560462404));
#61701=CARTESIAN_POINT('Ctrl Pts',(10.4308436412036,15.1931804156785,10.515160126788));
#61702=CARTESIAN_POINT('Ctrl Pts',(10.4443760953691,15.1791276751459,10.5375114335937));
#61703=CARTESIAN_POINT('Ctrl Pts',(10.4751024728252,15.141046953201,10.5969408652329));
#61704=CARTESIAN_POINT('Ctrl Pts',(10.4913920727396,15.1052988240476,10.6504456673435));
#61705=CARTESIAN_POINT('Ctrl Pts',(10.5062952995223,15.0445689617835,10.738105707657));
#61706=CARTESIAN_POINT('Ctrl Pts',(10.5095242362634,15.0251151344585,10.7657948560931));
#61707=CARTESIAN_POINT('Ctrl Pts',(10.512859180135,14.9930042358173,10.8109388057733));
#61708=CARTESIAN_POINT('Ctrl Pts',(10.5136719991087,14.980158632354,10.8288525957506));
#61709=CARTESIAN_POINT('Ctrl Pts',(10.514295657022,14.9557944051665,10.8625659242064));
#61710=CARTESIAN_POINT('Ctrl Pts',(10.5142026737932,14.9441980550706,10.8785001588623));
#61711=CARTESIAN_POINT('Ctrl Pts',(10.5131483322071,14.918679157882,10.9133218854645));
#61712=CARTESIAN_POINT('Ctrl Pts',(10.512009812725,14.9046350959894,10.9323257432013));
#61713=CARTESIAN_POINT('Ctrl Pts',(10.5074172692912,14.867408179605,10.982266387329));
#61714=CARTESIAN_POINT('Ctrl Pts',(10.5028514263372,14.8436435603699,11.0136928796461));
#61715=CARTESIAN_POINT('Ctrl Pts',(10.4823258875198,14.7713905226838,11.1076465924618));
#61716=CARTESIAN_POINT('Ctrl Pts',(10.4610892332284,14.7306218898341,11.1583801679713));
#61717=CARTESIAN_POINT('Ctrl Pts',(10.4253700252926,14.691716618007,11.204324316231));
#61718=CARTESIAN_POINT('Ctrl Pts',(10.4122912190472,14.6795733779005,11.2183425550237));
#61719=CARTESIAN_POINT('Ctrl Pts',(10.3868737804666,14.6653025788806,11.2333292380637));
#61720=CARTESIAN_POINT('Ctrl Pts',(10.3771760707494,14.6611418199486,11.2373627293707));
#61721=CARTESIAN_POINT('Ctrl Pts',(10.3604838650278,14.6569075620133,11.2404850110942));
#61722=CARTESIAN_POINT('Ctrl Pts',(10.35429238307,14.6558980954078,11.2409109817661));
#61723=CARTESIAN_POINT('Ctrl Pts',(10.3480326234796,14.655466104402,11.2405743353076));
#61724=CARTESIAN_POINT('Origin',(10.3388776100546,17.0586813188882,12.3938574498629));
#61725=CARTESIAN_POINT('Origin',(1.05309141530195,18.0449568312087,13.110428553894));
#61726=CARTESIAN_POINT('Origin',(1.63623295246351,19.0374307818588,6.18563622669653));
#61727=CARTESIAN_POINT('',(1.90706327644678,16.7176961632773,5.90912166928202));
#61728=CARTESIAN_POINT('',(1.90706327644678,16.998194874094,5.04583540480242));
#61729=CARTESIAN_POINT('Ctrl Pts',(1.90706327644678,16.7176961632773,5.90912166928201));
#61730=CARTESIAN_POINT('Ctrl Pts',(1.90026014388931,16.7171370538224,5.90891747725146));
#61731=CARTESIAN_POINT('Ctrl Pts',(1.89355517775467,16.7169428161624,5.90770704485232));
#61732=CARTESIAN_POINT('Ctrl Pts',(1.87732280058928,16.7173002954459,5.90243158644642));
#61733=CARTESIAN_POINT('Ctrl Pts',(1.86840987580604,16.7182373577842,5.89743569235092));
#61734=CARTESIAN_POINT('Ctrl Pts',(1.84749974153964,16.7218050267904,5.88180608769448));
#61735=CARTESIAN_POINT('Ctrl Pts',(1.83650132566944,16.7251494451274,5.86939109701612));
#61736=CARTESIAN_POINT('Ctrl Pts',(1.81085694928076,16.7353298338014,5.83352153589184));
#61737=CARTESIAN_POINT('Ctrl Pts',(1.79594323550141,16.7445431753865,5.80312318641932));
#61738=CARTESIAN_POINT('Ctrl Pts',(1.76902539468055,16.76964073249,5.7229452648757));
#61739=CARTESIAN_POINT('Ctrl Pts',(1.75949337448563,16.7845442855166,5.67650047046868));
#61740=CARTESIAN_POINT('Ctrl Pts',(1.74741836256365,16.812676669264,5.58926584375912));
#61741=CARTESIAN_POINT('Ctrl Pts',(1.74418490387271,16.8269787063912,5.54515926519279));
#61742=CARTESIAN_POINT('Ctrl Pts',(1.74230474178712,16.8548265548092,5.45939048647873));
#61743=CARTESIAN_POINT('Ctrl Pts',(1.74356051202795,16.8689635910101,5.41590892159149));
#61744=CARTESIAN_POINT('Ctrl Pts',(1.75089245923146,16.8971914959605,5.32933507280557));
#61745=CARTESIAN_POINT('Ctrl Pts',(1.7573644240365,16.9120469371982,5.28389327657052));
#61746=CARTESIAN_POINT('Ctrl Pts',(1.77948145071182,16.9432828393381,5.18955296706001));
#61747=CARTESIAN_POINT('Ctrl Pts',(1.79536357091814,16.9576377997412,5.14706849481492));
#61748=CARTESIAN_POINT('Ctrl Pts',(1.82385809603028,16.9748765638374,5.09851442742642));
#61749=CARTESIAN_POINT('Ctrl Pts',(1.83844662204054,16.9824854044481,5.07756522074461));
#61750=CARTESIAN_POINT('Ctrl Pts',(1.8661229457107,16.9911586174823,5.05694052510362));
#61751=CARTESIAN_POINT('Ctrl Pts',(1.8751102789935,16.993456348059,5.05197070751669));
#61752=CARTESIAN_POINT('Ctrl Pts',(1.88937385988036,16.9960621155411,5.04758145200955));
#61753=CARTESIAN_POINT('Ctrl Pts',(1.89395673353113,16.996762860725,5.04662994623251));
#61754=CARTESIAN_POINT('Ctrl Pts',(1.90144341432864,16.9976700356441,5.04587570171682));
#61755=CARTESIAN_POINT('Ctrl Pts',(1.90425145401561,16.9979583144095,5.04576785233519));
#61756=CARTESIAN_POINT('Ctrl Pts',(1.90706327644678,16.998194874094,5.04583540480242));
#61757=CARTESIAN_POINT('',(1.62584114411962,18.3094773381637,8.42191748352189));
#61758=CARTESIAN_POINT('Origin',(1.62584114411962,19.0362172778497,6.18524193534253));
#61759=CARTESIAN_POINT('',(1.33846910697111,18.3685680770895,8.12587071790561));
#61760=CARTESIAN_POINT('Origin',(1.63623295246351,18.4033394670442,8.13716862736726));
#61761=CARTESIAN_POINT('Origin',(1.33846910697111,19.0026593919042,6.17433831723488));
#61762=CARTESIAN_POINT('Origin',(1.62584114411962,19.0362172778497,6.18524193534253));
#61763=CARTESIAN_POINT('Origin',(5.83867335851287,19.5281709987517,6.34508738889865));
#61764=CARTESIAN_POINT('',(10.3480326234796,17.4117050340792,6.16163338174817));
#61765=CARTESIAN_POINT('Ctrl Pts',(10.3480326234796,17.4117050340792,6.16163338174816));
#61766=CARTESIAN_POINT('Ctrl Pts',(7.54972025675578,17.1815384276765,6.078182693581));
#61767=CARTESIAN_POINT('Ctrl Pts',(4.7091881268347,16.9479863250953,5.99322580193243));
#61768=CARTESIAN_POINT('Ctrl Pts',(1.90706327644678,16.7176961632773,5.90912166928201));
#61769=CARTESIAN_POINT('',(10.0307219562183,19.1995786420573,9.02205585163693));
#61770=CARTESIAN_POINT('Origin',(10.0307219562183,20.0176977116355,6.50414425974677));
#61771=CARTESIAN_POINT('',(10.3480326234796,17.7080825054385,5.24947731735612));
#61772=CARTESIAN_POINT('Origin',(10.0307219562183,20.0176977116355,6.50414425974677));
#61773=CARTESIAN_POINT('Ctrl Pts',(1.90706327644677,16.998194874094,5.04583540480243));
#61774=CARTESIAN_POINT('Ctrl Pts',(4.70918812184411,17.2339386970511,5.11315489293588));
#61775=CARTESIAN_POINT('Ctrl Pts',(7.54972025123709,17.4728227250588,5.18170180532829));
#61776=CARTESIAN_POINT('Ctrl Pts',(10.3480326234796,17.7080825054385,5.24947731735613));
#61777=CARTESIAN_POINT('Origin',(10.0411137645622,20.0189112156446,6.50453855110077));
#61778=CARTESIAN_POINT('',(10.3388776100546,19.3282121608924,8.74860490494395));
#61779=CARTESIAN_POINT('Origin',(10.3388776100546,20.0536826055992,6.51583646056242));
#61780=CARTESIAN_POINT('Origin',(10.0411137645622,19.2934407709377,8.73730699548229));
#61781=CARTESIAN_POINT('Ctrl Pts',(10.3480326234796,17.7080825054385,5.24947731735611));
#61782=CARTESIAN_POINT('Ctrl Pts',(10.3515114639741,17.7083749785944,5.24956157535322));
#61783=CARTESIAN_POINT('Ctrl Pts',(10.3549914179992,17.7085835892234,5.24992909484555));
#61784=CARTESIAN_POINT('Ctrl Pts',(10.3584662558372,17.7087077679084,5.25057973058012));
#61785=CARTESIAN_POINT('Ctrl Pts',(10.367223098271,17.7090207071676,5.25221937964431));
#61786=CARTESIAN_POINT('Ctrl Pts',(10.3753630700179,17.708779410352,5.25553811631362));
#61787=CARTESIAN_POINT('Ctrl Pts',(10.3939290316259,17.7072720478088,5.26631748509037));
#61788=CARTESIAN_POINT('Ctrl Pts',(10.4035780672154,17.705574721304,5.27498292572686));
#61789=CARTESIAN_POINT('Ctrl Pts',(10.4280013399751,17.6996950906475,5.30215236459277));
#61790=CARTESIAN_POINT('Ctrl Pts',(10.4407678160188,17.6942316042004,5.32424702952845));
#61791=CARTESIAN_POINT('Ctrl Pts',(10.4685456259696,17.6789356068265,5.38326592638877));
#61792=CARTESIAN_POINT('Ctrl Pts',(10.4828713837316,17.6659261793668,5.43021451281097));
#61793=CARTESIAN_POINT('Ctrl Pts',(10.5038238234649,17.6349429829058,5.5361243650136));
#61794=CARTESIAN_POINT('Ctrl Pts',(10.5097149363751,17.6182406825358,5.59075039378809));
#61795=CARTESIAN_POINT('Ctrl Pts',(10.5152093525458,17.5845792171893,5.69732777215566));
#61796=CARTESIAN_POINT('Ctrl Pts',(10.5146501294348,17.5665197371488,5.75259648941308));
#61797=CARTESIAN_POINT('Ctrl Pts',(10.5071723447785,17.5310183201387,5.8578293481557));
#61798=CARTESIAN_POINT('Ctrl Pts',(10.5000174147823,17.5123838347761,5.91132323381311));
#61799=CARTESIAN_POINT('Ctrl Pts',(10.4763655908937,17.4753908390236,6.01347812322484));
#61800=CARTESIAN_POINT('Ctrl Pts',(10.4605419031702,17.4590326714753,6.05642735042512));
#61801=CARTESIAN_POINT('Ctrl Pts',(10.4319469960435,17.4387122071681,6.10705647468785));
#61802=CARTESIAN_POINT('Ctrl Pts',(10.4192298015583,17.4312562494153,6.12493725783482));
#61803=CARTESIAN_POINT('Ctrl Pts',(10.3949786188434,17.421409626235,6.14650298767116));
#61804=CARTESIAN_POINT('Ctrl Pts',(10.3846960006404,17.4180488377084,6.15331567799441));
#61805=CARTESIAN_POINT('Ctrl Pts',(10.3651744504234,17.4137258644339,6.16041901843185));
#61806=CARTESIAN_POINT('Ctrl Pts',(10.3566858346071,17.4124167774369,6.16189143600689));
#61807=CARTESIAN_POINT('Ctrl Pts',(10.3480326234796,17.4117050340792,6.16163338174817));
#61808=CARTESIAN_POINT('Origin',(10.3388776100546,20.0536826055992,6.51583646056242));
#61809=CARTESIAN_POINT('Origin',(1.05309141530195,21.2131190072776,6.89256018399713));
#61810=CARTESIAN_POINT('Origin',(1.63623295246351,20.0171393136753,0.));
#61811=CARTESIAN_POINT('',(1.90706327644678,17.7254928911647,0.453856447902045));
#61812=CARTESIAN_POINT('',(1.90706327644678,17.7254928911647,-0.453856447902046));
#61813=CARTESIAN_POINT('Ctrl Pts',(1.90706327644678,17.7254928911647,0.453856447902035));
#61814=CARTESIAN_POINT('Ctrl Pts',(1.90025953240075,17.7248979942003,0.453835022138424));
#61815=CARTESIAN_POINT('Ctrl Pts',(1.89355398287695,17.7243391729705,0.452743661072792));
#61816=CARTESIAN_POINT('Ctrl Pts',(1.87729436838401,17.7230467959918,0.447606881401318));
#61817=CARTESIAN_POINT('Ctrl Pts',(1.86835902888697,17.7223927114578,0.442546314019954));
#61818=CARTESIAN_POINT('Ctrl Pts',(1.84731494009718,17.7209473414004,0.426450928590348));
#61819=CARTESIAN_POINT('Ctrl Pts',(1.83623221810144,17.7202879485125,0.413449286575288));
#61820=CARTESIAN_POINT('Ctrl Pts',(1.81006546585384,17.7188609517424,0.375219786695204));
#61821=CARTESIAN_POINT('Ctrl Pts',(1.79484445174362,17.718225371305,0.34231373525627));
#61822=CARTESIAN_POINT('Ctrl Pts',(1.76839326635433,17.7173517778109,0.257598032754681));
#61823=CARTESIAN_POINT('Ctrl Pts',(1.75921616149678,17.7171803340553,0.210107900635043));
#61824=CARTESIAN_POINT('Ctrl Pts',(1.74822227890615,17.7169975657511,0.12619438804156));
#61825=CARTESIAN_POINT('Ctrl Pts',(1.74516474660346,17.716966780863,0.0869626247184948));
#61826=CARTESIAN_POINT('Ctrl Pts',(1.742515427654,17.7169388371718,0.0122397150279365));
#61827=CARTESIAN_POINT('Ctrl Pts',(1.74267268152351,17.7169400569674,-0.0243528511925373));
#61828=CARTESIAN_POINT('Ctrl Pts',(1.7460254704568,17.71697649914,-0.0996677434279772));
#61829=CARTESIAN_POINT('Ctrl Pts',(1.74954197522313,17.7170140039981,-0.139554220983467));
#61830=CARTESIAN_POINT('Ctrl Pts',(1.76185308853556,17.7172332241403,-0.224756276815653));
#61831=CARTESIAN_POINT('Ctrl Pts',(1.77207894319658,17.7174389665533,-0.273353606354512));
#61832=CARTESIAN_POINT('Ctrl Pts',(1.79824775577058,17.7183749061738,-0.348923678372305));
#61833=CARTESIAN_POINT('Ctrl Pts',(1.81321786098538,17.718986113044,-0.382374164872911));
#61834=CARTESIAN_POINT('Ctrl Pts',(1.84564815302469,17.7208443091635,-0.424859842185074));
#61835=CARTESIAN_POINT('Ctrl Pts',(1.85822154357173,17.7216651227597,-0.436125221547154));
#61836=CARTESIAN_POINT('Ctrl Pts',(1.87729261989272,17.7230568968889,-0.44720620221701));
#61837=CARTESIAN_POINT('Ctrl Pts',(1.88421421928262,17.7235877581235,-0.450152284724119));
#61838=CARTESIAN_POINT('Ctrl Pts',(1.89663970726115,17.7245977295641,-0.453190575607774));
#61839=CARTESIAN_POINT('Ctrl Pts',(1.90183077483582,17.7250353784623,-0.453839970159509));
#61840=CARTESIAN_POINT('Ctrl Pts',(1.90706327644678,17.7254928911647,-0.453856447902036));
#61841=CARTESIAN_POINT('',(1.62584114411962,20.0158633600508,2.35177984678802));
#61842=CARTESIAN_POINT('Origin',(1.62584114411962,20.0158633600508,-1.4400498308341E-16));
#61843=CARTESIAN_POINT('',(1.33846910697111,19.9805785106537,2.05196259868229));
#61844=CARTESIAN_POINT('Origin',(1.63623295246351,20.0171393136753,2.05196259868229));
#61845=CARTESIAN_POINT('Origin',(1.33846910697111,19.9805785106537,0.));
#61846=CARTESIAN_POINT('Origin',(1.62584114411962,20.0158633600508,-1.4400498308341E-16));
#61847=CARTESIAN_POINT('Origin',(5.83867335851287,20.5331341136527,0.));
#61848=CARTESIAN_POINT('',(10.3480326234796,18.4635649605383,0.479548822159048));
#61849=CARTESIAN_POINT('Ctrl Pts',(10.3480326234796,18.4635649605383,0.47954882215904));
#61850=CARTESIAN_POINT('Ctrl Pts',(7.55083071619378,18.2189729292873,0.47131116456692));
#61851=CARTESIAN_POINT('Ctrl Pts',(4.70971831191321,17.9705478141232,0.462682327280519));
#61852=CARTESIAN_POINT('Ctrl Pts',(1.90706327644678,17.7254928911647,0.453856447902026));
#61853=CARTESIAN_POINT('',(10.0307219562183,21.0478529600056,2.64748892284415));
#61854=CARTESIAN_POINT('Origin',(10.0307219562183,21.0478529600056,-1.62111941756958E-16));
#61855=CARTESIAN_POINT('',(10.3480326234796,18.4635649605383,-0.479548822159049));
#61856=CARTESIAN_POINT('Origin',(10.0307219562183,21.0478529600056,-1.62111941756958E-16));
#61857=CARTESIAN_POINT('Ctrl Pts',(1.90706327644678,17.7254928911647,-0.453856447902026));
#61858=CARTESIAN_POINT('Ctrl Pts',(4.70971830698341,17.9705478136921,-0.462682327264995));
#61859=CARTESIAN_POINT('Ctrl Pts',(7.55083071063942,18.2189729288016,-0.471311164550563));
#61860=CARTESIAN_POINT('Ctrl Pts',(10.3480326234796,18.4635649605383,-0.47954882215904));
#61861=CARTESIAN_POINT('Origin',(10.0411137645622,21.0491289136301,0.));
#61862=CARTESIAN_POINT('',(10.3388776100546,21.0856897166516,2.34767167473842));
#61863=CARTESIAN_POINT('Origin',(10.3388776100546,21.0856897166516,0.));
#61864=CARTESIAN_POINT('Origin',(10.0411137645622,21.0491289136301,2.34767167473842));
#61865=CARTESIAN_POINT('Ctrl Pts',(10.3480326234796,18.4635649605383,-0.479548822159038));
#61866=CARTESIAN_POINT('Ctrl Pts',(10.3515043799367,18.463868536752,-0.479559046355176));
#61867=CARTESIAN_POINT('Ctrl Pts',(10.3549842920161,18.4641804719486,-0.479275189924434));
#61868=CARTESIAN_POINT('Ctrl Pts',(10.3584662558372,18.4645002849058,-0.478693581607877));
#61869=CARTESIAN_POINT('Ctrl Pts',(10.3670410360545,18.4652878651219,-0.477261296913584));
#61870=CARTESIAN_POINT('Ctrl Pts',(10.3752404682198,18.46608779957,-0.474083787713369));
#61871=CARTESIAN_POINT('Ctrl Pts',(10.3939159291592,18.4679971841149,-0.463271309310389));
#61872=CARTESIAN_POINT('Ctrl Pts',(10.4037620790052,18.4690808995383,-0.454395207725884));
#61873=CARTESIAN_POINT('Ctrl Pts',(10.4301534297193,18.4721165427773,-0.424234118800134));
#61874=CARTESIAN_POINT('Ctrl Pts',(10.4436201527527,18.4738680701254,-0.398508891735425));
#61875=CARTESIAN_POINT('Ctrl Pts',(10.4707559634892,18.4775000338928,-0.337044819567072));
#61876=CARTESIAN_POINT('Ctrl Pts',(10.4855434672333,18.4797232784594,-0.285219862910056));
#61877=CARTESIAN_POINT('Ctrl Pts',(10.503063797412,18.4824794109906,-0.184213295767395));
#61878=CARTESIAN_POINT('Ctrl Pts',(10.5077954452097,18.4832622430944,-0.142902659146711));
#61879=CARTESIAN_POINT('Ctrl Pts',(10.5129524699051,18.4841201320625,-0.0690531837747526));
#61880=CARTESIAN_POINT('Ctrl Pts',(10.5141249106268,18.4843191140946,-0.0355299301020176));
#61881=CARTESIAN_POINT('Ctrl Pts',(10.5142094879025,18.4843333798549,0.0307774777112076));
#61882=CARTESIAN_POINT('Ctrl Pts',(10.5131850989077,18.4841592802621,0.0641628250530171));
#61883=CARTESIAN_POINT('Ctrl Pts',(10.5083046161227,18.4833464708957,0.137261078256563));
#61884=CARTESIAN_POINT('Ctrl Pts',(10.503879825914,18.4826118937437,0.17809920171751));
#61885=CARTESIAN_POINT('Ctrl Pts',(10.4867651973882,18.479909817102,0.28011633465925));
#61886=CARTESIAN_POINT('Ctrl Pts',(10.4718859508698,18.4776521193349,0.334420796175931));
#61887=CARTESIAN_POINT('Ctrl Pts',(10.4435576763645,18.4738593034485,0.398681362505303));
#61888=CARTESIAN_POINT('Ctrl Pts',(10.4292853290431,18.4719918118745,0.426411149600752));
#61889=CARTESIAN_POINT('Ctrl Pts',(10.4002072192657,18.4686862833898,0.457777203495697));
#61890=CARTESIAN_POINT('Ctrl Pts',(10.3895121106101,18.4675238404129,0.466757785235076));
#61891=CARTESIAN_POINT('Ctrl Pts',(10.3691517352141,18.4654920629651,0.476520858724271));
#61892=CARTESIAN_POINT('Ctrl Pts',(10.3605255868115,18.4646727052056,0.478994932552595));
#61893=CARTESIAN_POINT('Ctrl Pts',(10.350269709773,18.4637613669848,0.479524924856827));
#61894=CARTESIAN_POINT('Ctrl Pts',(10.3491503490814,18.4636626963416,0.479552113820167));
#61895=CARTESIAN_POINT('Ctrl Pts',(10.3480326234796,18.4635649605383,0.479548822159038));
#61896=CARTESIAN_POINT('Origin',(10.3388776100546,21.0856897166516,0.));
#61897=CARTESIAN_POINT('Origin',(1.05309141530195,22.3047932944232,0.));
#61898=CARTESIAN_POINT('Origin',(-0.307999999999999,0.,0.));
#61899=CARTESIAN_POINT('',(-0.507999999999999,-18.418471118769,-2.25561217007885E-15));
#61900=CARTESIAN_POINT('',(-0.307999999999999,-18.618471118769,-2.28010510606179E-15));
#61901=CARTESIAN_POINT('Origin',(-0.507999999999999,0.,0.));
#61902=CARTESIAN_POINT('Origin',(6.00065787119115,0.,0.));
#61903=CARTESIAN_POINT('',(6.00065787119115,-18.0894454950083,-2.21531815238124E-15));
#61904=CARTESIAN_POINT('',(6.00065787119115,-18.0894454950083,-2.21531815238124E-15));
#61905=CARTESIAN_POINT('Origin',(13.974,0.,0.));
#61906=CARTESIAN_POINT('',(14.224,-21.1856897166516,-2.59449870992264E-15));
#61907=CARTESIAN_POINT('Origin',(14.224,0.,0.));
#61908=CARTESIAN_POINT('',(13.974,-21.4356897166516,-2.62511487990132E-15));
#61909=CARTESIAN_POINT('Origin',(14.224,14.294,0.));
#61910=CARTESIAN_POINT('',(14.224,-14.294,-1.75051013470123E-15));
#61911=CARTESIAN_POINT('Origin',(14.224,0.,0.));
#61912=CARTESIAN_POINT('Origin',(13.824,0.,0.));
#61913=CARTESIAN_POINT('',(13.424,-13.494,-1.65253839076944E-15));
#61914=CARTESIAN_POINT('',(13.824,-13.894,-1.70152426273533E-15));
#61915=CARTESIAN_POINT('Origin',(13.424,0.,0.));
#61916=CARTESIAN_POINT('Origin',(6.758,0.,0.));
#61917=CARTESIAN_POINT('',(0.092000000000001,-13.494,-1.65253839076944E-15));
#61918=CARTESIAN_POINT('',(6.758,-13.494,-1.65253839076944E-15));
#61919=CARTESIAN_POINT('Origin',(0.0920000000000008,0.,0.));
#61920=CARTESIAN_POINT('Origin',(-0.207999999999999,0.,0.));
#61921=CARTESIAN_POINT('',(-0.508,-14.094,-1.72601719871828E-15));
#61922=CARTESIAN_POINT('',(-0.207999999999999,-13.794,-1.68927779474386E-15));
#61923=CARTESIAN_POINT('Origin',(-0.507999999999999,0.,0.));
#61924=CARTESIAN_POINT('Origin',(-0.507999999999999,18.418471118769,0.));
#61925=CARTESIAN_POINT('',(0.,0.,0.));
#61926=CARTESIAN_POINT('Origin',(2.3,8.,-13.));
#61927=CARTESIAN_POINT('',(2.2,-2.4,-12.9));
#61928=CARTESIAN_POINT('',(2.4,-2.4,-13.1));
#61929=CARTESIAN_POINT('',(1.7,-2.4,-12.4));
#61930=CARTESIAN_POINT('',(2.4,2.4,-13.1));
#61931=CARTESIAN_POINT('',(2.4,8.,-13.1));
#61932=CARTESIAN_POINT('',(2.2,2.4,-12.9));
#61933=CARTESIAN_POINT('',(1.9,2.4,-12.6));
#61934=CARTESIAN_POINT('',(2.2,8.,-12.9));
#61935=CARTESIAN_POINT('Origin',(0.,-2.4,-12.9));
#61936=CARTESIAN_POINT('',(0.2,-2.4,-12.9));
#61937=CARTESIAN_POINT('',(0.,-2.4,-12.9));
#61938=CARTESIAN_POINT('',(0.,-2.4,-13.1));
#61939=CARTESIAN_POINT('',(0.1,-2.4,-13.));
#61940=CARTESIAN_POINT('',(0.,-2.4,-13.3865604245452));
#61941=CARTESIAN_POINT('',(0.,-2.4,-12.9));
#61942=CARTESIAN_POINT('',(2.4,-2.4,-13.3865604245452));
#61943=CARTESIAN_POINT('',(1.2,-2.4,-13.3865604245452));
#61944=CARTESIAN_POINT('',(2.4,-2.4,-12.9));
#61945=CARTESIAN_POINT('Origin',(0.,2.4,-12.9));
#61946=CARTESIAN_POINT('',(0.2,2.4,-12.9));
#61947=CARTESIAN_POINT('',(0.,2.4,-12.9));
#61948=CARTESIAN_POINT('',(0.2,11.3,-12.9));
#61949=CARTESIAN_POINT('Origin',(0.1,11.3,-13.));
#61950=CARTESIAN_POINT('',(0.,2.4,-13.1));
#61951=CARTESIAN_POINT('',(-0.0999999999999996,2.4,-13.2));
#61952=CARTESIAN_POINT('',(0.,11.3,-13.1));
#61953=CARTESIAN_POINT('Origin',(0.,2.4,-13.7));
#61954=CARTESIAN_POINT('',(2.4,2.4,-13.3865604245452));
#61955=CARTESIAN_POINT('',(2.4,2.4,-13.7));
#61956=CARTESIAN_POINT('',(0.,2.4,-13.3865604245452));
#61957=CARTESIAN_POINT('',(1.2,2.4,-13.3865604245452));
#61958=CARTESIAN_POINT('',(0.,2.4,-13.7));
#61959=CARTESIAN_POINT('Origin',(2.4,13.6,0.));
#61960=CARTESIAN_POINT('',(2.4,-20.2,-2.47378653427765E-15));
#61961=CARTESIAN_POINT('Origin',(2.4,0.,0.));
#61962=CARTESIAN_POINT('Origin',(2.4,0.,0.));
#61963=CARTESIAN_POINT('Origin',(1.2,0.,0.));
#61964=CARTESIAN_POINT('Origin',(0.,0.,0.));
#61965=CARTESIAN_POINT('Origin',(0.,20.2,0.));
#61966=CARTESIAN_POINT('',(-1.2490009027033E-15,-20.2,-2.47378653427765E-15));
#61967=CARTESIAN_POINT('Origin',(0.,0.,0.));
#61968=CARTESIAN_POINT('Origin',(0.1,0.,0.));
#61969=CARTESIAN_POINT('',(0.199999999999999,-20.5,-2.51052593825207E-15));
#61970=CARTESIAN_POINT('Origin',(0.2,0.,0.));
#61971=CARTESIAN_POINT('',(0.1,-20.35,-2.49215623626486E-15));
#61972=CARTESIAN_POINT('Origin',(1.2,0.,0.));
#61973=CARTESIAN_POINT('',(2.2,-20.5,-2.51052593825207E-15));
#61974=CARTESIAN_POINT('Origin',(2.2,0.,0.));
#61975=CARTESIAN_POINT('',(1.2,-20.5,-2.51052593825207E-15));
#61976=CARTESIAN_POINT('Origin',(2.3,0.,0.));
#61977=CARTESIAN_POINT('',(2.3,-20.35,-2.49215623626486E-15));
#61978=CARTESIAN_POINT('',(0.,0.,0.));
#61979=CARTESIAN_POINT('Origin',(15.65,-6.08813972081441,0.455032679971239));
#61980=CARTESIAN_POINT('',(15.4,-17.6561953920765,7.4225278703698));
#61981=CARTESIAN_POINT('',(15.9,-16.7109201357914,6.29942267750568));
#61982=CARTESIAN_POINT('Ctrl Pts',(15.4,-17.6561953920765,7.4225278703698));
#61983=CARTESIAN_POINT('Ctrl Pts',(15.659421374204,-17.1714233605295,6.84309060700005));
#61984=CARTESIAN_POINT('Ctrl Pts',(15.9,-16.7109201357914,6.29942267750568));
#61985=CARTESIAN_POINT('',(15.9,-12.6466233749287,3.95289984855508));
#61986=CARTESIAN_POINT('',(15.9,-6.21313972081441,0.238526329025129));
#61987=CARTESIAN_POINT('',(15.6433901317022,-12.3389772513248,4.071587819396));
#61988=CARTESIAN_POINT('Ctrl Pts',(15.9000000000344,-12.6466233749697,3.95289984853906));
#61989=CARTESIAN_POINT('Ctrl Pts',(15.7706592115056,-12.4922823846733,4.01314090443486));
#61990=CARTESIAN_POINT('Ctrl Pts',(15.6433901317022,-12.3389772513248,4.071587819396));
#61991=CARTESIAN_POINT('',(15.4,-12.4774525214495,4.43257927994945));
#61992=CARTESIAN_POINT('',(14.6907281821669,-12.8809881912407,5.48455725744013));
#61993=CARTESIAN_POINT('',(15.4,-5.96313972081441,0.671539030917348));
#61994=CARTESIAN_POINT('Origin',(15.9,0.,0.));
#61995=CARTESIAN_POINT('',(15.9,-16.7109201357914,-6.29942267750567));
#61996=CARTESIAN_POINT('Origin',(15.9,0.,0.));
#61997=CARTESIAN_POINT('',(15.9,-12.6466233749287,-3.95289984855507));
#61998=CARTESIAN_POINT('',(15.9,-11.409292143521,-3.23852632902513));
#61999=CARTESIAN_POINT('Origin',(15.9,0.,0.));
#62000=CARTESIAN_POINT('Origin',(15.15,0.,0.));
#62001=CARTESIAN_POINT('',(15.3288252219091,-17.8169872981078,7.51536112060047));
#62002=CARTESIAN_POINT('Ctrl Pts',(15.4,-17.6561953920765,7.4225278703698));
#62003=CARTESIAN_POINT('Ctrl Pts',(15.3645856261785,-17.736206562841,7.46872234134886));
#62004=CARTESIAN_POINT('Ctrl Pts',(15.3288252219091,-17.8169872981078,7.51536112060047));
#62005=CARTESIAN_POINT('',(15.2106539453059,-18.25,7.26536112060047));
#62006=CARTESIAN_POINT('Ctrl Pts',(15.2106539453059,-18.25,7.26536112060047));
#62007=CARTESIAN_POINT('Ctrl Pts',(15.2709785585168,-18.031794847786,7.39134192396977));
#62008=CARTESIAN_POINT('Ctrl Pts',(15.3288252219091,-17.8169872981078,7.51536112060047));
#62009=CARTESIAN_POINT('',(15.2106539453093,-18.25,-7.26536112060046));
#62010=CARTESIAN_POINT('Ctrl Pts',(15.2106539453093,-18.25,-7.26536112060046));
#62011=CARTESIAN_POINT('Ctrl Pts',(16.2489053918282,-18.25,-2.42950104478723E-11));
#62012=CARTESIAN_POINT('Ctrl Pts',(15.2106539453059,-18.25,7.26536112060047));
#62013=CARTESIAN_POINT('',(15.3288252219121,-17.8169872981078,-7.51536112060046));
#62014=CARTESIAN_POINT('Ctrl Pts',(15.3288252219121,-17.8169872981078,-7.51536112060046));
#62015=CARTESIAN_POINT('Ctrl Pts',(15.2709785585222,-18.0317948477897,-7.39134192396767));
#62016=CARTESIAN_POINT('Ctrl Pts',(15.2106539453093,-18.25,-7.26536112060046));
#62017=CARTESIAN_POINT('',(15.4,-17.656195392083,-7.42252787037352));
#62018=CARTESIAN_POINT('Ctrl Pts',(15.3288252219121,-17.8169872981078,-7.51536112060046));
#62019=CARTESIAN_POINT('Ctrl Pts',(15.3645856261806,-17.7362065628429,-7.46872234134997));
#62020=CARTESIAN_POINT('Ctrl Pts',(15.4,-17.656195392083,-7.42252787037352));
#62021=CARTESIAN_POINT('Ctrl Pts',(15.9,-16.7109201357914,-6.29942267750567));
#62022=CARTESIAN_POINT('Ctrl Pts',(15.6594213742066,-17.1714233605351,-6.84309060700024));
#62023=CARTESIAN_POINT('Ctrl Pts',(15.4,-17.656195392083,-7.42252787037352));
#62024=CARTESIAN_POINT('Origin',(15.9,-10.7262794416288,3.42153903091735));
#62025=CARTESIAN_POINT('',(9.89139647084341,-12.4774525214495,4.43257927994945));
#62026=CARTESIAN_POINT('',(0.,-12.4774525214495,4.43257927994945));
#62027=CARTESIAN_POINT('',(9.9,-12.4850287992543,4.43695344597952));
#62028=CARTESIAN_POINT('Ctrl Pts',(9.89999999999984,-12.4850287992542,4.43695344597944));
#62029=CARTESIAN_POINT('Ctrl Pts',(9.89569679092782,-12.4812394300896,4.43476565267222));
#62030=CARTESIAN_POINT('Ctrl Pts',(9.89139647084332,-12.4774525214494,4.43257927994941));
#62031=CARTESIAN_POINT('',(9.9,-17.75,7.47668598600566));
#62032=CARTESIAN_POINT('',(9.9,-21.1185842870421,9.42153903091735));
#62033=CARTESIAN_POINT('',(9.83301270189222,-17.8169872981078,7.51536112060047));
#62034=CARTESIAN_POINT('',(12.8327618786655,-14.8172381213345,5.78345512588906));
#62035=CARTESIAN_POINT('',(7.95,-17.8169872981078,7.51536112060047));
#62036=CARTESIAN_POINT('Origin',(7.95,-18.0334936490539,7.39036112060047));
#62037=CARTESIAN_POINT('',(9.4,-18.25,7.26536112060047));
#62038=CARTESIAN_POINT('',(9.53701905283833,-18.1129809471617,7.34446910764079));
#62039=CARTESIAN_POINT('',(7.95,-18.25,7.26536112060047));
#62040=CARTESIAN_POINT('Origin',(7.95,-18.0334936490539,-7.39036112060046));
#62041=CARTESIAN_POINT('',(9.83301270189222,-17.8169872981078,-7.51536112060046));
#62042=CARTESIAN_POINT('',(7.95,-17.8169872981078,-7.51536112060046));
#62043=CARTESIAN_POINT('',(9.4,-18.25,-7.26536112060046));
#62044=CARTESIAN_POINT('',(7.95,-18.25,-7.26536112060046));
#62045=CARTESIAN_POINT('',(9.4,-18.25,-7.26536112060046));
#62046=CARTESIAN_POINT('Origin',(9.65,-18.,1.01832120635534));
#62047=CARTESIAN_POINT('',(9.4,-18.25,-10.0366424127107));
#62048=CARTESIAN_POINT('',(9.4,-18.25,1.01832120635534));
#62049=CARTESIAN_POINT('',(9.61650635094611,-18.0334936490539,-10.4116424127107));
#62050=CARTESIAN_POINT('',(6.68182667397366,-20.9681733260263,-5.32862810825457));
#62051=CARTESIAN_POINT('',(9.9,-17.75,-10.2479672781159));
#62052=CARTESIAN_POINT('',(11.1698262954046,-16.4801737045954,-9.51483272463993));
#62053=CARTESIAN_POINT('',(9.9,-17.75,-7.47668598600565));
#62054=CARTESIAN_POINT('',(9.9,-17.75,1.01832120635534));
#62055=CARTESIAN_POINT('',(11.1671033514046,-16.4828966485954,-6.74512352498115));
#62056=CARTESIAN_POINT('Origin',(15.9,-21.1185842870421,-9.42153903091734));
#62057=CARTESIAN_POINT('',(9.9,-12.4850287992543,-4.43695344597952));
#62058=CARTESIAN_POINT('',(9.9,-10.7262794416288,-3.42153903091735));
#62059=CARTESIAN_POINT('',(9.8913964708434,-12.4774525214495,-4.43257927994945));
#62060=CARTESIAN_POINT('Ctrl Pts',(9.89139647084313,-12.4774525214493,-4.43257927994931));
#62061=CARTESIAN_POINT('Ctrl Pts',(9.89569679092766,-12.4812394300895,-4.43476565267213));
#62062=CARTESIAN_POINT('Ctrl Pts',(9.89999999999972,-12.4850287992541,-4.43695344597938));
#62063=CARTESIAN_POINT('',(15.4,-12.4774525214495,-4.43257927994945));
#62064=CARTESIAN_POINT('',(0.,-12.4774525214495,-4.43257927994945));
#62065=CARTESIAN_POINT('',(15.4,-11.159292143521,-3.67153903091734));
#62066=CARTESIAN_POINT('Origin',(9.9,-14.7224318643355,-8.5));
#62067=CARTESIAN_POINT('',(9.9,-15.35,-11.633607924171));
#62068=CARTESIAN_POINT('',(9.9,-17.1181079660839,-10.6127903139961));
#62069=CARTESIAN_POINT('',(9.9,-10.0850287992543,-8.59387538414482));
#62070=CARTESIAN_POINT('',(9.9,-18.7185842870421,-13.5784609690826));
#62071=CARTESIAN_POINT('Origin',(9.9,0.,0.));
#62072=CARTESIAN_POINT('Origin',(9.65,-17.2431079660839,-10.8292966649422));
#62073=CARTESIAN_POINT('',(9.4,-17.8169872981078,-10.7866424127107));
#62074=CARTESIAN_POINT('',(9.83301270189222,-18.25,-10.0366424127107));
#62075=CARTESIAN_POINT('',(9.4,-15.4169872981078,-12.1722830587658));
#62076=CARTESIAN_POINT('',(9.4,-17.3681079660839,-11.0458030158883));
#62077=CARTESIAN_POINT('',(9.83301270189222,-15.4169872981078,-11.6722830587658));
#62078=CARTESIAN_POINT('',(9.83301270189222,-15.4169872981078,-11.6722830587658));
#62079=CARTESIAN_POINT('',(12.8327618786655,-12.4172381213345,-9.94037706405436));
#62080=CARTESIAN_POINT('Origin',(15.65,-11.284292143521,-3.45503267997124));
#62081=CARTESIAN_POINT('',(15.6433901317022,-12.3389772513248,-4.07158781939599));
#62082=CARTESIAN_POINT('Ctrl Pts',(15.6433901317022,-12.3389772513248,-4.07158781939599));
#62083=CARTESIAN_POINT('Ctrl Pts',(15.7706592115054,-12.4922823846731,-4.01314090443493));
#62084=CARTESIAN_POINT('Ctrl Pts',(15.9000000000344,-12.6466233749697,-3.95289984853905));
#62085=CARTESIAN_POINT('',(13.6398107279463,-13.4789009633564,-7.04325730755368));
#62086=CARTESIAN_POINT('Origin',(15.65,0.,0.));
#62087=CARTESIAN_POINT('',(15.4,-12.1991696110502,-3.70712298161641));
#62088=CARTESIAN_POINT('Ctrl Pts',(15.6433901273902,-12.3389772534808,-4.0715878156617));
#62089=CARTESIAN_POINT('Ctrl Pts',(15.5613792592266,-12.2925524049577,-3.95056278141904));
#62090=CARTESIAN_POINT('Ctrl Pts',(15.4801979882799,-12.2459386469402,-3.82904527862226));
#62091=CARTESIAN_POINT('Ctrl Pts',(15.4,-12.1991696110502,-3.70712298161641));
#62092=CARTESIAN_POINT('',(15.4,-12.1991696110502,3.70712298161641));
#62093=CARTESIAN_POINT('Origin',(15.4,0.,0.));
#62094=CARTESIAN_POINT('Ctrl Pts',(15.6433901273902,-12.3389772534808,4.0715878156617));
#62095=CARTESIAN_POINT('Ctrl Pts',(15.5613792592266,-12.2925524049577,3.95056278141906));
#62096=CARTESIAN_POINT('Ctrl Pts',(15.4801979882799,-12.2459386469402,3.82904527862227));
#62097=CARTESIAN_POINT('Ctrl Pts',(15.4,-12.1991696110502,3.70712298161641));
#62098=CARTESIAN_POINT('Origin',(0.,-18.0334936490539,10.4116424127107));
#62099=CARTESIAN_POINT('',(9.61650635094611,-18.0334936490539,10.4116424127107));
#62100=CARTESIAN_POINT('',(9.4,-17.8169872981078,10.7866424127107));
#62101=CARTESIAN_POINT('',(6.68182667397368,-15.0988139720814,15.4946567171668));
#62102=CARTESIAN_POINT('',(1.14709933354294,-17.8169872981078,10.7866424127107));
#62103=CARTESIAN_POINT('',(0.,-17.8169872981078,10.7866424127107));
#62104=CARTESIAN_POINT('',(1.14709933354217,-18.25,10.0366424127107));
#62105=CARTESIAN_POINT('Ctrl Pts',(1.14709933354294,-17.8169872981078,10.7866424127107));
#62106=CARTESIAN_POINT('Ctrl Pts',(1.14362113475313,-18.0334936490539,10.4116424127107));
#62107=CARTESIAN_POINT('Ctrl Pts',(1.14709933354217,-18.25,10.0366424127107));
#62108=CARTESIAN_POINT('',(9.4,-18.25,10.0366424127107));
#62109=CARTESIAN_POINT('',(0.,-18.25,10.0366424127107));
#62110=CARTESIAN_POINT('',(8.50682667397365,-19.1431733260264,8.48962083206777));
#62111=CARTESIAN_POINT('Origin',(0.,1.29036654044864E-15,21.0732848254213));
#62112=CARTESIAN_POINT('',(9.4,-15.4169872981078,12.1722830587658));
#62113=CARTESIAN_POINT('',(9.4,-8.24310796608386,16.3141242222437));
#62114=CARTESIAN_POINT('',(15.2106539453093,-15.4169872981078,12.1722830587658));
#62115=CARTESIAN_POINT('',(7.95,-15.4169872981078,12.1722830587658));
#62116=CARTESIAN_POINT('',(15.2106539453059,-2.83301270189222,19.4376441793662));
#62117=CARTESIAN_POINT('Ctrl Pts',(15.2106539453093,-15.4169872981078,12.1722830587658));
#62118=CARTESIAN_POINT('Ctrl Pts',(16.2489053918282,-9.12500000002104,15.8049636190539));
#62119=CARTESIAN_POINT('Ctrl Pts',(15.2106539453059,-2.83301270189222,19.4376441793663));
#62120=CARTESIAN_POINT('',(9.4,-2.83301270189222,19.4376441793662));
#62121=CARTESIAN_POINT('',(3.975,-2.83301270189222,19.4376441793662));
#62122=CARTESIAN_POINT('',(9.4,-0.433012701892218,20.8232848254213));
#62123=CARTESIAN_POINT('',(9.4,-0.881892033916136,20.5641242222437));
#62124=CARTESIAN_POINT('',(1.14709933354217,-0.433012701892219,20.8232848254213));
#62125=CARTESIAN_POINT('',(0.,-0.433012701892218,20.8232848254213));
#62126=CARTESIAN_POINT('Ctrl Pts',(1.14709933354217,-0.433012701892218,
20.8232848254213));
#62127=CARTESIAN_POINT('Ctrl Pts',(-0.721559551129004,-9.12499999996429,
15.8049636190866));
#62128=CARTESIAN_POINT('Ctrl Pts',(1.14709933354294,-17.8169872981078,10.7866424127107));
#62129=CARTESIAN_POINT('Origin',(9.65,-8.11810796608386,16.0976178712976));
#62130=CARTESIAN_POINT('',(9.9,-17.75,10.2479672781159));
#62131=CARTESIAN_POINT('',(9.9,-17.75,10.2479672781159));
#62132=CARTESIAN_POINT('',(9.9,-15.35,11.633607924171));
#62133=CARTESIAN_POINT('',(9.9,-7.99310796608386,15.8811115203515));
#62134=CARTESIAN_POINT('',(9.83301270189222,-15.4169872981078,11.6722830587658));
#62135=CARTESIAN_POINT('',(11.1671033514046,-14.0828966485954,10.9020454631465));
#62136=CARTESIAN_POINT('',(9.4,-15.4169872981078,12.1722830587658));
#62137=CARTESIAN_POINT('Origin',(9.65,-18.,9.51832120635533));
#62138=CARTESIAN_POINT('',(9.4,-18.25,9.51832120635533));
#62139=CARTESIAN_POINT('',(9.9,-17.75,9.51832120635533));
#62140=CARTESIAN_POINT('Origin',(15.65,-3.43813972081441,-5.04496732002876));
#62141=CARTESIAN_POINT('',(15.4,-15.2561953920766,-11.5794498085352));
#62142=CARTESIAN_POINT('',(15.9,-13.8109201357914,-11.3223700194554));
#62143=CARTESIAN_POINT('Ctrl Pts',(15.4,-15.2561953920766,-11.5794498085352));
#62144=CARTESIAN_POINT('Ctrl Pts',(15.659421374204,-14.5120019863256,-11.4493435458561));
#62145=CARTESIAN_POINT('Ctrl Pts',(15.9,-13.8109201357914,-11.3223700194554));
#62146=CARTESIAN_POINT('',(15.9,-9.74662337492871,-8.97584719050482));
#62147=CARTESIAN_POINT('',(15.9,-3.31313972081441,-5.26147367097487));
#62148=CARTESIAN_POINT('',(15.6433901317022,-9.6955871109986,-8.65007384666752));
#62149=CARTESIAN_POINT('Ctrl Pts',(15.9000000000343,-9.74662337493534,-8.97584719054823));
#62150=CARTESIAN_POINT('Ctrl Pts',(15.7706592115056,-9.72162316454368,-8.81206344415842));
#62151=CARTESIAN_POINT('Ctrl Pts',(15.6433901317022,-9.6955871109986,-8.65007384666752));
#62152=CARTESIAN_POINT('',(15.4,-10.0774525214495,-8.58950121811475));
#62153=CARTESIAN_POINT('',(14.6907281821669,-11.1902600090738,-8.41298437074177));
#62154=CARTESIAN_POINT('',(15.4,-3.56313972081441,-4.82846096908265));
#62155=CARTESIAN_POINT('Origin',(15.65,0.,0.));
#62156=CARTESIAN_POINT('',(15.9,-2.9,-12.9287470390599));
#62157=CARTESIAN_POINT('Origin',(15.9,0.,0.));
#62158=CARTESIAN_POINT('',(15.6433901317022,-2.64339014032616,-12.7216616660635));
#62159=CARTESIAN_POINT('Ctrl Pts',(15.6433901317022,-2.64339014032616,-12.7216616660635));
#62160=CARTESIAN_POINT('Ctrl Pts',(15.7706592115055,-2.77065922012951,-12.8252043485933));
#62161=CARTESIAN_POINT('Ctrl Pts',(15.9000000000343,-2.90000000003428,-12.9287470390873));
#62162=CARTESIAN_POINT('',(15.4,-2.88912212849219,-12.4183522790528));
#62163=CARTESIAN_POINT('Ctrl Pts',(15.6433901273902,-2.64339014463815,-12.7216616660635));
#62164=CARTESIAN_POINT('Ctrl Pts',(15.5613792592266,-2.72498847452463,-12.6209440507544));
#62165=CARTESIAN_POINT('Ctrl Pts',(15.4801979882799,-2.80691883994237,-12.519816600747));
#62166=CARTESIAN_POINT('Ctrl Pts',(15.4,-2.88912212849219,-12.4183522790528));
#62167=CARTESIAN_POINT('',(15.4,-9.31004748255804,-8.71122929743642));
#62168=CARTESIAN_POINT('Origin',(15.4,0.,0.));
#62169=CARTESIAN_POINT('Ctrl Pts',(15.4,-9.31004748255804,-8.71122929743642));
#62170=CARTESIAN_POINT('Ctrl Pts',(15.4801979882799,-9.43901980699785,-8.69077132212473));
#62171=CARTESIAN_POINT('Ctrl Pts',(15.5613792592266,-9.56756393043304,-8.67038126933532));
#62172=CARTESIAN_POINT('Ctrl Pts',(15.6433901273902,-9.6955871088426,-8.65007385040182));
#62173=CARTESIAN_POINT('Origin',(15.9,0.,0.));
#62174=CARTESIAN_POINT('',(15.9,-2.9,-17.6217926969611));
#62175=CARTESIAN_POINT('Origin',(15.9,0.,0.));
#62176=CARTESIAN_POINT('',(15.9,-2.9,-11.5));
#62177=CARTESIAN_POINT('Origin',(15.15,0.,0.));
#62178=CARTESIAN_POINT('',(15.3288252219092,-15.4169872981078,-11.6722830587658));
#62179=CARTESIAN_POINT('Ctrl Pts',(15.4,-15.2561953920766,-11.5794498085352));
#62180=CARTESIAN_POINT('Ctrl Pts',(15.3645856261792,-15.3362065628395,-11.6256442795133));
#62181=CARTESIAN_POINT('Ctrl Pts',(15.3288252219092,-15.4169872981078,-11.6722830587658));
#62182=CARTESIAN_POINT('',(15.2106539453059,-15.4169872981078,-12.1722830587658));
#62183=CARTESIAN_POINT('Ctrl Pts',(15.2106539453059,-15.4169872981078,-12.1722830587658));
#62184=CARTESIAN_POINT('Ctrl Pts',(15.2709785585169,-15.4169872981078,-11.9203214520272));
#62185=CARTESIAN_POINT('Ctrl Pts',(15.3288252219092,-15.4169872981078,-11.6722830587658));
#62186=CARTESIAN_POINT('',(15.2106539453093,-2.83301270189222,-19.4376441793662));
#62187=CARTESIAN_POINT('Ctrl Pts',(15.2106539453093,-2.83301270189223,-19.4376441793662));
#62188=CARTESIAN_POINT('Ctrl Pts',(16.2489053918282,-9.12499999997897,-15.8049636190782));
#62189=CARTESIAN_POINT('Ctrl Pts',(15.2106539453059,-15.4169872981078,-12.1722830587658));
#62190=CARTESIAN_POINT('',(15.3288252219121,-2.4,-19.1876441793662));
#62191=CARTESIAN_POINT('Ctrl Pts',(15.3288252219121,-2.4,-19.1876441793662));
#62192=CARTESIAN_POINT('Ctrl Pts',(15.2709785585222,-2.61480754968187,-19.311663375999));
#62193=CARTESIAN_POINT('Ctrl Pts',(15.2106539453093,-2.83301270189222,-19.4376441793662));
#62194=CARTESIAN_POINT('',(15.4,-2.4,-19.0019776789123));
#62195=CARTESIAN_POINT('Ctrl Pts',(15.3288252219121,-2.4,-19.1876441793662));
#62196=CARTESIAN_POINT('Ctrl Pts',(15.3645856261801,-2.4,-19.0943666208664));
#62197=CARTESIAN_POINT('Ctrl Pts',(15.4,-2.4,-19.0019776789123));
#62198=CARTESIAN_POINT('Ctrl Pts',(15.9,-2.9,-17.6217926969611));
#62199=CARTESIAN_POINT('Ctrl Pts',(15.6594213742066,-2.65942137420663,-18.292434152861));
#62200=CARTESIAN_POINT('Ctrl Pts',(15.4,-2.4,-19.0019776789123));
#62201=CARTESIAN_POINT('Origin',(7.95,-15.4169872981078,-11.9222830587658));
#62202=CARTESIAN_POINT('',(7.95,-15.4169872981078,-12.1722830587658));
#62203=CARTESIAN_POINT('',(7.95,-15.4169872981078,-11.6722830587658));
#62204=CARTESIAN_POINT('Origin',(0.,-18.0334936490539,-10.4116424127107));
#62205=CARTESIAN_POINT('',(1.14709933354294,-18.25,-10.0366424127107));
#62206=CARTESIAN_POINT('',(0.,-18.25,-10.0366424127107));
#62207=CARTESIAN_POINT('',(1.14709933354217,-17.8169872981078,-10.7866424127107));
#62208=CARTESIAN_POINT('Ctrl Pts',(1.14709933354294,-18.25,-10.0366424127107));
#62209=CARTESIAN_POINT('Ctrl Pts',(1.14362113475313,-18.0334936490539,-10.4116424127107));
#62210=CARTESIAN_POINT('Ctrl Pts',(1.14709933354217,-17.8169872981078,-10.7866424127107));
#62211=CARTESIAN_POINT('',(0.,-17.8169872981078,-10.7866424127107));
#62212=CARTESIAN_POINT('Origin',(0.,-18.25,-10.5366424127107));
#62213=CARTESIAN_POINT('',(1.14709933354294,-0.433012701892223,-20.8232848254213));
#62214=CARTESIAN_POINT('Ctrl Pts',(1.14709933354217,-17.8169872981078,-10.7866424127107));
#62215=CARTESIAN_POINT('Ctrl Pts',(-0.721559551129003,-9.12500000003573,
-15.8049636190454));
#62216=CARTESIAN_POINT('Ctrl Pts',(1.14709933354294,-0.433012701892223,
-20.8232848254213));
#62217=CARTESIAN_POINT('',(9.4,-0.433012701892223,-20.8232848254213));
#62218=CARTESIAN_POINT('',(0.,-0.433012701892223,-20.8232848254213));
#62219=CARTESIAN_POINT('',(9.4,-2.83301270189222,-19.4376441793662));
#62220=CARTESIAN_POINT('',(9.4,-10.0068920339161,-15.2958030158883));
#62221=CARTESIAN_POINT('',(7.95,-2.83301270189222,-19.4376441793662));
#62222=CARTESIAN_POINT('Origin',(0.75,0.,0.));
#62223=CARTESIAN_POINT('',(0.,-17.8588235294118,2.18707510718316E-15));
#62224=CARTESIAN_POINT('Origin',(0.,0.,0.));
#62225=CARTESIAN_POINT('',(0.151136363625822,-18.25,-5.64802764011468E-15));
#62226=CARTESIAN_POINT('',(0.75,-19.8,-2.42480066231176E-15));
#62227=CARTESIAN_POINT('Ctrl Pts',(1.14709933354217,-18.25,10.0366424127107));
#62228=CARTESIAN_POINT('Ctrl Pts',(0.15113636362346,-18.25,4.68728503810705));
#62229=CARTESIAN_POINT('Ctrl Pts',(0.151136363625822,-18.25,-9.06107487178543E-15));
#62230=CARTESIAN_POINT('',(1.14709933354294,0.433012701892216,20.8232848254213));
#62231=CARTESIAN_POINT('Ctrl Pts',(1.14709933354294,0.433012701892216,20.8232848254213));
#62232=CARTESIAN_POINT('Ctrl Pts',(1.14362113475313,-8.04911692853238E-15,
20.8232848254213));
#62233=CARTESIAN_POINT('Ctrl Pts',(1.14709933354217,-0.433012701892219,
20.8232848254213));
#62234=CARTESIAN_POINT('',(1.14709933354217,17.8169872981078,10.7866424127107));
#62235=CARTESIAN_POINT('Ctrl Pts',(1.14709933354217,17.8169872981078,10.7866424127107));
#62236=CARTESIAN_POINT('Ctrl Pts',(-0.721559551129003,9.12500000003573,
15.8049636190454));
#62237=CARTESIAN_POINT('Ctrl Pts',(1.14709933354294,0.433012701892217,20.8232848254213));
#62238=CARTESIAN_POINT('',(1.14709933354294,18.25,10.0366424127107));
#62239=CARTESIAN_POINT('Ctrl Pts',(1.14709933354294,18.25,10.0366424127107));
#62240=CARTESIAN_POINT('Ctrl Pts',(1.14362113475313,18.0334936490539,10.4116424127107));
#62241=CARTESIAN_POINT('Ctrl Pts',(1.14709933354217,17.8169872981078,10.7866424127107));
#62242=CARTESIAN_POINT('',(1.14709933354217,18.25,-10.0366424127107));
#62243=CARTESIAN_POINT('Ctrl Pts',(1.14709933354217,18.25,-10.0366424127107));
#62244=CARTESIAN_POINT('Ctrl Pts',(-0.721559551129004,18.25,-4.12425649187753E-11));
#62245=CARTESIAN_POINT('Ctrl Pts',(1.14709933354294,18.25,10.0366424127107));
#62246=CARTESIAN_POINT('',(1.14709933354294,17.8169872981078,-10.7866424127107));
#62247=CARTESIAN_POINT('Ctrl Pts',(1.14709933354294,17.8169872981078,-10.7866424127107));
#62248=CARTESIAN_POINT('Ctrl Pts',(1.14362113475313,18.0334936490539,-10.4116424127107));
#62249=CARTESIAN_POINT('Ctrl Pts',(1.14709933354217,18.25,-10.0366424127107));
#62250=CARTESIAN_POINT('',(1.14709933354217,0.433012701892212,-20.8232848254213));
#62251=CARTESIAN_POINT('Ctrl Pts',(1.14709933354217,0.433012701892213,-20.8232848254213));
#62252=CARTESIAN_POINT('Ctrl Pts',(-0.721559551129003,9.12499999996428,
-15.8049636190866));
#62253=CARTESIAN_POINT('Ctrl Pts',(1.14709933354294,17.8169872981078,-10.7866424127107));
#62254=CARTESIAN_POINT('Ctrl Pts',(1.14709933354294,-0.433012701892223,
-20.8232848254213));
#62255=CARTESIAN_POINT('Ctrl Pts',(1.14362113475313,1.66533453693773E-15,
-20.8232848254213));
#62256=CARTESIAN_POINT('Ctrl Pts',(1.14709933354217,0.433012701892212,-20.8232848254213));
#62257=CARTESIAN_POINT('Ctrl Pts',(0.151136363625822,-18.25,-9.06107487178543E-15));
#62258=CARTESIAN_POINT('Ctrl Pts',(0.151136363628184,-18.25,-4.68728503808653));
#62259=CARTESIAN_POINT('Ctrl Pts',(1.14709933354294,-18.25,-10.0366424127107));
#62260=CARTESIAN_POINT('Origin',(15.65,2.65,-5.5));
#62261=CARTESIAN_POINT('',(15.4,2.4,-19.0019776789049));
#62262=CARTESIAN_POINT('',(15.9,2.9,-17.6217926969611));
#62263=CARTESIAN_POINT('Ctrl Pts',(15.4,2.4,-19.0019776789049));
#62264=CARTESIAN_POINT('Ctrl Pts',(15.6594213742041,2.65942137420405,-18.2924341528561));
#62265=CARTESIAN_POINT('Ctrl Pts',(15.9,2.9,-17.6217926969611));
#62266=CARTESIAN_POINT('',(15.9,2.9,-12.9287470390599));
#62267=CARTESIAN_POINT('',(15.9,2.9,-5.5));
#62268=CARTESIAN_POINT('',(15.6433901317022,2.64339014032616,-12.7216616660635));
#62269=CARTESIAN_POINT('Ctrl Pts',(15.9000000000343,2.90000000003429,-12.9287470390873));
#62270=CARTESIAN_POINT('Ctrl Pts',(15.7706592115055,2.77065922012948,-12.8252043485932));
#62271=CARTESIAN_POINT('Ctrl Pts',(15.6433901317022,2.64339014032616,-12.7216616660635));
#62272=CARTESIAN_POINT('',(15.4,2.4,-13.0220804980642));
#62273=CARTESIAN_POINT('',(14.6907281821669,1.6907281821669,-13.8975416281819));
#62274=CARTESIAN_POINT('',(15.4,2.4,-5.5));
#62275=CARTESIAN_POINT('Origin',(15.9,0.,0.));
#62276=CARTESIAN_POINT('',(15.9,13.8109201357914,-11.3223700194554));
#62277=CARTESIAN_POINT('Origin',(15.9,0.,0.));
#62278=CARTESIAN_POINT('',(15.9,9.74662337492871,-8.97584719050482));
#62279=CARTESIAN_POINT('',(15.9,8.50929214352104,-8.26147367097488));
#62280=CARTESIAN_POINT('Origin',(15.9,0.,0.));
#62281=CARTESIAN_POINT('Origin',(15.15,0.,0.));
#62282=CARTESIAN_POINT('',(15.3288252219091,2.4,-19.1876441793662));
#62283=CARTESIAN_POINT('Ctrl Pts',(15.4,2.4,-19.0019776789049));
#62284=CARTESIAN_POINT('Ctrl Pts',(15.3645856261785,2.4,-19.094366620863));
#62285=CARTESIAN_POINT('Ctrl Pts',(15.3288252219091,2.4,-19.1876441793662));
#62286=CARTESIAN_POINT('',(15.2106539453059,2.83301270189221,-19.4376441793662));
#62287=CARTESIAN_POINT('Ctrl Pts',(15.2106539453059,2.83301270189221,-19.4376441793662));
#62288=CARTESIAN_POINT('Ctrl Pts',(15.2709785585168,2.61480754967825,-19.3116633759969));
#62289=CARTESIAN_POINT('Ctrl Pts',(15.3288252219091,2.4,-19.1876441793662));
#62290=CARTESIAN_POINT('',(15.2106539453093,15.4169872981078,-12.1722830587658));
#62291=CARTESIAN_POINT('Ctrl Pts',(15.2106539453093,15.4169872981078,-12.1722830587658));
#62292=CARTESIAN_POINT('Ctrl Pts',(16.2489053918282,9.12500000002104,-15.8049636190539));
#62293=CARTESIAN_POINT('Ctrl Pts',(15.2106539453059,2.83301270189221,-19.4376441793662));
#62294=CARTESIAN_POINT('',(15.3288252219121,15.4169872981078,-11.6722830587658));
#62295=CARTESIAN_POINT('Ctrl Pts',(15.3288252219121,15.4169872981078,-11.6722830587658));
#62296=CARTESIAN_POINT('Ctrl Pts',(15.2709785585222,15.4169872981078,-11.9203214520314));
#62297=CARTESIAN_POINT('Ctrl Pts',(15.2106539453093,15.4169872981078,-12.1722830587658));
#62298=CARTESIAN_POINT('',(15.4,15.256195392083,-11.5794498085389));
#62299=CARTESIAN_POINT('Ctrl Pts',(15.3288252219121,15.4169872981078,-11.6722830587658));
#62300=CARTESIAN_POINT('Ctrl Pts',(15.3645856261809,15.3362065628422,-11.6256442795149));
#62301=CARTESIAN_POINT('Ctrl Pts',(15.4,15.256195392083,-11.5794498085389));
#62302=CARTESIAN_POINT('Ctrl Pts',(15.9,13.8109201357914,-11.3223700194554));
#62303=CARTESIAN_POINT('Ctrl Pts',(15.6594213742065,14.5120019863289,-11.4493435458609));
#62304=CARTESIAN_POINT('Ctrl Pts',(15.4,15.256195392083,-11.5794498085389));
#62305=CARTESIAN_POINT('Origin',(15.9,2.4,-11.));
#62306=CARTESIAN_POINT('',(9.89139647084341,2.4,-13.0220804980642));
#62307=CARTESIAN_POINT('',(0.,2.4,-13.0220804980642));
#62308=CARTESIAN_POINT('',(9.9,2.4,-13.0308288301244));
#62309=CARTESIAN_POINT('Ctrl Pts',(9.89999999999984,2.4,-13.0308288301242));
#62310=CARTESIAN_POINT('Ctrl Pts',(9.89569679092782,2.4,-13.0264532435097));
#62311=CARTESIAN_POINT('Ctrl Pts',(9.89139647084332,2.4,-13.0220804980641));
#62312=CARTESIAN_POINT('',(9.9,2.4,-19.1102939101766));
#62313=CARTESIAN_POINT('',(9.9,2.4,-23.));
#62314=CARTESIAN_POINT('',(9.83301270189222,2.4,-19.1876441793662));
#62315=CARTESIAN_POINT('',(12.8327618786655,2.4,-15.7238321899434));
#62316=CARTESIAN_POINT('',(7.95,2.4,-19.1876441793662));
#62317=CARTESIAN_POINT('Origin',(7.95,2.61650635094611,-19.3126441793662));
#62318=CARTESIAN_POINT('',(9.4,2.83301270189222,-19.4376441793662));
#62319=CARTESIAN_POINT('',(7.95,2.83301270189222,-19.4376441793662));
#62320=CARTESIAN_POINT('',(9.83301270189222,2.4,-19.1876441793662));
#62321=CARTESIAN_POINT('Origin',(9.9,-1.66533453693773E-15,-20.4959345562317));
#62322=CARTESIAN_POINT('',(9.4,0.433012701892213,-20.8232848254213));
#62323=CARTESIAN_POINT('',(9.4,0.433012701892213,-20.8232848254213));
#62324=CARTESIAN_POINT('',(9.9,2.22044604925031E-15,-20.4959345562317));
#62325=CARTESIAN_POINT('',(9.9,-1.66533453693773E-15,-20.4959345562317));
#62326=CARTESIAN_POINT('',(9.4,-0.43301270189222,-20.8232848254213));
#62327=CARTESIAN_POINT('Origin',(9.65,0.756892033916132,-20.3476178712976));
#62328=CARTESIAN_POINT('',(9.9,0.631892033916133,-20.1311115203515));
#62329=CARTESIAN_POINT('',(9.4,0.881892033916132,-20.5641242222437));
#62330=CARTESIAN_POINT('Origin',(7.95,-2.61650635094611,-19.3126441793662));
#62331=CARTESIAN_POINT('',(9.83301270189222,-2.4,-19.1876441793662));
#62332=CARTESIAN_POINT('',(7.95,-2.4,-19.1876441793662));
#62333=CARTESIAN_POINT('',(9.4,-2.83301270189222,-19.4376441793662));
#62334=CARTESIAN_POINT('Origin',(9.65,-9.88189203391614,-15.0792966649422));
#62335=CARTESIAN_POINT('',(9.9,-2.4,-19.1102939101766));
#62336=CARTESIAN_POINT('',(9.9,-9.75689203391614,-14.8627903139961));
#62337=CARTESIAN_POINT('',(11.1671033514046,-2.4,-17.6471689881276));
#62338=CARTESIAN_POINT('Origin',(0.,-5.30825383648903E-15,-20.8232848254213));
#62339=CARTESIAN_POINT('',(0.,0.433012701892213,-20.8232848254213));
#62340=CARTESIAN_POINT('Origin',(0.,-3.87109962134591E-15,-21.0732848254213));
#62341=CARTESIAN_POINT('',(9.4,17.8169872981078,-10.7866424127107));
#62342=CARTESIAN_POINT('',(0.,17.8169872981078,-10.7866424127107));
#62343=CARTESIAN_POINT('',(9.4,15.4169872981078,-12.1722830587658));
#62344=CARTESIAN_POINT('',(9.4,8.24310796608386,-16.3141242222437));
#62345=CARTESIAN_POINT('',(7.95,15.4169872981078,-12.1722830587658));
#62346=CARTESIAN_POINT('Origin',(15.65,-2.65,-11.5));
#62347=CARTESIAN_POINT('',(15.4,-2.4,-13.0220804980642));
#62348=CARTESIAN_POINT('',(15.4,-2.4,-11.5));
#62349=CARTESIAN_POINT('',(13.6398107279464,-0.639810727946355,-15.1946993031381));
#62350=CARTESIAN_POINT('Origin',(7.95,15.4169872981078,-11.9222830587658));
#62351=CARTESIAN_POINT('',(9.83301270189222,15.4169872981078,-11.6722830587658));
#62352=CARTESIAN_POINT('',(7.95,15.4169872981078,-11.6722830587658));
#62353=CARTESIAN_POINT('',(9.4,15.4169872981078,-12.1722830587658));
#62354=CARTESIAN_POINT('Origin',(9.65,8.11810796608386,-16.0976178712976));
#62355=CARTESIAN_POINT('',(9.61650635094611,18.0334936490539,-10.4116424127107));
#62356=CARTESIAN_POINT('',(6.68182667397365,15.0988139720815,-15.4946567171668));
#62357=CARTESIAN_POINT('',(9.9,17.75,-10.2479672781159));
#62358=CARTESIAN_POINT('',(11.1698262954046,16.4801737045954,-9.51483272463995));
#62359=CARTESIAN_POINT('',(9.9,15.35,-11.633607924171));
#62360=CARTESIAN_POINT('',(9.9,7.99310796608386,-15.8811115203515));
#62361=CARTESIAN_POINT('',(11.1671033514046,14.0828966485954,-10.9020454631465));
#62362=CARTESIAN_POINT('Origin',(15.9,18.7185842870421,-13.5784609690827));
#62363=CARTESIAN_POINT('',(9.9,10.0850287992543,-8.59387538414483));
#62364=CARTESIAN_POINT('',(9.9,8.32627944162882,-7.57846096908266));
#62365=CARTESIAN_POINT('',(9.89139647084341,10.0774525214495,-8.58950121811476));
#62366=CARTESIAN_POINT('Ctrl Pts',(9.89139647084313,10.0774525214493,-8.58950121811462));
#62367=CARTESIAN_POINT('Ctrl Pts',(9.89569679092767,10.0812394300895,-8.59168759083745));
#62368=CARTESIAN_POINT('Ctrl Pts',(9.89999999999973,10.0850287992541,-8.59387538414469));
#62369=CARTESIAN_POINT('',(15.4,10.0774525214495,-8.58950121811476));
#62370=CARTESIAN_POINT('',(0.,10.0774525214495,-8.58950121811476));
#62371=CARTESIAN_POINT('',(15.4,8.75929214352104,-7.82846096908266));
#62372=CARTESIAN_POINT('Origin',(9.9,14.7224318643355,-8.50000000000001));
#62373=CARTESIAN_POINT('',(9.9,17.75,-7.47668598600567));
#62374=CARTESIAN_POINT('',(9.9,17.75,-9.51832120635534));
#62375=CARTESIAN_POINT('',(9.9,12.4850287992543,-4.43695344597953));
#62376=CARTESIAN_POINT('',(9.9,21.1185842870421,-9.42153903091736));
#62377=CARTESIAN_POINT('Origin',(9.9,0.,0.));
#62378=CARTESIAN_POINT('Origin',(9.65,18.,-9.51832120635534));
#62379=CARTESIAN_POINT('',(9.4,18.25,-10.0366424127107));
#62380=CARTESIAN_POINT('',(9.83301270189222,17.8169872981078,-10.7866424127107));
#62381=CARTESIAN_POINT('',(9.4,18.25,-7.26536112060048));
#62382=CARTESIAN_POINT('',(9.4,18.25,-9.51832120635534));
#62383=CARTESIAN_POINT('',(9.83301270189222,17.8169872981078,-7.51536112060048));
#62384=CARTESIAN_POINT('',(9.83301270189222,17.8169872981078,-7.51536112060048));
#62385=CARTESIAN_POINT('',(12.8327618786655,14.8172381213345,-5.78345512588907));
#62386=CARTESIAN_POINT('Origin',(15.65,8.63429214352104,-8.04496732002877));
#62387=CARTESIAN_POINT('',(15.6433901317022,9.69558711099859,-8.65007384666753));
#62388=CARTESIAN_POINT('Ctrl Pts',(15.6433901317022,9.69558711099859,-8.65007384666753));
#62389=CARTESIAN_POINT('Ctrl Pts',(15.7706592115056,9.72162316454367,-8.81206344415844));
#62390=CARTESIAN_POINT('Ctrl Pts',(15.9000000000343,9.74662337493534,-8.97584719054825));
#62391=CARTESIAN_POINT('',(13.6398107279463,12.8390902354101,-8.15144199558439));
#62392=CARTESIAN_POINT('Origin',(15.65,0.,0.));
#62393=CARTESIAN_POINT('',(15.4,9.31004748255804,-8.71122929743643));
#62394=CARTESIAN_POINT('Ctrl Pts',(15.6433901273902,9.69558710884259,-8.65007385040183));
#62395=CARTESIAN_POINT('Ctrl Pts',(15.5613792592266,9.56756393043305,-8.67038126933533));
#62396=CARTESIAN_POINT('Ctrl Pts',(15.4801979882799,9.43901980699784,-8.69077132212474));
#62397=CARTESIAN_POINT('Ctrl Pts',(15.4,9.31004748255804,-8.71122929743643));
#62398=CARTESIAN_POINT('',(15.4,2.88912212849219,-12.4183522790528));
#62399=CARTESIAN_POINT('Origin',(15.4,0.,0.));
#62400=CARTESIAN_POINT('Ctrl Pts',(15.6433901273902,2.64339014463815,-12.7216616660635));
#62401=CARTESIAN_POINT('Ctrl Pts',(15.5613792592266,2.72498847452463,-12.6209440507544));
#62402=CARTESIAN_POINT('Ctrl Pts',(15.4801979882799,2.80691883994236,-12.519816600747));
#62403=CARTESIAN_POINT('Ctrl Pts',(15.4,2.88912212849219,-12.4183522790528));
#62404=CARTESIAN_POINT('Origin',(9.65,-0.756892033916135,20.3476178712976));
#62405=CARTESIAN_POINT('',(9.61650635094611,1.11022302462516E-15,20.8232848254213));
#62406=CARTESIAN_POINT('',(8.50682667397367,-2.21935935394489,20.8232848254213));
#62407=CARTESIAN_POINT('',(9.83301270189222,-2.4,19.1876441793662));
#62408=CARTESIAN_POINT('',(9.53701905283833,-2.69599364905389,19.3585361923259));
#62409=CARTESIAN_POINT('',(9.9,-2.4,19.1102939101766));
#62410=CARTESIAN_POINT('',(12.8327618786655,-2.4,15.7238321899434));
#62411=CARTESIAN_POINT('',(9.9,5.55111512312578E-15,20.4959345562317));
#62412=CARTESIAN_POINT('',(9.9,-0.631892033916135,20.1311115203515));
#62413=CARTESIAN_POINT('',(11.1698262954046,7.21644966006352E-15,19.0296654492799));
#62414=CARTESIAN_POINT('Origin',(0.,-3.46944695195361E-16,20.8232848254213));
#62415=CARTESIAN_POINT('',(9.4,0.433012701892217,20.8232848254213));
#62416=CARTESIAN_POINT('',(6.68182667397366,5.8693593539449,20.8232848254213));
#62417=CARTESIAN_POINT('',(0.,0.433012701892218,20.8232848254213));
#62418=CARTESIAN_POINT('Origin',(7.95,-15.4169872981078,11.9222830587658));
#62419=CARTESIAN_POINT('',(15.3288252219121,-15.4169872981078,11.6722830587658));
#62420=CARTESIAN_POINT('',(7.95,-15.4169872981078,11.6722830587658));
#62421=CARTESIAN_POINT('Ctrl Pts',(15.3288252219121,-15.4169872981078,11.6722830587658));
#62422=CARTESIAN_POINT('Ctrl Pts',(15.2709785585223,-15.4169872981078,11.9203214520311));
#62423=CARTESIAN_POINT('Ctrl Pts',(15.2106539453093,-15.4169872981078,12.1722830587658));
#62424=CARTESIAN_POINT('Origin',(15.15,0.,0.));
#62425=CARTESIAN_POINT('',(15.4,-15.2561953920829,11.5794498085388));
#62426=CARTESIAN_POINT('Ctrl Pts',(15.3288252219121,-15.4169872981078,11.6722830587658));
#62427=CARTESIAN_POINT('Ctrl Pts',(15.36458562618,-15.3362065628442,11.625644279516));
#62428=CARTESIAN_POINT('Ctrl Pts',(15.4,-15.2561953920829,11.5794498085388));
#62429=CARTESIAN_POINT('',(15.9,-13.8109201357914,11.3223700194554));
#62430=CARTESIAN_POINT('Ctrl Pts',(15.9,-13.8109201357914,11.3223700194554));
#62431=CARTESIAN_POINT('Ctrl Pts',(15.6594213742065,-14.5120019863289,11.4493435458609));
#62432=CARTESIAN_POINT('Ctrl Pts',(15.4,-15.2561953920828,11.5794498085388));
#62433=CARTESIAN_POINT('',(15.9,-2.9,17.6217926969611));
#62434=CARTESIAN_POINT('Origin',(15.9,0.,0.));
#62435=CARTESIAN_POINT('',(15.4,-2.4,19.0019776789049));
#62436=CARTESIAN_POINT('Ctrl Pts',(15.4,-2.4,19.0019776789049));
#62437=CARTESIAN_POINT('Ctrl Pts',(15.6594213742039,-2.65942137420393,18.2924341528561));
#62438=CARTESIAN_POINT('Ctrl Pts',(15.9,-2.9,17.6217926969611));
#62439=CARTESIAN_POINT('',(15.3288252219091,-2.4,19.1876441793662));
#62440=CARTESIAN_POINT('Ctrl Pts',(15.4,-2.4,19.0019776789049));
#62441=CARTESIAN_POINT('Ctrl Pts',(15.3645856261785,-2.4,19.094366620863));
#62442=CARTESIAN_POINT('Ctrl Pts',(15.3288252219091,-2.4,19.1876441793662));
#62443=CARTESIAN_POINT('Ctrl Pts',(15.2106539453059,-2.83301270189222,19.4376441793662));
#62444=CARTESIAN_POINT('Ctrl Pts',(15.2709785585168,-2.61480754967826,19.3116633759969));
#62445=CARTESIAN_POINT('Ctrl Pts',(15.3288252219091,-2.4,19.1876441793662));
#62446=CARTESIAN_POINT('Origin',(15.9,-18.7185842870421,13.5784609690827));
#62447=CARTESIAN_POINT('',(9.9,-10.0850287992543,8.59387538414483));
#62448=CARTESIAN_POINT('',(9.9,-8.32627944162883,7.57846096908265));
#62449=CARTESIAN_POINT('',(9.8913964708434,-10.0774525214495,8.58950121811475));
#62450=CARTESIAN_POINT('Ctrl Pts',(9.89139647084313,-10.0774525214493,8.58950121811462));
#62451=CARTESIAN_POINT('Ctrl Pts',(9.89569679092767,-10.0812394300895,8.59168759083744));
#62452=CARTESIAN_POINT('Ctrl Pts',(9.89999999999973,-10.0850287992541,8.59387538414469));
#62453=CARTESIAN_POINT('',(15.4,-10.0774525214495,8.58950121811475));
#62454=CARTESIAN_POINT('',(0.,-10.0774525214495,8.58950121811475));
#62455=CARTESIAN_POINT('',(15.4,-8.75929214352104,7.82846096908265));
#62456=CARTESIAN_POINT('Origin',(9.9,-14.7224318643355,8.5));
#62457=CARTESIAN_POINT('Origin',(9.9,0.,0.));
#62458=CARTESIAN_POINT('Origin',(0.,18.25,10.5366424127107));
#62459=CARTESIAN_POINT('',(9.4,2.83301270189222,19.4376441793662));
#62460=CARTESIAN_POINT('',(9.4,10.0068920339161,15.2958030158883));
#62461=CARTESIAN_POINT('',(15.2106539453093,2.83301270189222,19.4376441793662));
#62462=CARTESIAN_POINT('',(7.95,2.83301270189222,19.4376441793662));
#62463=CARTESIAN_POINT('',(15.2106539453059,15.4169872981078,12.1722830587658));
#62464=CARTESIAN_POINT('Ctrl Pts',(15.2106539453093,2.83301270189222,19.4376441793662));
#62465=CARTESIAN_POINT('Ctrl Pts',(16.2489053918282,9.12499999997897,15.8049636190781));
#62466=CARTESIAN_POINT('Ctrl Pts',(15.2106539453059,15.4169872981078,12.1722830587658));
#62467=CARTESIAN_POINT('',(9.4,15.4169872981078,12.1722830587658));
#62468=CARTESIAN_POINT('',(7.95,15.4169872981078,12.1722830587658));
#62469=CARTESIAN_POINT('',(9.4,17.8169872981078,10.7866424127107));
#62470=CARTESIAN_POINT('',(9.4,17.3681079660839,11.0458030158883));
#62471=CARTESIAN_POINT('',(0.,17.8169872981078,10.7866424127107));
#62472=CARTESIAN_POINT('Origin',(9.65,9.88189203391614,15.0792966649422));
#62473=CARTESIAN_POINT('',(9.9,2.4,19.1102939101766));
#62474=CARTESIAN_POINT('',(9.9,9.75689203391614,14.8627903139961));
#62475=CARTESIAN_POINT('',(9.83301270189222,2.4,19.1876441793662));
#62476=CARTESIAN_POINT('',(11.1671033514046,2.4,17.6471689881276));
#62477=CARTESIAN_POINT('',(8.2334476242669,3.9995650776253,20.1111535075195));
#62478=CARTESIAN_POINT('Origin',(7.95,2.61650635094611,19.3126441793662));
#62479=CARTESIAN_POINT('',(15.3288252219121,2.4,19.1876441793662));
#62480=CARTESIAN_POINT('Ctrl Pts',(15.3288252219121,2.4,19.1876441793662));
#62481=CARTESIAN_POINT('Ctrl Pts',(15.2709785585223,2.6148075496816,19.3116633759989));
#62482=CARTESIAN_POINT('Ctrl Pts',(15.2106539453093,2.83301270189222,19.4376441793662));
#62483=CARTESIAN_POINT('',(7.95,2.4,19.1876441793662));
#62484=CARTESIAN_POINT('Origin',(15.9,2.4,23.));
#62485=CARTESIAN_POINT('',(9.9,2.4,13.0308288301244));
#62486=CARTESIAN_POINT('',(9.9,2.4,11.));
#62487=CARTESIAN_POINT('',(9.89139647084341,2.4,13.0220804980642));
#62488=CARTESIAN_POINT('Ctrl Pts',(9.89139647084313,2.4,13.0220804980639));
#62489=CARTESIAN_POINT('Ctrl Pts',(9.89569679092767,2.4,13.0264532435096));
#62490=CARTESIAN_POINT('Ctrl Pts',(9.89999999999972,2.4,13.0308288301241));
#62491=CARTESIAN_POINT('',(15.4,2.4,13.0220804980642));
#62492=CARTESIAN_POINT('',(0.,2.4,13.0220804980642));
#62493=CARTESIAN_POINT('',(15.4,2.4,19.0019776789123));
#62494=CARTESIAN_POINT('',(15.4,2.4,11.5));
#62495=CARTESIAN_POINT('Ctrl Pts',(15.3288252219121,2.4,19.1876441793662));
#62496=CARTESIAN_POINT('Ctrl Pts',(15.36458562618,2.4,19.0943666208667));
#62497=CARTESIAN_POINT('Ctrl Pts',(15.4,2.4,19.0019776789123));
#62498=CARTESIAN_POINT('Origin',(7.95,-2.61650635094611,19.3126441793662));
#62499=CARTESIAN_POINT('',(7.95,-2.4,19.1876441793662));
#62500=CARTESIAN_POINT('Origin',(15.9,-2.4,11.));
#62501=CARTESIAN_POINT('',(15.4,-2.4,13.0220804980642));
#62502=CARTESIAN_POINT('',(15.4,-2.4,5.5));
#62503=CARTESIAN_POINT('',(9.89139647084341,-2.4,13.0220804980642));
#62504=CARTESIAN_POINT('',(0.,-2.4,13.0220804980642));
#62505=CARTESIAN_POINT('',(9.9,-2.4,13.0308288301244));
#62506=CARTESIAN_POINT('Ctrl Pts',(9.89999999999984,-2.4,13.0308288301242));
#62507=CARTESIAN_POINT('Ctrl Pts',(9.89569679092782,-2.4,13.0264532435097));
#62508=CARTESIAN_POINT('Ctrl Pts',(9.89139647084332,-2.4,13.0220804980641));
#62509=CARTESIAN_POINT('',(9.9,-2.4,23.));
#62510=CARTESIAN_POINT('Origin',(15.65,-2.65,5.5));
#62511=CARTESIAN_POINT('',(15.9,-2.9,12.9287470390599));
#62512=CARTESIAN_POINT('',(15.9,-2.9,5.5));
#62513=CARTESIAN_POINT('',(15.6433901360358,-2.64339013603585,12.7216616766814));
#62514=CARTESIAN_POINT('Ctrl Pts',(15.9,-2.9,12.9287470390599));
#62515=CARTESIAN_POINT('Ctrl Pts',(15.770659214218,-2.77065921421805,12.8252043578707));
#62516=CARTESIAN_POINT('Ctrl Pts',(15.6433901360358,-2.64339013603585,12.7216616766814));
#62517=CARTESIAN_POINT('',(14.6907281821669,-1.6907281821669,13.8975416281819));
#62518=CARTESIAN_POINT('Origin',(15.65,0.,0.));
#62519=CARTESIAN_POINT('',(15.9,-9.74662337492871,8.97584719050482));
#62520=CARTESIAN_POINT('Origin',(15.9,0.,0.));
#62521=CARTESIAN_POINT('',(15.4,-9.31004748255804,8.71122929743642));
#62522=CARTESIAN_POINT('Ctrl Pts',(15.3999999999999,-9.31004748255797,8.71122929743639));
#62523=CARTESIAN_POINT('Ctrl Pts',(15.64392961771,-9.52336184589457,8.84027374524564));
#62524=CARTESIAN_POINT('Ctrl Pts',(15.9,-9.74662337492871,8.97584719050482));
#62525=CARTESIAN_POINT('',(15.4,-2.88912212849219,12.4183522790528));
#62526=CARTESIAN_POINT('Origin',(15.4,0.,0.));
#62527=CARTESIAN_POINT('Ctrl Pts',(15.4,-2.88912212849219,12.4183522790528));
#62528=CARTESIAN_POINT('Ctrl Pts',(15.5187354577638,-2.76741776526553,12.5685731629111));
#62529=CARTESIAN_POINT('Ctrl Pts',(15.6433901360358,-2.64339013603585,12.7216616766814));
#62530=CARTESIAN_POINT('Origin',(15.9,0.,0.));
#62531=CARTESIAN_POINT('',(15.9,-8.50929214352104,8.26147367097487));
#62532=CARTESIAN_POINT('Origin',(15.4,-9.31004748255804,8.71122929743642));
#62533=CARTESIAN_POINT('',(15.4,-9.31004748255804,8.71122929743642));
#62534=CARTESIAN_POINT('',(15.4,-10.0774525214495,8.58950121811475));
#62535=CARTESIAN_POINT('Origin',(15.65,-8.63429214352104,8.04496732002876));
#62536=CARTESIAN_POINT('Origin',(0.,-9.69375000200378,8.65036525777559));
#62537=CARTESIAN_POINT('',(9.4,-9.31004748255804,8.71122929743642));
#62538=CARTESIAN_POINT('',(0.,-9.31004748255804,8.71122929743642));
#62539=CARTESIAN_POINT('Ctrl Pts',(9.8913964708434,-10.0774525214495,8.58950121811475));
#62540=CARTESIAN_POINT('Ctrl Pts',(9.72448837871538,-9.82385455019892,8.62972768575015));
#62541=CARTESIAN_POINT('Ctrl Pts',(9.56028038038363,-9.56780623266559,8.6703428346315));
#62542=CARTESIAN_POINT('Ctrl Pts',(9.4,-9.31004748255804,8.71122929743642));
#62543=CARTESIAN_POINT('Origin',(0.,-12.3383110662499,4.06985113078293));
#62544=CARTESIAN_POINT('',(9.4,-12.1991696110502,3.70712298161641));
#62545=CARTESIAN_POINT('',(0.,-12.1991696110502,3.70712298161641));
#62546=CARTESIAN_POINT('Ctrl Pts',(9.4,-12.1991696110502,3.70712298161641));
#62547=CARTESIAN_POINT('Ctrl Pts',(9.56028038038363,-12.2926402706441,3.95079183865974));
#62548=CARTESIAN_POINT('Ctrl Pts',(9.72448837871538,-12.385490678701,4.19284376068054));
#62549=CARTESIAN_POINT('Ctrl Pts',(9.8913964708434,-12.4774525214495,4.43257927994945));
#62550=CARTESIAN_POINT('Origin',(0.,-12.3383110662499,-4.06985113078293));
#62551=CARTESIAN_POINT('',(9.4,-12.1991696110502,-3.70712298161641));
#62552=CARTESIAN_POINT('Ctrl Pts',(9.8913964708434,-12.4774525214495,-4.43257927994945));
#62553=CARTESIAN_POINT('Ctrl Pts',(9.72448837871531,-12.3854906787009,-4.19284376068043));
#62554=CARTESIAN_POINT('Ctrl Pts',(9.5602803803836,-12.292640270644,-3.95079183865968));
#62555=CARTESIAN_POINT('Ctrl Pts',(9.4,-12.1991696110502,-3.70712298161641));
#62556=CARTESIAN_POINT('',(0.,-12.1991696110502,-3.70712298161641));
#62557=CARTESIAN_POINT('Origin',(0.,-2.6445610642461,-12.7202163885585));
#62558=CARTESIAN_POINT('',(9.89139647084341,-2.4,-13.0220804980642));
#62559=CARTESIAN_POINT('',(0.,-2.4,-13.0220804980642));
#62560=CARTESIAN_POINT('',(9.4,-2.88912212849219,-12.4183522790528));
#62561=CARTESIAN_POINT('Ctrl Pts',(9.89139647084341,-2.4,-13.0220804980642));
#62562=CARTESIAN_POINT('Ctrl Pts',(9.7244883787154,-2.56163612850206,-12.8225714464307));
#62563=CARTESIAN_POINT('Ctrl Pts',(9.56028038038364,-2.72483403797847,-12.6211346732912));
#62564=CARTESIAN_POINT('Ctrl Pts',(9.4,-2.88912212849219,-12.4183522790528));
#62565=CARTESIAN_POINT('',(0.,-2.88912212849219,-12.4183522790528));
#62566=CARTESIAN_POINT('Origin',(0.,2.64456106424609,-12.7202163885585));
#62567=CARTESIAN_POINT('',(9.4,2.88912212849219,-12.4183522790528));
#62568=CARTESIAN_POINT('',(0.,2.88912212849219,-12.4183522790528));
#62569=CARTESIAN_POINT('Ctrl Pts',(9.4,2.88912212849219,-12.4183522790528));
#62570=CARTESIAN_POINT('Ctrl Pts',(9.56028038038363,2.72483403797847,-12.6211346732912));
#62571=CARTESIAN_POINT('Ctrl Pts',(9.72448837871538,2.56163612850207,-12.8225714464307));
#62572=CARTESIAN_POINT('Ctrl Pts',(9.89139647084341,2.4,-13.0220804980642));
#62573=CARTESIAN_POINT('Origin',(0.,9.69375000200378,-8.65036525777559));
#62574=CARTESIAN_POINT('',(9.4,9.31004748255804,-8.71122929743643));
#62575=CARTESIAN_POINT('Ctrl Pts',(9.89139647084341,10.0774525214495,-8.58950121811476));
#62576=CARTESIAN_POINT('Ctrl Pts',(9.72448837871533,9.82385455019883,-8.62972768575017));
#62577=CARTESIAN_POINT('Ctrl Pts',(9.56028038038361,9.56780623266555,-8.67034283463151));
#62578=CARTESIAN_POINT('Ctrl Pts',(9.4,9.31004748255804,-8.71122929743643));
#62579=CARTESIAN_POINT('',(0.,9.31004748255804,-8.71122929743643));
#62580=CARTESIAN_POINT('Origin',(0.,12.3383110662499,-4.06985113078294));
#62581=CARTESIAN_POINT('',(9.89139647084341,12.4774525214495,-4.43257927994946));
#62582=CARTESIAN_POINT('',(15.4,12.4774525214495,-4.43257927994946));
#62583=CARTESIAN_POINT('',(0.,12.4774525214495,-4.43257927994946));
#62584=CARTESIAN_POINT('',(15.6433901361021,12.3389772584149,-4.07158782840527));
#62585=CARTESIAN_POINT('',(14.6907281821669,12.8809881912407,-5.48455725744011));
#62586=CARTESIAN_POINT('',(15.4,12.1991696110502,-3.70712298161642));
#62587=CARTESIAN_POINT('Ctrl Pts',(15.6433901361021,12.3389772584149,-4.07158782840527));
#62588=CARTESIAN_POINT('Ctrl Pts',(15.5187354576438,12.2684125309717,-3.88763249356148));
#62589=CARTESIAN_POINT('Ctrl Pts',(15.3999999996623,12.1991696108533,-3.70712298110308));
#62590=CARTESIAN_POINT('',(9.4,12.1991696110502,-3.70712298161642));
#62591=CARTESIAN_POINT('',(0.,12.1991696110502,-3.70712298161642));
#62592=CARTESIAN_POINT('Ctrl Pts',(9.4,12.1991696110502,-3.70712298161642));
#62593=CARTESIAN_POINT('Ctrl Pts',(9.56028038038363,12.292640270644,-3.95079183865973));
#62594=CARTESIAN_POINT('Ctrl Pts',(9.72448837871537,12.385490678701,-4.19284376068052));
#62595=CARTESIAN_POINT('Ctrl Pts',(9.89139647084341,12.4774525214495,-4.43257927994946));
#62596=CARTESIAN_POINT('Origin',(9.65,0.,0.));
#62597=CARTESIAN_POINT('Ctrl Pts',(9.89999999999984,12.4850287992542,-4.43695344597945));
#62598=CARTESIAN_POINT('Ctrl Pts',(9.89569679092782,12.4812394300896,-4.43476565267222));
#62599=CARTESIAN_POINT('Ctrl Pts',(9.89139647084332,12.4774525214494,-4.43257927994942));
#62600=CARTESIAN_POINT('Origin',(9.4,0.,0.));
#62601=CARTESIAN_POINT('Origin',(9.65,0.,0.));
#62602=CARTESIAN_POINT('',(9.9,-2.4,-13.0308288301244));
#62603=CARTESIAN_POINT('Origin',(9.9,0.,0.));
#62604=CARTESIAN_POINT('Origin',(9.4,0.,0.));
#62605=CARTESIAN_POINT('Ctrl Pts',(9.89139647084313,-2.4,-13.0220804980639));
#62606=CARTESIAN_POINT('Ctrl Pts',(9.89569679092767,-2.4,-13.0264532435096));
#62607=CARTESIAN_POINT('Ctrl Pts',(9.89999999999973,-2.4,-13.0308288301241));
#62608=CARTESIAN_POINT('Origin',(0.,-9.69375000200378,-8.65036525777559));
#62609=CARTESIAN_POINT('',(9.4,-9.31004748255804,-8.71122929743642));
#62610=CARTESIAN_POINT('',(0.,-9.31004748255804,-8.71122929743642));
#62611=CARTESIAN_POINT('',(9.89139647084341,-10.0774525214495,-8.58950121811475));
#62612=CARTESIAN_POINT('Ctrl Pts',(9.4,-9.31004748255804,-8.71122929743642));
#62613=CARTESIAN_POINT('Ctrl Pts',(9.56028038038362,-9.56780623266557,-8.6703428346315));
#62614=CARTESIAN_POINT('Ctrl Pts',(9.72448837871536,-9.82385455019888,-8.62972768575016));
#62615=CARTESIAN_POINT('Ctrl Pts',(9.89139647084341,-10.0774525214495,-8.58950121811475));
#62616=CARTESIAN_POINT('',(0.,-10.0774525214495,-8.58950121811475));
#62617=CARTESIAN_POINT('Origin',(9.65,0.,0.));
#62618=CARTESIAN_POINT('Ctrl Pts',(9.89999999999984,-10.0850287992542,-8.59387538414475));
#62619=CARTESIAN_POINT('Ctrl Pts',(9.89569679092782,-10.0812394300896,-8.59168759083752));
#62620=CARTESIAN_POINT('Ctrl Pts',(9.89139647084332,-10.0774525214494,-8.58950121811471));
#62621=CARTESIAN_POINT('Origin',(9.4,0.,0.));
#62622=CARTESIAN_POINT('Origin',(9.65,0.,0.));
#62623=CARTESIAN_POINT('Origin',(9.4,0.,0.));
#62624=CARTESIAN_POINT('Origin',(0.,-2.64456106424609,12.7202163885585));
#62625=CARTESIAN_POINT('',(9.4,-2.88912212849219,12.4183522790528));
#62626=CARTESIAN_POINT('',(0.,-2.88912212849219,12.4183522790528));
#62627=CARTESIAN_POINT('Ctrl Pts',(9.4,-2.88912212849219,12.4183522790528));
#62628=CARTESIAN_POINT('Ctrl Pts',(9.56028038038363,-2.72483403797847,12.6211346732912));
#62629=CARTESIAN_POINT('Ctrl Pts',(9.72448837871539,-2.56163612850206,12.8225714464307));
#62630=CARTESIAN_POINT('Ctrl Pts',(9.89139647084341,-2.4,13.0220804980642));
#62631=CARTESIAN_POINT('Origin',(0.,0.,0.));
#62632=CARTESIAN_POINT('',(15.4,12.1991696110502,3.70712298161641));
#62633=CARTESIAN_POINT('Origin',(15.4,0.,0.));
#62634=CARTESIAN_POINT('',(9.4,12.1991696110502,3.70712298161641));
#62635=CARTESIAN_POINT('',(0.,12.1991696110502,3.70712298161641));
#62636=CARTESIAN_POINT('',(9.4,9.31004748255805,8.71122929743641));
#62637=CARTESIAN_POINT('Origin',(9.4,0.,0.));
#62638=CARTESIAN_POINT('',(15.4,9.31004748255805,8.71122929743641));
#62639=CARTESIAN_POINT('',(0.,9.31004748255805,8.71122929743641));
#62640=CARTESIAN_POINT('',(15.4,2.88912212849219,12.4183522790528));
#62641=CARTESIAN_POINT('Origin',(15.4,0.,0.));
#62642=CARTESIAN_POINT('',(9.4,2.88912212849219,12.4183522790528));
#62643=CARTESIAN_POINT('',(0.,2.88912212849219,12.4183522790528));
#62644=CARTESIAN_POINT('',(9.4,-1.56142466891288E-15,12.75));
#62645=CARTESIAN_POINT('Origin',(9.4,0.,0.));
#62646=CARTESIAN_POINT('',(0.600000000000001,-1.56142466891288E-15,12.75));
#62647=CARTESIAN_POINT('',(0.,-1.56142466891288E-15,12.75));
#62648=CARTESIAN_POINT('',(0.600000000000003,-12.75,-1.56142466891287E-15));
#62649=CARTESIAN_POINT('Origin',(0.600000000000001,0.,0.));
#62650=CARTESIAN_POINT('Origin',(0.600000000000001,0.,0.));
#62651=CARTESIAN_POINT('Origin',(9.4,0.,0.));
#62652=CARTESIAN_POINT('Origin',(15.65,0.,0.));
#62653=CARTESIAN_POINT('',(15.9,12.6466233749287,-3.95289984855508));
#62654=CARTESIAN_POINT('Ctrl Pts',(15.9,12.6466233749287,-3.95289984855508));
#62655=CARTESIAN_POINT('Ctrl Pts',(15.8143094271252,12.5443697249457,-3.99281062684437));
#62656=CARTESIAN_POINT('Ctrl Pts',(15.7287625868629,12.441814765937,-4.0323814761614));
#62657=CARTESIAN_POINT('Ctrl Pts',(15.6433901361021,12.3389772584547,-4.07158782838998));
#62658=CARTESIAN_POINT('',(15.9,12.6466233749287,3.95289984855507));
#62659=CARTESIAN_POINT('Origin',(15.9,0.,0.));
#62660=CARTESIAN_POINT('Ctrl Pts',(15.4,12.1991696110502,3.7071229816164));
#62661=CARTESIAN_POINT('Ctrl Pts',(15.64392961771,12.4175825627386,3.82733641535336));
#62662=CARTESIAN_POINT('Ctrl Pts',(15.9,12.6466233749287,3.95289984855507));
#62663=CARTESIAN_POINT('Origin',(15.65,6.08813972081441,-0.455032679971241));
#62664=CARTESIAN_POINT('',(15.4,17.6561953920766,-7.42252787036989));
#62665=CARTESIAN_POINT('',(15.4,5.96313972081441,-0.67153903091735));
#62666=CARTESIAN_POINT('',(15.9,16.7109201357914,-6.29942267750569));
#62667=CARTESIAN_POINT('Ctrl Pts',(15.4,17.6561953920766,-7.42252787036989));
#62668=CARTESIAN_POINT('Ctrl Pts',(15.659421374204,17.1714233605295,-6.84309060700007));
#62669=CARTESIAN_POINT('Ctrl Pts',(15.9,16.7109201357914,-6.29942267750569));
#62670=CARTESIAN_POINT('',(15.9,6.21313972081441,-0.238526329025132));
#62671=CARTESIAN_POINT('Origin',(7.95,18.0334936490539,-7.39036112060048));
#62672=CARTESIAN_POINT('',(15.2106539453059,18.25,-7.26536112060048));
#62673=CARTESIAN_POINT('',(7.95,18.25,-7.26536112060048));
#62674=CARTESIAN_POINT('',(15.3288252219092,17.8169872981078,-7.51536112060048));
#62675=CARTESIAN_POINT('Ctrl Pts',(15.2106539453059,18.25,-7.26536112060048));
#62676=CARTESIAN_POINT('Ctrl Pts',(15.2709785585169,18.031794847786,-7.39134192396977));
#62677=CARTESIAN_POINT('Ctrl Pts',(15.3288252219092,17.8169872981078,-7.51536112060048));
#62678=CARTESIAN_POINT('',(7.95,17.8169872981078,-7.51536112060048));
#62679=CARTESIAN_POINT('Origin',(0.,18.0334936490539,-10.4116424127107));
#62680=CARTESIAN_POINT('',(0.,18.25,-10.0366424127107));
#62681=CARTESIAN_POINT('Origin',(15.15,0.,0.));
#62682=CARTESIAN_POINT('',(15.2106539453093,18.25,7.26536112060045));
#62683=CARTESIAN_POINT('Ctrl Pts',(15.2106539453093,18.25,7.26536112060045));
#62684=CARTESIAN_POINT('Ctrl Pts',(16.2489053918282,18.25,2.42850184406507E-11));
#62685=CARTESIAN_POINT('Ctrl Pts',(15.2106539453059,18.25,-7.26536112060048));
#62686=CARTESIAN_POINT('',(15.3288252219121,17.8169872981078,7.51536112060045));
#62687=CARTESIAN_POINT('Ctrl Pts',(15.3288252219121,17.8169872981078,7.51536112060045));
#62688=CARTESIAN_POINT('Ctrl Pts',(15.2709785585222,18.0317948477897,7.39134192396766));
#62689=CARTESIAN_POINT('Ctrl Pts',(15.2106539453093,18.25,7.26536112060045));
#62690=CARTESIAN_POINT('',(15.4,17.6561953920829,7.42252787037345));
#62691=CARTESIAN_POINT('Ctrl Pts',(15.3288252219121,17.8169872981078,7.51536112060045));
#62692=CARTESIAN_POINT('Ctrl Pts',(15.3645856261801,17.736206562844,7.46872234135055));
#62693=CARTESIAN_POINT('Ctrl Pts',(15.4,17.6561953920829,7.42252787037345));
#62694=CARTESIAN_POINT('',(15.9,16.7109201357914,6.29942267750566));
#62695=CARTESIAN_POINT('Ctrl Pts',(15.9,16.7109201357914,6.29942267750567));
#62696=CARTESIAN_POINT('Ctrl Pts',(15.6594213742065,17.1714233605353,6.84309060700057));
#62697=CARTESIAN_POINT('Ctrl Pts',(15.4,17.6561953920829,7.42252787037345));
#62698=CARTESIAN_POINT('Origin',(15.9,0.,0.));
#62699=CARTESIAN_POINT('Ctrl Pts',(15.4,17.6561953920766,-7.42252787036989));
#62700=CARTESIAN_POINT('Ctrl Pts',(15.3645856261794,17.736206562839,-7.46872234134772));
#62701=CARTESIAN_POINT('Ctrl Pts',(15.3288252219092,17.8169872981078,-7.51536112060048));
#62702=CARTESIAN_POINT('Origin',(0.,18.25,-10.5366424127107));
#62703=CARTESIAN_POINT('',(9.4,18.25,10.0366424127107));
#62704=CARTESIAN_POINT('',(0.,18.25,10.0366424127107));
#62705=CARTESIAN_POINT('',(9.4,18.25,7.26536112060045));
#62706=CARTESIAN_POINT('',(9.4,18.25,-1.01832120635535));
#62707=CARTESIAN_POINT('',(7.95,18.25,7.26536112060045));
#62708=CARTESIAN_POINT('Origin',(15.4,2.88912212849219,12.4183522790528));
#62709=CARTESIAN_POINT('',(15.4,2.88912212849219,12.4183522790528));
#62710=CARTESIAN_POINT('',(15.9,2.9,12.9287470390599));
#62711=CARTESIAN_POINT('Ctrl Pts',(15.4,2.88912212849219,12.4183522790528));
#62712=CARTESIAN_POINT('Ctrl Pts',(15.64392961771,2.89422071684404,12.667610160599));
#62713=CARTESIAN_POINT('Ctrl Pts',(15.9,2.9,12.9287470390599));
#62714=CARTESIAN_POINT('',(15.4,2.4,13.0220804980642));
#62715=CARTESIAN_POINT('Origin',(15.4,9.31004748255805,8.71122929743641));
#62716=CARTESIAN_POINT('',(15.9,9.74662337492872,8.97584719050481));
#62717=CARTESIAN_POINT('Ctrl Pts',(15.9,9.74662337492871,8.97584719050482));
#62718=CARTESIAN_POINT('Ctrl Pts',(15.64392961771,9.5233618458946,8.84027374524565));
#62719=CARTESIAN_POINT('Ctrl Pts',(15.4,9.31004748255803,8.71122929743641));
#62720=CARTESIAN_POINT('',(15.4,10.0774525214495,8.58950121811475));
#62721=CARTESIAN_POINT('',(15.4,10.0774525214495,8.58950121811475));
#62722=CARTESIAN_POINT('',(15.9,9.74662337492872,8.97584719050481));
#62723=CARTESIAN_POINT('Origin',(0.,9.69375000200379,8.65036525777558));
#62724=CARTESIAN_POINT('',(9.8913964708434,10.0774525214495,8.58950121811475));
#62725=CARTESIAN_POINT('',(0.,10.0774525214495,8.58950121811475));
#62726=CARTESIAN_POINT('Ctrl Pts',(9.4,9.31004748255805,8.71122929743641));
#62727=CARTESIAN_POINT('Ctrl Pts',(9.56028038038361,9.56780623266555,8.6703428346315));
#62728=CARTESIAN_POINT('Ctrl Pts',(9.72448837871532,9.82385455019883,8.62972768575016));
#62729=CARTESIAN_POINT('Ctrl Pts',(9.8913964708434,10.0774525214495,8.58950121811475));
#62730=CARTESIAN_POINT('Origin',(15.4,12.1991696110502,3.70712298161641));
#62731=CARTESIAN_POINT('',(15.4,12.4774525214495,4.43257927994945));
#62732=CARTESIAN_POINT('',(15.4,12.1991696110502,3.70712298161641));
#62733=CARTESIAN_POINT('',(15.4,12.4774525214495,4.43257927994945));
#62734=CARTESIAN_POINT('Origin',(15.65,11.284292143521,3.45503267997123));
#62735=CARTESIAN_POINT('',(15.4,11.159292143521,3.67153903091734));
#62736=CARTESIAN_POINT('',(15.9,11.409292143521,3.23852632902512));
#62737=CARTESIAN_POINT('Origin',(0.,12.3383110662499,4.06985113078293));
#62738=CARTESIAN_POINT('',(9.89139647084341,12.4774525214495,4.43257927994945));
#62739=CARTESIAN_POINT('',(0.,12.4774525214495,4.43257927994945));
#62740=CARTESIAN_POINT('Ctrl Pts',(9.89139647084341,12.4774525214495,4.43257927994944));
#62741=CARTESIAN_POINT('Ctrl Pts',(9.72448837871538,12.385490678701,4.19284376068052));
#62742=CARTESIAN_POINT('Ctrl Pts',(9.56028038038363,12.2926402706441,3.95079183865972));
#62743=CARTESIAN_POINT('Ctrl Pts',(9.4,12.1991696110502,3.7071229816164));
#62744=CARTESIAN_POINT('Origin',(9.65,0.,0.));
#62745=CARTESIAN_POINT('',(9.9,12.4850287992543,4.43695344597951));
#62746=CARTESIAN_POINT('Ctrl Pts',(9.89139647084313,12.4774525214493,4.4325792799493));
#62747=CARTESIAN_POINT('Ctrl Pts',(9.89569679092767,12.4812394300895,4.43476565267213));
#62748=CARTESIAN_POINT('Ctrl Pts',(9.89999999999972,12.4850287992541,4.43695344597937));
#62749=CARTESIAN_POINT('',(9.9,10.0850287992544,8.59387538414482));
#62750=CARTESIAN_POINT('Origin',(9.9,0.,0.));
#62751=CARTESIAN_POINT('Ctrl Pts',(9.89999999999984,10.0850287992542,8.59387538414474));
#62752=CARTESIAN_POINT('Ctrl Pts',(9.89569679092782,10.0812394300896,8.59168759083751));
#62753=CARTESIAN_POINT('Ctrl Pts',(9.89139647084332,10.0774525214494,8.5895012181147));
#62754=CARTESIAN_POINT('Origin',(15.65,3.43813972081442,5.04496732002876));
#62755=CARTESIAN_POINT('',(15.4,15.2561953920765,11.5794498085351));
#62756=CARTESIAN_POINT('',(15.9,13.8109201357914,11.3223700194554));
#62757=CARTESIAN_POINT('Ctrl Pts',(15.4,15.2561953920765,11.5794498085351));
#62758=CARTESIAN_POINT('Ctrl Pts',(15.6594213742041,14.5120019863252,11.449343545856));
#62759=CARTESIAN_POINT('Ctrl Pts',(15.9,13.8109201357914,11.3223700194554));
#62760=CARTESIAN_POINT('',(15.9,3.31313972081442,5.26147367097487));
#62761=CARTESIAN_POINT('',(15.4,3.56313972081442,4.82846096908265));
#62762=CARTESIAN_POINT('Origin',(15.65,0.,0.));
#62763=CARTESIAN_POINT('Origin',(15.9,0.,0.));
#62764=CARTESIAN_POINT('Origin',(15.65,2.65,11.5));
#62765=CARTESIAN_POINT('',(15.9,2.9,17.6217926969611));
#62766=CARTESIAN_POINT('Ctrl Pts',(15.9,2.9,17.6217926969611));
#62767=CARTESIAN_POINT('Ctrl Pts',(15.6594213742065,2.65942137420647,18.2924341528615));
#62768=CARTESIAN_POINT('Ctrl Pts',(15.4,2.4,19.0019776789123));
#62769=CARTESIAN_POINT('',(15.9,2.9,11.5));
#62770=CARTESIAN_POINT('Origin',(0.,2.64456106424609,12.7202163885585));
#62771=CARTESIAN_POINT('Ctrl Pts',(9.89139647084341,2.4,13.0220804980642));
#62772=CARTESIAN_POINT('Ctrl Pts',(9.72448837871539,2.56163612850206,12.8225714464307));
#62773=CARTESIAN_POINT('Ctrl Pts',(9.56028038038364,2.72483403797846,12.6211346732912));
#62774=CARTESIAN_POINT('Ctrl Pts',(9.4,2.88912212849219,12.4183522790528));
#62775=CARTESIAN_POINT('Origin',(9.65,0.,0.));
#62776=CARTESIAN_POINT('Origin',(9.9,0.,0.));
#62777=CARTESIAN_POINT('Origin',(15.9,10.7262794416288,-3.42153903091735));
#62778=CARTESIAN_POINT('Origin',(9.9,0.,17.));
#62779=CARTESIAN_POINT('Origin',(7.95,15.4169872981078,11.9222830587658));
#62780=CARTESIAN_POINT('',(15.3288252219091,15.4169872981078,11.6722830587658));
#62781=CARTESIAN_POINT('Ctrl Pts',(15.2106539453059,15.4169872981078,12.1722830587658));
#62782=CARTESIAN_POINT('Ctrl Pts',(15.2709785585168,15.4169872981078,11.9203214520272));
#62783=CARTESIAN_POINT('Ctrl Pts',(15.3288252219091,15.4169872981078,11.6722830587658));
#62784=CARTESIAN_POINT('',(9.83301270189222,15.4169872981078,11.6722830587658));
#62785=CARTESIAN_POINT('',(7.95,15.4169872981078,11.6722830587658));
#62786=CARTESIAN_POINT('',(9.83301270189222,15.4169872981078,11.6722830587658));
#62787=CARTESIAN_POINT('Origin',(9.9,17.75,10.2479672781159));
#62788=CARTESIAN_POINT('',(9.4,17.8169872981078,10.7866424127107));
#62789=CARTESIAN_POINT('',(9.9,17.75,10.2479672781159));
#62790=CARTESIAN_POINT('',(9.9,17.75,10.2479672781159));
#62791=CARTESIAN_POINT('',(9.4,18.25,10.0366424127107));
#62792=CARTESIAN_POINT('Origin',(9.65,17.2431079660839,10.8292966649422));
#62793=CARTESIAN_POINT('',(9.9,15.35,11.633607924171));
#62794=CARTESIAN_POINT('',(9.9,17.1181079660839,10.6127903139961));
#62795=CARTESIAN_POINT('',(12.8327618786655,12.4172381213345,9.94037706405436));
#62796=CARTESIAN_POINT('Origin',(7.95,18.0334936490539,7.39036112060045));
#62797=CARTESIAN_POINT('',(9.83301270189222,17.8169872981078,7.51536112060045));
#62798=CARTESIAN_POINT('',(7.95,17.8169872981078,7.51536112060045));
#62799=CARTESIAN_POINT('',(9.4,18.25,7.26536112060045));
#62800=CARTESIAN_POINT('Origin',(9.65,18.,-1.01832120635535));
#62801=CARTESIAN_POINT('',(9.9,17.75,7.47668598600564));
#62802=CARTESIAN_POINT('',(9.9,17.75,-1.01832120635535));
#62803=CARTESIAN_POINT('',(11.1671033514046,16.4828966485954,6.74512352498114));
#62804=CARTESIAN_POINT('Origin',(0.,18.0334936490539,10.4116424127107));
#62805=CARTESIAN_POINT('Origin',(15.15,0.,0.));
#62806=CARTESIAN_POINT('Origin',(15.9,0.,0.));
#62807=CARTESIAN_POINT('Ctrl Pts',(15.4,15.2561953920765,11.5794498085351));
#62808=CARTESIAN_POINT('Ctrl Pts',(15.3645856261785,15.336206562841,11.6256442795142));
#62809=CARTESIAN_POINT('Ctrl Pts',(15.3288252219091,15.4169872981078,11.6722830587658));
#62810=CARTESIAN_POINT('Origin',(0.25,0.,0.));
#62811=CARTESIAN_POINT('',(0.,-13.3071428571429,-1.62965499057966E-15));
#62812=CARTESIAN_POINT('Origin',(0.,0.,0.));
#62813=CARTESIAN_POINT('',(0.25,-13.075,-1.60122568988516E-15));
#62814=CARTESIAN_POINT('Origin',(15.9,21.1185842870421,9.42153903091733));
#62815=CARTESIAN_POINT('',(9.9,10.7262794416288,3.42153903091734));
#62816=CARTESIAN_POINT('Origin',(15.9,8.32627944162883,7.57846096908265));
#62817=CARTESIAN_POINT('',(9.9,18.7185842870421,13.5784609690826));
#62818=CARTESIAN_POINT('Origin',(9.9,14.7224318643355,8.49999999999999));
#62819=CARTESIAN_POINT('Origin',(15.9,0.,0.));
#62820=CARTESIAN_POINT('Origin',(15.9,0.,0.));
#62821=CARTESIAN_POINT('Origin',(15.9,-2.4,-23.));
#62822=CARTESIAN_POINT('',(9.9,-2.4,-11.));
#62823=CARTESIAN_POINT('Origin',(9.9,-2.0818995585505E-15,-17.));
#62824=CARTESIAN_POINT('Origin',(15.9,-8.32627944162883,-7.57846096908265));
#62825=CARTESIAN_POINT('Origin',(0.,-18.25,10.5366424127107));
#62826=CARTESIAN_POINT('Origin',(0.,0.,0.));
#62827=CARTESIAN_POINT('',(0.,0.,0.));
#62828=CARTESIAN_POINT('Origin',(109.5,0.,17.1));
#62829=CARTESIAN_POINT('',(110.957496466156,0.968609344154195,17.2));
#62830=CARTESIAN_POINT('',(111.26134813329,0.836751309143921,17.0000000000042));
#62831=CARTESIAN_POINT('Ctrl Pts',(111.261348133289,0.836751309140648,17.0000000000024));
#62832=CARTESIAN_POINT('Ctrl Pts',(111.193368852489,0.880393938856773,17.0426754624596));
#62833=CARTESIAN_POINT('Ctrl Pts',(111.121707329493,0.915065044515368,17.088908703297));
#62834=CARTESIAN_POINT('Ctrl Pts',(111.018383164403,0.951678216844113,17.1581953291081));
#62835=CARTESIAN_POINT('Ctrl Pts',(110.987987650589,0.960873765425233,17.1788868315244));
#62836=CARTESIAN_POINT('Ctrl Pts',(110.957496464733,0.968609345524605,17.1999999974435));
#62837=CARTESIAN_POINT('',(109.5,-1.95,17.0000000000057));
#62838=CARTESIAN_POINT('Origin',(109.5,0.,17.));
#62839=CARTESIAN_POINT('',(111.261348133293,-0.836751309138393,17.0000000000001));
#62840=CARTESIAN_POINT('Origin',(109.5,0.,17.));
#62841=CARTESIAN_POINT('',(110.957496466156,-0.968609344154194,17.2));
#62842=CARTESIAN_POINT('Ctrl Pts',(110.957496464733,-0.968609345524603,
17.1999999974435));
#62843=CARTESIAN_POINT('Ctrl Pts',(111.001101495698,-0.957546797437459,
17.1698063454805));
#62844=CARTESIAN_POINT('Ctrl Pts',(111.044512077677,-0.943498238918733,
17.1404742731241));
#62845=CARTESIAN_POINT('Ctrl Pts',(111.147005642954,-0.902487957738779,
17.0726239093433));
#62846=CARTESIAN_POINT('Ctrl Pts',(111.20542520737,-0.872653771182455,17.0351068251626));
#62847=CARTESIAN_POINT('Ctrl Pts',(111.261348133292,-0.836751309139038,
17.0000000000008));
#62848=CARTESIAN_POINT('Origin',(109.5,0.,17.2));
#62849=CARTESIAN_POINT('Origin',(109.5,0.,-16.));
#62850=CARTESIAN_POINT('Ctrl Pts',(111.261348133291,0.836751309142101,17.0000000000057));
#62851=CARTESIAN_POINT('Ctrl Pts',(111.271270988545,0.815863857414333,16.9694752063524));
#62852=CARTESIAN_POINT('Ctrl Pts',(111.281647172364,0.79306554162572,16.9403253270067));
#62853=CARTESIAN_POINT('Ctrl Pts',(111.325941268158,0.689755334685708,16.8242697948987));
#62854=CARTESIAN_POINT('Ctrl Pts',(111.360584011539,0.594205474502249,16.7528911725506));
#62855=CARTESIAN_POINT('Ctrl Pts',(111.417556923573,0.37310394039917,16.643452411098));
#62856=CARTESIAN_POINT('Ctrl Pts',(111.438467087766,0.248212018892159,16.6083564739943));
#62857=CARTESIAN_POINT('Ctrl Pts',(111.454232282562,-0.00969172202381931,
16.5815554081639));
#62858=CARTESIAN_POINT('Ctrl Pts',(111.449047773732,-0.140002812849383,
16.5898935474965));
#62859=CARTESIAN_POINT('Ctrl Pts',(111.414723878012,-0.390345158053136,
16.6498762958916));
#62860=CARTESIAN_POINT('Ctrl Pts',(111.385873474846,-0.507644453415908,
16.7010984120851));
#62861=CARTESIAN_POINT('Ctrl Pts',(111.327369049441,-0.685129348563325,
16.8248010526809));
#62862=CARTESIAN_POINT('Ctrl Pts',(111.300518338828,-0.751237326031986,
16.887053403656));
#62863=CARTESIAN_POINT('Ctrl Pts',(111.270547957266,-0.817184329085975,
16.9722816702371));
#62864=CARTESIAN_POINT('Ctrl Pts',(111.265899036497,-0.827171730624058,
16.9860004628025));
#62865=CARTESIAN_POINT('Ctrl Pts',(111.261348133293,-0.836751309138331,
17.0000000000002));
#62866=CARTESIAN_POINT('',(109.5,-1.95,15.5));
#62867=CARTESIAN_POINT('',(109.5,-1.95,-16.));
#62868=CARTESIAN_POINT('',(109.84835607319,-1.9186318162356,15.5));
#62869=CARTESIAN_POINT('Origin',(109.5,0.,15.5));
#62870=CARTESIAN_POINT('',(109.84835607319,-1.9186318162356,-15.6));
#62871=CARTESIAN_POINT('',(109.84835607319,-1.9186318162356,-16.));
#62872=CARTESIAN_POINT('',(109.84835607319,1.9186318162356,-15.6));
#62873=CARTESIAN_POINT('Origin',(109.5,0.,-15.6));
#62874=CARTESIAN_POINT('',(109.84835607319,1.9186318162356,15.5));
#62875=CARTESIAN_POINT('',(109.84835607319,1.9186318162356,-16.));
#62876=CARTESIAN_POINT('',(109.15164392681,1.9186318162356,15.5));
#62877=CARTESIAN_POINT('Origin',(109.5,0.,15.5));
#62878=CARTESIAN_POINT('',(109.15164392681,1.9186318162356,-15.6));
#62879=CARTESIAN_POINT('',(109.15164392681,1.9186318162356,-16.));
#62880=CARTESIAN_POINT('',(109.15164392681,-1.9186318162356,-15.6));
#62881=CARTESIAN_POINT('Origin',(109.5,0.,-15.6));
#62882=CARTESIAN_POINT('',(109.15164392681,-1.9186318162356,15.5));
#62883=CARTESIAN_POINT('',(109.15164392681,-1.9186318162356,-16.));
#62884=CARTESIAN_POINT('Origin',(109.5,0.,15.5));
#62885=CARTESIAN_POINT('Origin',(109.749178036595,-1.83142701287898,-16.));
#62886=CARTESIAN_POINT('',(109.750434791609,-1.83253209412259,-15.7004347680384));
#62887=CARTESIAN_POINT('Ctrl Pts',(109.750434791609,-1.83253209412259,-15.7004347680384));
#62888=CARTESIAN_POINT('Ctrl Pts',(109.798101224611,-1.87444401393227,-15.6524546953631));
#62889=CARTESIAN_POINT('Ctrl Pts',(109.84835607319,-1.91863181623643,-15.5999999999986));
#62890=CARTESIAN_POINT('',(109.65,-1.74422220952236,15.5));
#62891=CARTESIAN_POINT('',(109.1825212855,-1.33317969677524,15.5));
#62892=CARTESIAN_POINT('',(109.65,-1.74422220952236,-15.6));
#62893=CARTESIAN_POINT('',(109.65,-1.74422220952236,-16.));
#62894=CARTESIAN_POINT('',(109.549428171904,-1.65579187964854,-15.4994281719038));
#62895=CARTESIAN_POINT('Origin',(109.5,0.,-15.8));
#62896=CARTESIAN_POINT('',(110.05,-1.44913767461895,-16.));
#62897=CARTESIAN_POINT('Ctrl Pts',(109.750434784424,-1.83253210215193,-15.7004347844244));
#62898=CARTESIAN_POINT('Ctrl Pts',(109.855124020005,-1.71256291063752,-15.8051240200051));
#62899=CARTESIAN_POINT('Ctrl Pts',(109.956584644308,-1.58450938593979,-15.9065846443083));
#62900=CARTESIAN_POINT('Ctrl Pts',(110.05,-1.44913767461895,-16.));
#62901=CARTESIAN_POINT('',(110.05,1.44913767461896,-16.));
#62902=CARTESIAN_POINT('Origin',(109.5,0.,-16.));
#62903=CARTESIAN_POINT('',(109.750434791609,1.83253209412259,-15.7004347680384));
#62904=CARTESIAN_POINT('Ctrl Pts',(109.750434784424,1.83253210215196,-15.7004347844244));
#62905=CARTESIAN_POINT('Ctrl Pts',(109.855124020005,1.71256291063753,-15.8051240200051));
#62906=CARTESIAN_POINT('Ctrl Pts',(109.956584644308,1.58450938593979,-15.9065846443083));
#62907=CARTESIAN_POINT('Ctrl Pts',(110.05,1.44913767461895,-16.));
#62908=CARTESIAN_POINT('Ctrl Pts',(109.84835607319,1.91863181623643,-15.5999999999986));
#62909=CARTESIAN_POINT('Ctrl Pts',(109.79810122461,1.87444401393154,-15.6524546953639));
#62910=CARTESIAN_POINT('Ctrl Pts',(109.750434791609,1.83253209412259,-15.7004347680384));
#62911=CARTESIAN_POINT('Origin',(109.85,0.,-15.8));
#62912=CARTESIAN_POINT('',(109.65,1.74422220952236,-15.6));
#62913=CARTESIAN_POINT('',(109.65,0.,-15.6));
#62914=CARTESIAN_POINT('',(109.549428171904,1.65579187964854,-15.4994281719038));
#62915=CARTESIAN_POINT('',(110.05,0.,-16.));
#62916=CARTESIAN_POINT('Origin',(109.65,0.,15.5));
#62917=CARTESIAN_POINT('',(109.65,1.74422220952236,15.5));
#62918=CARTESIAN_POINT('',(109.65,0.,15.5));
#62919=CARTESIAN_POINT('',(109.65,1.74422220952236,-16.));
#62920=CARTESIAN_POINT('Origin',(109.250821963405,-1.83142701287898,-16.));
#62921=CARTESIAN_POINT('',(109.249565208391,-1.83253209412259,-15.7004347680384));
#62922=CARTESIAN_POINT('',(109.35,-1.74422220952236,-15.6));
#62923=CARTESIAN_POINT('',(109.450571828096,-1.65579187964854,-15.4994281719038));
#62924=CARTESIAN_POINT('',(109.35,-1.74422220952236,15.5));
#62925=CARTESIAN_POINT('',(109.35,-1.74422220952236,-16.));
#62926=CARTESIAN_POINT('',(109.732882317017,-1.40756322422156,15.5));
#62927=CARTESIAN_POINT('Ctrl Pts',(109.15164392681,-1.91863181623643,-15.5999999999986));
#62928=CARTESIAN_POINT('Ctrl Pts',(109.20189877539,-1.87444401393148,-15.652454695364));
#62929=CARTESIAN_POINT('Ctrl Pts',(109.249565208391,-1.83253209412259,-15.7004347680384));
#62930=CARTESIAN_POINT('Origin',(109.35,0.,-16.5));
#62931=CARTESIAN_POINT('',(109.35,1.74422220952236,-15.6));
#62932=CARTESIAN_POINT('',(109.35,0.,-15.6));
#62933=CARTESIAN_POINT('',(109.35,1.74422220952236,15.5));
#62934=CARTESIAN_POINT('',(109.35,1.74422220952236,-16.));
#62935=CARTESIAN_POINT('',(109.35,0.,15.5));
#62936=CARTESIAN_POINT('Origin',(109.15,0.,-15.8));
#62937=CARTESIAN_POINT('',(108.95,-1.44913767461896,-16.));
#62938=CARTESIAN_POINT('Ctrl Pts',(108.95,-1.44913767461895,-16.));
#62939=CARTESIAN_POINT('Ctrl Pts',(109.043415355692,-1.58450938593979,-15.9065846443083));
#62940=CARTESIAN_POINT('Ctrl Pts',(109.144875979995,-1.71256291063752,-15.8051240200051));
#62941=CARTESIAN_POINT('Ctrl Pts',(109.249565215576,-1.83253210215195,-15.7004347844244));
#62942=CARTESIAN_POINT('',(108.95,1.44913767461895,-16.));
#62943=CARTESIAN_POINT('',(108.95,0.,-16.));
#62944=CARTESIAN_POINT('',(109.249565208391,1.83253209412259,-15.7004347680384));
#62945=CARTESIAN_POINT('Ctrl Pts',(109.249565215576,1.83253210215195,-15.7004347844244));
#62946=CARTESIAN_POINT('Ctrl Pts',(109.144875979995,1.71256291063752,-15.8051240200051));
#62947=CARTESIAN_POINT('Ctrl Pts',(109.043415355692,1.5845093859398,-15.9065846443082));
#62948=CARTESIAN_POINT('Ctrl Pts',(108.95,1.44913767461895,-16.));
#62949=CARTESIAN_POINT('',(109.450571828096,1.65579187964854,-15.4994281719038));
#62950=CARTESIAN_POINT('Origin',(109.250821963405,1.83142701287898,-16.));
#62951=CARTESIAN_POINT('Ctrl Pts',(109.249565208391,1.83253209412259,-15.7004347680384));
#62952=CARTESIAN_POINT('Ctrl Pts',(109.201898775389,1.87444401393228,-15.6524546953631));
#62953=CARTESIAN_POINT('Ctrl Pts',(109.15164392681,1.91863181623643,-15.5999999999986));
#62954=CARTESIAN_POINT('',(109.732882317017,1.40756322422156,15.5));
#62955=CARTESIAN_POINT('Origin',(109.749178036595,1.83142701287898,-16.));
#62956=CARTESIAN_POINT('',(109.1825212855,1.33317969677524,15.5));
#62957=CARTESIAN_POINT('Origin',(109.5,0.,-16.));
#62958=CARTESIAN_POINT('Origin',(109.5,0.,-15.8));
#62959=CARTESIAN_POINT('Origin',(109.5,0.,-16.));
#62960=CARTESIAN_POINT('Origin',(109.5,0.,-16.));
#62961=CARTESIAN_POINT('Origin',(109.35,0.,15.5));
#62962=CARTESIAN_POINT('Origin',(110.1,0.,19.6));
#62963=CARTESIAN_POINT('',(110.1,-1.22464679914735E-16,20.9));
#62964=CARTESIAN_POINT('Origin',(110.1,0.,21.9));
#62965=CARTESIAN_POINT('Origin',(110.1,1.22464679914735E-16,19.6));
#62966=CARTESIAN_POINT('Ctrl Pts',(110.957496466316,-0.968609346005826,
17.2));
#62967=CARTESIAN_POINT('Ctrl Pts',(110.666585330308,-0.993729619858369,
17.2));
#62968=CARTESIAN_POINT('Ctrl Pts',(110.369405244968,-0.994987437106615,
17.2));
#62969=CARTESIAN_POINT('Ctrl Pts',(109.584606004541,-0.994987437106615,
17.2));
#62970=CARTESIAN_POINT('Ctrl Pts',(108.966168883834,-1.00163012723263,17.2));
#62971=CARTESIAN_POINT('Ctrl Pts',(108.351640706405,-0.750967734840807,
17.2));
#62972=CARTESIAN_POINT('Ctrl Pts',(108.198421877032,-0.660471858983854,
17.2));
#62973=CARTESIAN_POINT('Ctrl Pts',(108.013855167537,-0.484337954844702,
17.2));
#62974=CARTESIAN_POINT('Ctrl Pts',(107.937850648849,-0.38109745127946,17.2));
#62975=CARTESIAN_POINT('Ctrl Pts',(107.858447096036,-0.19916364867032,17.2));
#62976=CARTESIAN_POINT('Ctrl Pts',(107.835049669419,-0.0916730147518283,
17.2));
#62977=CARTESIAN_POINT('Ctrl Pts',(107.835049669419,0.0916730147518283,
17.2));
#62978=CARTESIAN_POINT('Ctrl Pts',(107.858447096036,0.19916364867032,17.2));
#62979=CARTESIAN_POINT('Ctrl Pts',(107.937850648849,0.38109745127946,17.2));
#62980=CARTESIAN_POINT('Ctrl Pts',(108.013855167537,0.484337954844702,17.2));
#62981=CARTESIAN_POINT('Ctrl Pts',(108.198421877032,0.660471858983854,17.2));
#62982=CARTESIAN_POINT('Ctrl Pts',(108.351640706405,0.750967734840807,17.2));
#62983=CARTESIAN_POINT('Ctrl Pts',(108.966168883834,1.00163012723263,17.2));
#62984=CARTESIAN_POINT('Ctrl Pts',(109.584606004541,0.994987437106615,17.2));
#62985=CARTESIAN_POINT('Ctrl Pts',(110.1,0.994987437106615,17.2));
#62986=CARTESIAN_POINT('Ctrl Pts',(110.369405244968,0.994987437106615,17.2));
#62987=CARTESIAN_POINT('Ctrl Pts',(110.666585330308,0.993729619858367,17.2));
#62988=CARTESIAN_POINT('Ctrl Pts',(110.957496466316,0.968609346005826,17.2));
#62989=CARTESIAN_POINT('Origin',(109.5,0.,17.2));
#62990=CARTESIAN_POINT('',(0.,0.,0.));
#62991=CARTESIAN_POINT('Origin',(15.6351280937245,0.,-1.28484844754444E-15));
#62992=CARTESIAN_POINT('',(15.7595726103092,20.5035615807565,-2.51096210609941E-15));
#62993=CARTESIAN_POINT('',(15.7595726103092,-20.5035615807565,-2.51096210609941E-15));
#62994=CARTESIAN_POINT('Origin',(15.7595726103092,0.,-1.25548105304971E-15));
#62995=CARTESIAN_POINT('Origin',(15.7595726103092,0.,-1.25548105304971E-15));
#62996=CARTESIAN_POINT('',(15.5106835771397,21.4627734781028,2.62843168407833E-15));
#62997=CARTESIAN_POINT('',(15.6351280937245,20.9831675294297,2.56969689508887E-15));
#62998=CARTESIAN_POINT('',(15.5106835771397,-21.4627734781028,-2.62843168407833E-15));
#62999=CARTESIAN_POINT('Origin',(15.5106835771397,0.,-1.31421584203917E-15));
#63000=CARTESIAN_POINT('Origin',(15.5106835771397,0.,-1.31421584203917E-15));
#63001=CARTESIAN_POINT('Origin',(15.25,0.,0.));
#63002=CARTESIAN_POINT('',(14.9893164228603,-22.7372265218972,-2.78450716815297E-15));
#63003=CARTESIAN_POINT('',(15.25,-22.1,-2.70646942611565E-15));
#63004=CARTESIAN_POINT('',(14.9893164228603,22.7372265218972,-2.78450716815297E-15));
#63005=CARTESIAN_POINT('Origin',(14.9893164228603,0.,-1.39225358407648E-15));
#63006=CARTESIAN_POINT('Origin',(14.9893164228603,0.,-1.39225358407648E-15));
#63007=CARTESIAN_POINT('Origin',(15.85,0.,0.));
#63008=CARTESIAN_POINT('',(16.,-18.5,-2.2655965784226E-15));
#63009=CARTESIAN_POINT('Origin',(16.,0.,0.));
#63010=CARTESIAN_POINT('',(15.85,-19.75,-2.41867742831602E-15));
#63011=CARTESIAN_POINT('Origin',(14.7178815161335,0.,-1.41724638624665E-15));
#63012=CARTESIAN_POINT('',(14.4464466094067,23.5535533905933,2.88447837683363E-15));
#63013=CARTESIAN_POINT('',(14.7178815161335,23.1453899562452,2.8344927724933E-15));
#63014=CARTESIAN_POINT('',(14.4464466094067,-23.5535533905933,-2.88447837683363E-15));
#63015=CARTESIAN_POINT('Origin',(14.4464466094067,0.,-1.44223918841682E-15));
#63016=CARTESIAN_POINT('Origin',(14.4464466094067,0.,-1.44223918841682E-15));
#63017=CARTESIAN_POINT('Origin',(14.,0.,0.));
#63018=CARTESIAN_POINT('',(13.5535533905933,-24.4464466094067,-2.99382625907366E-15));
#63019=CARTESIAN_POINT('',(14.,-24.,-2.93915231795365E-15));
#63020=CARTESIAN_POINT('',(13.5535533905933,24.4464466094067,-2.99382625907366E-15));
#63021=CARTESIAN_POINT('Origin',(13.5535533905933,0.,-1.49691312953683E-15));
#63022=CARTESIAN_POINT('Origin',(13.5535533905933,0.,-1.49691312953683E-15));
#63023=CARTESIAN_POINT('Origin',(13.1418283394245,0.,-1.51296901209402E-15));
#63024=CARTESIAN_POINT('',(12.7301032882558,24.9708715315434,3.05804978930243E-15));
#63025=CARTESIAN_POINT('',(13.1418283394245,24.708659070475,3.02593802418805E-15));
#63026=CARTESIAN_POINT('',(12.7301032882558,-24.9708715315434,-3.05804978930243E-15));
#63027=CARTESIAN_POINT('Origin',(12.7301032882558,0.,-1.52902489465122E-15));
#63028=CARTESIAN_POINT('Origin',(12.7301032882558,0.,-1.52902489465122E-15));
#63029=CARTESIAN_POINT('Origin',(12.1,0.,0.));
#63030=CARTESIAN_POINT('',(11.4698967117442,-25.4291284684566,-3.11417007840023E-15));
#63031=CARTESIAN_POINT('',(12.1,-25.2,-3.08610993385133E-15));
#63032=CARTESIAN_POINT('',(11.4698967117442,25.4291284684566,-3.11417007840023E-15));
#63033=CARTESIAN_POINT('Origin',(11.4698967117442,0.,-1.55708503920011E-15));
#63034=CARTESIAN_POINT('Origin',(11.4698967117442,0.,-1.55708503920011E-15));
#63035=CARTESIAN_POINT('Origin',(10.9849483558721,0.,-7.78542519600057E-16));
#63036=CARTESIAN_POINT('',(10.5,25.6,3.13509580581722E-15));
#63037=CARTESIAN_POINT('',(10.9849483558721,25.5145642342283,3.12463294210873E-15));
#63038=CARTESIAN_POINT('',(10.5,-25.6,-3.13509580581722E-15));
#63039=CARTESIAN_POINT('Origin',(10.5,0.,0.));
#63040=CARTESIAN_POINT('Origin',(10.5,0.,0.));
#63041=CARTESIAN_POINT('Origin',(6.3,0.,0.));
#63042=CARTESIAN_POINT('',(1.6,-25.6,-3.13509580581722E-15));
#63043=CARTESIAN_POINT('',(6.3,-25.6,-3.13509580581722E-15));
#63044=CARTESIAN_POINT('Origin',(1.6,0.,0.));
#63045=CARTESIAN_POINT('Origin',(-8.,24.52,0.));
#63046=CARTESIAN_POINT('',(-8.,-24.52,-3.00283395150931E-15));
#63047=CARTESIAN_POINT('Origin',(-8.,0.,0.));
#63048=CARTESIAN_POINT('',(-8.,-24.32,-2.97834101552636E-15));
#63049=CARTESIAN_POINT('Origin',(-8.,0.,0.));
#63050=CARTESIAN_POINT('Origin',(-7.7,0.,0.));
#63051=CARTESIAN_POINT('',(-7.4,-25.12,-3.07631275945815E-15));
#63052=CARTESIAN_POINT('Origin',(-7.4,0.,0.));
#63053=CARTESIAN_POINT('',(-7.7,-24.82,-3.03957335548373E-15));
#63054=CARTESIAN_POINT('Origin',(-3.7,0.,0.));
#63055=CARTESIAN_POINT('',(0.,-25.12,-3.07631275945815E-15));
#63056=CARTESIAN_POINT('Origin',(0.,0.,0.));
#63057=CARTESIAN_POINT('',(-3.7,-25.12,-3.07631275945815E-15));
#63058=CARTESIAN_POINT('Origin',(0.,26.8,0.));
#63059=CARTESIAN_POINT('',(0.,-26.8,-3.28205342171491E-15));
#63060=CARTESIAN_POINT('Origin',(0.,0.,0.));
#63061=CARTESIAN_POINT('Origin',(0.599999999999999,0.,0.));
#63062=CARTESIAN_POINT('',(1.2,-26.8,-3.28205342171491E-15));
#63063=CARTESIAN_POINT('Origin',(1.2,0.,0.));
#63064=CARTESIAN_POINT('',(0.599999999999999,-26.8,-3.28205342171491E-15));
#63065=CARTESIAN_POINT('Origin',(1.4,0.,0.));
#63066=CARTESIAN_POINT('',(1.4,-26.2,-3.20857461376607E-15));
#63067=CARTESIAN_POINT('Origin',(16.,0.,0.));
#63068=CARTESIAN_POINT('Origin',(15.2,18.4,0.));
#63069=CARTESIAN_POINT('',(15.2,-18.4,-2.25335011043113E-15));
#63070=CARTESIAN_POINT('Origin',(15.2,0.,0.));
#63071=CARTESIAN_POINT('Origin',(15.05,0.,0.));
#63072=CARTESIAN_POINT('',(14.9,-20.7,-2.53501887423502E-15));
#63073=CARTESIAN_POINT('',(15.05,-19.55,-2.39418449233308E-15));
#63074=CARTESIAN_POINT('Origin',(14.9,0.,0.));
#63075=CARTESIAN_POINT('Origin',(14.5,0.,0.));
#63076=CARTESIAN_POINT('',(14.1,-22.6,-2.76770176607302E-15));
#63077=CARTESIAN_POINT('',(14.5,-21.65,-2.65136032015402E-15));
#63078=CARTESIAN_POINT('Origin',(14.1,0.,0.));
#63079=CARTESIAN_POINT('Origin',(13.35,0.,0.));
#63080=CARTESIAN_POINT('',(12.6,-24.,-2.93915231795365E-15));
#63081=CARTESIAN_POINT('',(13.35,-23.3,-2.85342704201333E-15));
#63082=CARTESIAN_POINT('Origin',(12.6,0.,0.));
#63083=CARTESIAN_POINT('Origin',(11.7,0.,0.));
#63084=CARTESIAN_POINT('',(10.8,-24.8,-3.03712406188544E-15));
#63085=CARTESIAN_POINT('',(11.7,-24.4,-2.98813818991954E-15));
#63086=CARTESIAN_POINT('Origin',(10.8,0.,0.));
#63087=CARTESIAN_POINT('Origin',(1.7,0.,0.));
#63088=CARTESIAN_POINT('',(-7.4,-24.32,-2.97834101552636E-15));
#63089=CARTESIAN_POINT('',(1.7,-24.56,-3.0077325387059E-15));
#63090=CARTESIAN_POINT('Origin',(-7.4,0.,0.));
#63091=CARTESIAN_POINT('Origin',(-7.7,0.,0.));
#63092=CARTESIAN_POINT('',(-7.7,-24.32,-2.97834101552636E-15));
#63093=CARTESIAN_POINT('',(0.,0.,0.));
#63094=CARTESIAN_POINT('Origin',(37.,0.,0.));
#63095=CARTESIAN_POINT('',(19.2762984310705,-6.28301010388654,0.000123638189770958));
#63096=CARTESIAN_POINT('',(19.0900381542954,-6.28269600454591,0.000102748039740536));
#63097=CARTESIAN_POINT('',(37.,-6.28269,-7.69407619853508E-16));
#63098=CARTESIAN_POINT('',(18.8656682926829,2.79354919692123,5.6277438367973));
#63099=CARTESIAN_POINT('Ctrl Pts',(19.2762984310705,-6.28301010388654,0.000123638189770958));
#63100=CARTESIAN_POINT('Ctrl Pts',(19.2719596990827,-6.28312959062582,0.134961570516868));
#63101=CARTESIAN_POINT('Ctrl Pts',(19.2676209670948,-6.27887713223786,0.269791942307153));
#63102=CARTESIAN_POINT('Ctrl Pts',(19.263282235107,-6.27020092921872,0.404337006186821));
#63103=CARTESIAN_POINT('Ctrl Pts',(19.2297589317878,-6.20316406538669,1.44390225225943));
#63104=CARTESIAN_POINT('Ctrl Pts',(19.1962356284685,-5.87203351789313,2.46643486571543));
#63105=CARTESIAN_POINT('Ctrl Pts',(19.1627123251492,-5.31695935551413,3.34796011705817));
#63106=CARTESIAN_POINT('Ctrl Pts',(19.12918902183,-4.76188519313513,4.2294853684009));
#63107=CARTESIAN_POINT('Ctrl Pts',(19.0956657185107,-3.98286741587068,4.97000325763038));
#63108=CARTESIAN_POINT('Ctrl Pts',(19.0621424151914,-3.07436035621313,5.4797127874075));
#63109=CARTESIAN_POINT('Ctrl Pts',(19.0286191118722,-2.16585329655558,5.98942231718462));
#63110=CARTESIAN_POINT('Ctrl Pts',(18.9950958085529,-1.12785695450492,6.26832348750938));
#63111=CARTESIAN_POINT('Ctrl Pts',(18.9615725052336,-0.0862303633136496,
6.28262611703396));
#63112=CARTESIAN_POINT('Ctrl Pts',(18.9296044343834,0.907072484844297,6.29626521070058));
#63113=CARTESIAN_POINT('Ctrl Pts',(18.8976363635331,1.90367656219001,6.06928709268379));
#63114=CARTESIAN_POINT('Ctrl Pts',(18.8656682926829,2.79368235183436,5.62796419942306));
#63115=CARTESIAN_POINT('',(18.8656682926829,-2.79341604200804,5.62752347417158));
#63116=CARTESIAN_POINT('Origin',(18.8656682926829,0.,0.));
#63117=CARTESIAN_POINT('Ctrl Pts',(18.8656682926829,-2.79341604200804,5.62752347417158));
#63118=CARTESIAN_POINT('Ctrl Pts',(18.8991915960022,-3.72675688127093,5.16422744617198));
#63119=CARTESIAN_POINT('Ctrl Pts',(18.9327148993215,-4.54215990698344,4.46450958611088));
#63120=CARTESIAN_POINT('Ctrl Pts',(18.9662382026407,-5.14104950209353,3.61230023328826));
#63121=CARTESIAN_POINT('Ctrl Pts',(18.99976150596,-5.73993909720363,2.76009088046562));
#63122=CARTESIAN_POINT('Ctrl Pts',(19.0332848092793,-6.12231526171131,1.75539003488145));
#63123=CARTESIAN_POINT('Ctrl Pts',(19.0668081125985,-6.24177993240548,0.720486511882419));
#63124=CARTESIAN_POINT('Ctrl Pts',(19.0745514598308,-6.26937436181975,0.481440339905098));
#63125=CARTESIAN_POINT('Ctrl Pts',(19.0822948070631,-6.28294151243645,0.240782745884617));
#63126=CARTESIAN_POINT('Ctrl Pts',(19.0900381542954,-6.28269600454591,0.000102748039740536));
#63127=CARTESIAN_POINT('Origin',(37.,0.,0.));
#63128=CARTESIAN_POINT('',(20.5462984310705,-6.28265148386535,-0.000161171021448303));
#63129=CARTESIAN_POINT('',(20.3600381542954,-6.28297657866995,-0.000130087838368273));
#63130=CARTESIAN_POINT('',(37.,-6.28269,-7.69407619853508E-16));
#63131=CARTESIAN_POINT('Ctrl Pts',(20.5462984310705,-6.28265148386535,-0.000161171021448303));
#63132=CARTESIAN_POINT('Ctrl Pts',(20.5209060055805,-6.28185518498536,0.789107786007277));
#63133=CARTESIAN_POINT('Ctrl Pts',(20.4955135800906,-6.13264436299944,1.57866931564015));
#63134=CARTESIAN_POINT('Ctrl Pts',(20.4701211546007,-5.84225412088425,2.3123523170549));
#63135=CARTESIAN_POINT('Ctrl Pts',(20.4365978512814,-5.45887837085035,3.28096706425059));
#63136=CARTESIAN_POINT('Ctrl Pts',(20.4030745479621,-4.82943377431738,4.15218826095493));
#63137=CARTESIAN_POINT('Ctrl Pts',(20.3695512446428,-4.03024021789354,4.82038071424489));
#63138=CARTESIAN_POINT('Ctrl Pts',(20.3360279413236,-3.2310466614697,5.48857316753485));
#63139=CARTESIAN_POINT('Ctrl Pts',(20.3025046380043,-2.26210414515502,5.95373687741044));
#63140=CARTESIAN_POINT('Ctrl Pts',(20.2689813346851,-1.24089653161339,6.1594709399743));
#63141=CARTESIAN_POINT('Ctrl Pts',(20.2354580313658,-0.219688918071764,
6.36520500253816));
#63142=CARTESIAN_POINT('Ctrl Pts',(20.2019347280465,0.853783792696783,6.31150941779028));
#63143=CARTESIAN_POINT('Ctrl Pts',(20.1684114247272,1.84936349578162,6.00489476066125));
#63144=CARTESIAN_POINT('Ctrl Pts',(20.134888121408,2.84494319886647,5.69828010353222));
#63145=CARTESIAN_POINT('Ctrl Pts',(20.1013648180887,3.76262989426761,5.13874637402203));
#63146=CARTESIAN_POINT('Ctrl Pts',(20.0678415147694,4.49115446665603,4.39413677958182));
#63147=CARTESIAN_POINT('Ctrl Pts',(20.0343182114502,5.21967903904446,3.64952718514161));
#63148=CARTESIAN_POINT('Ctrl Pts',(20.0007949081309,5.75904148842017,2.71984172577137));
#63149=CARTESIAN_POINT('Ctrl Pts',(19.9672716048117,6.04384434700476,1.71780439540296));
#63150=CARTESIAN_POINT('Ctrl Pts',(19.9337483014924,6.32864720558935,0.715767065034549));
#63151=CARTESIAN_POINT('Ctrl Pts',(19.9002249981731,6.35889047338282,-0.358622136332033));
#63152=CARTESIAN_POINT('Ctrl Pts',(19.8667016948538,6.13090717293739,-1.37509404334423));
#63153=CARTESIAN_POINT('Ctrl Pts',(19.8331783915346,5.90292387249196,-2.39156595035644));
#63154=CARTESIAN_POINT('Ctrl Pts',(19.7996550882153,5.41671400380763,-3.35012056301426));
#63155=CARTESIAN_POINT('Ctrl Pts',(19.766131784896,4.73123029292878,-4.13453342405899));
#63156=CARTESIAN_POINT('Ctrl Pts',(19.7326084815768,4.04574658204992,-4.91894628510371));
#63157=CARTESIAN_POINT('Ctrl Pts',(19.6990851782575,3.16098902897655,-5.52921739453534));
#63158=CARTESIAN_POINT('Ctrl Pts',(19.6655618749382,2.18423412824459,-5.89135188379759));
#63159=CARTESIAN_POINT('Ctrl Pts',(19.632038571619,1.20747922751265,-6.25348637305983));
#63160=CARTESIAN_POINT('Ctrl Pts',(19.5985152682997,0.138726979122119,-6.36748424215271));
#63161=CARTESIAN_POINT('Ctrl Pts',(19.5649919649804,-0.892436909941828,
-6.21952282731311));
#63162=CARTESIAN_POINT('Ctrl Pts',(19.5314686616612,-1.92360079900578,-6.07156141247351));
#63163=CARTESIAN_POINT('Ctrl Pts',(19.4979453583419,-2.91717632874314,-5.66164071370144));
#63164=CARTESIAN_POINT('Ctrl Pts',(19.4644220550226,-3.75269280943037,-5.03946436137122));
#63165=CARTESIAN_POINT('Ctrl Pts',(19.4308987517034,-4.5882092901176,-4.417288009041));
#63166=CARTESIAN_POINT('Ctrl Pts',(19.3973754483841,-5.26566672175468,-3.58285600315263));
#63167=CARTESIAN_POINT('Ctrl Pts',(19.3638521450648,-5.70292384748797,-2.63734106086383));
#63168=CARTESIAN_POINT('Ctrl Pts',(19.3346675737334,-6.08358925073353,-1.81419878233041));
#63169=CARTESIAN_POINT('Ctrl Pts',(19.3054830024019,-6.28220637383928,-0.906866529731437));
#63170=CARTESIAN_POINT('Ctrl Pts',(19.2762984310705,-6.28301010388654,0.000123638189770958));
#63171=CARTESIAN_POINT('Ctrl Pts',(19.0900381542954,-6.28269600454591,0.000102748039740536));
#63172=CARTESIAN_POINT('Ctrl Pts',(19.1158181103824,-6.2818786341701,-0.801194105803656));
#63173=CARTESIAN_POINT('Ctrl Pts',(19.1415980664694,-6.12795810464849,-1.60273928956053));
#63174=CARTESIAN_POINT('Ctrl Pts',(19.1673780225563,-5.82885452380126,-2.34589344717355));
#63175=CARTESIAN_POINT('Ctrl Pts',(19.2009013258756,-5.4399112676222,-3.31226368281658));
#63176=CARTESIAN_POINT('Ctrl Pts',(19.2344246291949,-4.80547157838342,-4.17989795368874));
#63177=CARTESIAN_POINT('Ctrl Pts',(19.2679479325141,-4.00244931177914,-4.84349431763947));
#63178=CARTESIAN_POINT('Ctrl Pts',(19.3014712358334,-3.19942704517486,-5.50709068159019));
#63179=CARTESIAN_POINT('Ctrl Pts',(19.3349945391527,-2.22782220120508,-5.96664913861948));
#63180=CARTESIAN_POINT('Ctrl Pts',(19.3685178424719,-1.20544745056172,-6.16650007909134));
#63181=CARTESIAN_POINT('Ctrl Pts',(19.4020411457912,-0.183072699918368,
-6.3663510195632));
#63182=CARTESIAN_POINT('Ctrl Pts',(19.4355644491105,0.890071957398561,-6.30649444347763));
#63183=CARTESIAN_POINT('Ctrl Pts',(19.4690877524297,1.88387126298836,-5.99416156852824));
#63184=CARTESIAN_POINT('Ctrl Pts',(19.502611055749,2.87767056857816,-5.68182869357886));
#63185=CARTESIAN_POINT('Ctrl Pts',(19.5361343590683,3.79212452244082,-5.11701951976566));
#63186=CARTESIAN_POINT('Ctrl Pts',(19.5696576623875,4.516354407704,-4.36823038555468));
#63187=CARTESIAN_POINT('Ctrl Pts',(19.6031809657068,5.24058429296718,-3.61944125134371));
#63188=CARTESIAN_POINT('Ctrl Pts',(19.6367042690261,5.77459010963087,-2.68667215673497));
#63189=CARTESIAN_POINT('Ctrl Pts',(19.6702275723453,6.05362468373747,-1.68301407119577));
#63190=CARTESIAN_POINT('Ctrl Pts',(19.7037508756646,6.33265925784406,-0.67935598565657));
#63191=CARTESIAN_POINT('Ctrl Pts',(19.7372741789839,6.35672258939355,0.395191090813077));
#63192=CARTESIAN_POINT('Ctrl Pts',(19.7707974823031,6.12289660028605,1.41033527152274));
#63193=CARTESIAN_POINT('Ctrl Pts',(19.8043207856224,5.88907061117856,2.4254794522324));
#63194=CARTESIAN_POINT('Ctrl Pts',(19.8378440889417,5.39735530141408,3.38122073718207));
#63195=CARTESIAN_POINT('Ctrl Pts',(19.8713673922609,4.70737114989471,4.16167770349345));
#63196=CARTESIAN_POINT('Ctrl Pts',(19.9048906955802,4.01738699837534,4.94213466980482));
#63197=CARTESIAN_POINT('Ctrl Pts',(19.9384139988995,3.12913400510108,5.5473073174779));
#63198=CARTESIAN_POINT('Ctrl Pts',(19.9719373022187,2.15031235628287,5.90381780552069));
#63199=CARTESIAN_POINT('Ctrl Pts',(20.005460605538,1.17149070746465,6.26032829356348));
#63200=CARTESIAN_POINT('Ctrl Pts',(20.0389839088573,0.10210040310249,6.36817662197599));
#63201=CARTESIAN_POINT('Ctrl Pts',(20.0725072121765,-0.928195388057467,
6.21428669637018));
#63202=CARTESIAN_POINT('Ctrl Pts',(20.1060305154958,-1.95849117921742,6.06039677076437));
#63203=CARTESIAN_POINT('Ctrl Pts',(20.1395538188151,-2.94969245717518,5.64476859114024));
#63204=CARTESIAN_POINT('Ctrl Pts',(20.1730771221343,-3.78161652151487,5.01779665574661));
#63205=CARTESIAN_POINT('Ctrl Pts',(20.2066004254536,-4.61354058585457,4.39082472035299));
#63206=CARTESIAN_POINT('Ctrl Pts',(20.2401237287729,-5.2861874365762,3.55250902918988));
#63207=CARTESIAN_POINT('Ctrl Pts',(20.2736470320921,-5.71799891828659,2.604495121429));
#63208=CARTESIAN_POINT('Ctrl Pts',(20.3024440728266,-6.08893172016407,1.79013637943426));
#63209=CARTESIAN_POINT('Ctrl Pts',(20.331241113561,-6.28215022177013,0.894830466416716));
#63210=CARTESIAN_POINT('Ctrl Pts',(20.3600381542954,-6.28297657866995,-0.000130087838368273));
#63211=CARTESIAN_POINT('Origin',(37.,0.,0.));
#63212=CARTESIAN_POINT('',(21.8162984310705,-6.28226794133467,0.000102037604138849));
#63213=CARTESIAN_POINT('',(21.6300381542954,-6.28215947560979,1.245194739236E-5));
#63214=CARTESIAN_POINT('',(37.,-6.28269,-7.69407619853508E-16));
#63215=CARTESIAN_POINT('Ctrl Pts',(21.8162984310705,-6.28226794133467,0.000102037604138849));
#63216=CARTESIAN_POINT('Ctrl Pts',(21.8033756153977,-6.28250126256899,0.401850367395142));
#63217=CARTESIAN_POINT('Ctrl Pts',(21.7904527997249,-6.24455488198961,0.803555180733288));
#63218=CARTESIAN_POINT('Ctrl Pts',(21.7775299840521,-6.16800368420105,1.19776333277082));
#63219=CARTESIAN_POINT('Ctrl Pts',(21.7440066807328,-5.96942087625138,2.22038563013157));
#63220=CARTESIAN_POINT('Ctrl Pts',(21.7104833774135,-5.51104903483399,3.19255954995002));
#63221=CARTESIAN_POINT('Ctrl Pts',(21.6769600740943,-4.8484655484309,3.99640942288543));
#63222=CARTESIAN_POINT('Ctrl Pts',(21.643436770775,-4.18588206202782,4.80025929582083));
#63223=CARTESIAN_POINT('Ctrl Pts',(21.6099134674557,-3.31908693063903,5.4357851218732));
#63224=CARTESIAN_POINT('Ctrl Pts',(21.5763901641365,-2.35317869086444,5.82592966817379));
#63225=CARTESIAN_POINT('Ctrl Pts',(21.5428668608172,-1.38727045108985,6.21607421447439));
#63226=CARTESIAN_POINT('Ctrl Pts',(21.5093435574979,-0.322249102929453,
6.36083748102322));
#63227=CARTESIAN_POINT('Ctrl Pts',(21.4758202541787,0.712751973552881,6.24266698405807));
#63228=CARTESIAN_POINT('Ctrl Pts',(21.4422969508594,1.74775305003522,6.12449648709291));
#63229=CARTESIAN_POINT('Ctrl Pts',(21.4087736475401,2.75273385483948,5.74339222661377));
#63230=CARTESIAN_POINT('Ctrl Pts',(21.3752503442209,3.60584089794109,5.14556293017366));
#63231=CARTESIAN_POINT('Ctrl Pts',(21.3417270409016,4.4589479410427,4.54773363373354));
#63232=CARTESIAN_POINT('Ctrl Pts',(21.3082037375823,5.16018122244165,3.73317930133244));
#63233=CARTESIAN_POINT('Ctrl Pts',(21.2746804342631,5.62451650858963,2.80066429517295));
#63234=CARTESIAN_POINT('Ctrl Pts',(21.2411571309438,6.0888517947376,1.86814928901346));
#63235=CARTESIAN_POINT('Ctrl Pts',(21.2076338276245,6.31628908563461,0.817673609095557));
#63236=CARTESIAN_POINT('Ctrl Pts',(21.1741105243053,6.27925170765075,-0.223393020520311));
#63237=CARTESIAN_POINT('Ctrl Pts',(21.140587220986,6.24221432966688,-1.26445965013619));
#63238=CARTESIAN_POINT('Ctrl Pts',(21.1070639176667,5.94070228280213,-2.29611722945003));
#63239=CARTESIAN_POINT('Ctrl Pts',(21.0735406143475,5.41127377296556,-3.1932777210302));
#63240=CARTESIAN_POINT('Ctrl Pts',(21.0400173110282,4.881845263129,-4.09043821261036));
#63241=CARTESIAN_POINT('Ctrl Pts',(21.0064940077089,4.12450029032062,-4.85310161645685));
#63242=CARTESIAN_POINT('Ctrl Pts',(20.9729707043897,3.23106660651773,-5.38879532307552));
#63243=CARTESIAN_POINT('Ctrl Pts',(20.9394474010704,2.33763292271485,-5.92448902969418));
#63244=CARTESIAN_POINT('Ctrl Pts',(20.9059240977511,1.30811052791746,-6.23321303908502));
#63245=CARTESIAN_POINT('Ctrl Pts',(20.8724007944319,0.267328569380539,-6.27753469806501));
#63246=CARTESIAN_POINT('Ctrl Pts',(20.8388774911126,-0.773453389156391,
-6.32185635704499));
#63247=CARTESIAN_POINT('Ctrl Pts',(20.8053541877933,-1.82549491143286,-6.10177566561411));
#63248=CARTESIAN_POINT('Ctrl Pts',(20.771830884474,-2.76123641570027,-5.64397731273306));
#63249=CARTESIAN_POINT('Ctrl Pts',(20.7383075811548,-3.69697791996767,-5.186178959852));
#63250=CARTESIAN_POINT('Ctrl Pts',(20.7047842778355,-4.51641940622602,-4.49066294552077));
#63251=CARTESIAN_POINT('Ctrl Pts',(20.6712609745163,-5.1202039469391,-3.64176028740937));
#63252=CARTESIAN_POINT('Ctrl Pts',(20.637737671197,-5.72398848765219,-2.79285762929797));
#63253=CARTESIAN_POINT('Ctrl Pts',(20.6042143678777,-6.11211608282,-1.7905683274064));
#63254=CARTESIAN_POINT('Ctrl Pts',(20.5706910645585,-6.23752642863648,-0.756419527617094));
#63255=CARTESIAN_POINT('Ctrl Pts',(20.5625601867291,-6.26794396209543,-0.505592887164689));
#63256=CARTESIAN_POINT('Ctrl Pts',(20.5544293088998,-6.28290646576581,-0.252892028364329));
#63257=CARTESIAN_POINT('Ctrl Pts',(20.5462984310705,-6.28265148386535,-0.000161171021448303));
#63258=CARTESIAN_POINT('Ctrl Pts',(20.3600381542954,-6.28297657866995,-0.000130087838368273));
#63259=CARTESIAN_POINT('Ctrl Pts',(20.3647644168803,-6.28311220301182,-0.147013881263527));
#63260=CARTESIAN_POINT('Ctrl Pts',(20.3694906794651,-6.27806547058088,-0.293888371957929));
#63261=CARTESIAN_POINT('Ctrl Pts',(20.3742169420499,-6.26777149220422,-0.440394174383335));
#63262=CARTESIAN_POINT('Ctrl Pts',(20.4077402453692,-6.19475647171228,-1.47955743807614));
#63263=CARTESIAN_POINT('Ctrl Pts',(20.4412635486885,-5.85775031802924,-2.50017184110311));
#63264=CARTESIAN_POINT('Ctrl Pts',(20.4747868520078,-5.29761487851413,-3.37848829441954));
#63265=CARTESIAN_POINT('Ctrl Pts',(20.508310155327,-4.73747943899902,-4.25680474773598));
#63266=CARTESIAN_POINT('Ctrl Pts',(20.5418334586463,-3.95421471365185,-4.99282325134187));
#63267=CARTESIAN_POINT('Ctrl Pts',(20.5753567619656,-3.04279121519469,-5.49730189480007));
#63268=CARTESIAN_POINT('Ctrl Pts',(20.6088800652848,-2.13136771673754,-6.00178053825826));
#63269=CARTESIAN_POINT('Ctrl Pts',(20.6424033686041,-1.0917854451704,-6.27471932156876));
#63270=CARTESIAN_POINT('Ctrl Pts',(20.6759266719233,-0.050093302497819,
-6.28302452638716));
#63271=CARTESIAN_POINT('Ctrl Pts',(20.7094499752426,0.991598840174758,-6.29132973120555));
#63272=CARTESIAN_POINT('Ctrl Pts',(20.7429732785619,2.03540085395279,-6.03500135753185));
#63273=CARTESIAN_POINT('Ctrl Pts',(20.7764965818812,2.95475219343646,-5.54511911461026));
#63274=CARTESIAN_POINT('Ctrl Pts',(20.8100198852004,3.87410353292014,-5.05523687168867));
#63275=CARTESIAN_POINT('Ctrl Pts',(20.8435431885197,4.66900419810947,-4.33180075951921));
#63276=CARTESIAN_POINT('Ctrl Pts',(20.8770664918389,5.2430728257406,-3.46252709314663));
#63277=CARTESIAN_POINT('Ctrl Pts',(20.9105897951582,5.81714145337173,-2.59325342677405));
#63278=CARTESIAN_POINT('Ctrl Pts',(20.9441130984775,6.17037804344467,-1.57814220619837));
#63279=CARTESIAN_POINT('Ctrl Pts',(20.9776364017968,6.25995281132153,-0.54027523110904));
#63280=CARTESIAN_POINT('Ctrl Pts',(21.011159705116,6.34952757919838,0.497591743980281));
#63281=CARTESIAN_POINT('Ctrl Pts',(21.0446830084353,6.17544052487916,1.55821447358325));
#63282=CARTESIAN_POINT('Ctrl Pts',(21.0782063117546,5.75879962883674,2.51299290881145));
#63283=CARTESIAN_POINT('Ctrl Pts',(21.1117296150738,5.3421587327943,3.46777134403967));
#63284=CARTESIAN_POINT('Ctrl Pts',(21.1452529183931,4.68296399502866,4.31670548489312));
#63285=CARTESIAN_POINT('Ctrl Pts',(21.1787762217123,3.86114249373319,4.95686243189617));
#63286=CARTESIAN_POINT('Ctrl Pts',(21.2122995250316,3.03932099243774,5.59701937889922));
#63287=CARTESIAN_POINT('Ctrl Pts',(21.2458228283509,2.05487272761245,6.02839913205186));
#63288=CARTESIAN_POINT('Ctrl Pts',(21.2793461316702,1.02716162766404,6.19869708210485));
#63289=CARTESIAN_POINT('Ctrl Pts',(21.3128694349894,-0.000549472284362418,
6.36899503215785));
#63290=CARTESIAN_POINT('Ctrl Pts',(21.3463927383087,-1.07152340735589,6.27821117911118));
#63291=CARTESIAN_POINT('Ctrl Pts',(21.379916041628,-2.05590504889449,5.93735302599625));
#63292=CARTESIAN_POINT('Ctrl Pts',(21.4134393449472,-3.04028669043309,5.59649487288131));
#63293=CARTESIAN_POINT('Ctrl Pts',(21.4469626482665,-3.93807603843877,5.00556241969809));
#63294=CARTESIAN_POINT('Ctrl Pts',(21.4804859515858,-4.64041652088273,4.23620597208803));
#63295=CARTESIAN_POINT('Ctrl Pts',(21.514009254905,-5.34275700332668,3.46684952447795));
#63296=CARTESIAN_POINT('Ctrl Pts',(21.5475325582243,-5.84964862020891,2.51906908244102));
#63297=CARTESIAN_POINT('Ctrl Pts',(21.5810558615436,-6.09963098115819,1.50778261661611));
#63298=CARTESIAN_POINT('Ctrl Pts',(21.5973832924608,-6.22138418936879,1.01523837802827));
#63299=CARTESIAN_POINT('Ctrl Pts',(21.6137107233781,-6.28219467558877,0.507629559776358));
#63300=CARTESIAN_POINT('Ctrl Pts',(21.6300381542954,-6.28215947560979,1.245194739236E-5));
#63301=CARTESIAN_POINT('Origin',(37.,0.,0.));
#63302=CARTESIAN_POINT('',(23.0862984310705,-6.28322123118156,1.47945420200454E-5));
#63303=CARTESIAN_POINT('',(22.9000381542954,-6.2830493926505,0.000112281392144475));
#63304=CARTESIAN_POINT('',(37.,-6.28269,-7.69407619853508E-16));
#63305=CARTESIAN_POINT('Ctrl Pts',(23.0862984310705,-6.28322123118156,1.47945420200454E-5));
#63306=CARTESIAN_POINT('Ctrl Pts',(23.0858452252148,-6.28322315649896,0.0140980318367827));
#63307=CARTESIAN_POINT('Ctrl Pts',(23.0853920193592,-6.28317679231295,0.0281812564013002));
#63308=CARTESIAN_POINT('Ctrl Pts',(23.0849388135035,-6.2830820614407,0.042264155619573));
#63309=CARTESIAN_POINT('Ctrl Pts',(23.0514155101842,-6.27607488859701,1.08396583758096));
#63310=CARTESIAN_POINT('Ctrl Pts',(23.0178922068649,-6.00443171689342,2.12388740320311));
#63311=CARTESIAN_POINT('Ctrl Pts',(22.9843689035457,-5.50108916397988,3.03593881025149));
#63312=CARTESIAN_POINT('Ctrl Pts',(22.9508456002264,-4.99774661106633,3.94799021729987));
#63313=CARTESIAN_POINT('Ctrl Pts',(22.9173222969072,-4.26270467694284,4.73217146577448));
#63314=CARTESIAN_POINT('Ctrl Pts',(22.8837989935879,-3.38508687974927,5.29340091682063));
#63315=CARTESIAN_POINT('Ctrl Pts',(22.8502756902686,-2.5074690825557,5.85463036786677));
#63316=CARTESIAN_POINT('Ctrl Pts',(22.8167523869493,-1.48727542229206,6.19290802148445));
#63317=CARTESIAN_POINT('Ctrl Pts',(22.7832290836301,-0.448203941159331,
6.26721785777208));
#63318=CARTESIAN_POINT('Ctrl Pts',(22.7497057803108,0.590867539973411,6.34152769405972));
#63319=CARTESIAN_POINT('Ctrl Pts',(22.7161824769916,1.64881684197523,6.15186971301729));
#63320=CARTESIAN_POINT('Ctrl Pts',(22.6826591736723,2.59736806733497,5.72123986321468));
#63321=CARTESIAN_POINT('Ctrl Pts',(22.649135870353,3.54591929269469,5.29061001341208));
#63322=CARTESIAN_POINT('Ctrl Pts',(22.6156125670338,4.38507244141232,4.61900829484931));
#63323=CARTESIAN_POINT('Ctrl Pts',(22.5820892637145,5.01308055538941,3.7878661268351));
#63324=CARTESIAN_POINT('Ctrl Pts',(22.5485659603952,5.64108866936651,2.95672395882087));
#63325=CARTESIAN_POINT('Ctrl Pts',(22.515042657076,6.05795174860305,1.96604134135519));
#63326=CARTESIAN_POINT('Ctrl Pts',(22.4815193537567,6.21312532416547,0.935938115401774));
#63327=CARTESIAN_POINT('Ctrl Pts',(22.4479960504374,6.36829889972788,-0.0941651105516532));
#63328=CARTESIAN_POINT('Ctrl Pts',(22.4144727471182,6.26178297161615,-1.16368894499283));
#63329=CARTESIAN_POINT('Ctrl Pts',(22.3809494437989,5.90649255026785,-2.14295408333414));
#63330=CARTESIAN_POINT('Ctrl Pts',(22.3474261404796,5.55120212891955,-3.12221922167544));
#63331=CARTESIAN_POINT('Ctrl Pts',(22.3139028371603,4.94713721433467,-4.0112256639169));
#63332=CARTESIAN_POINT('Ctrl Pts',(22.2803795338411,4.16754041740843,-4.70218176157783));
#63333=CARTESIAN_POINT('Ctrl Pts',(22.2468562305218,3.3879436204822,-5.39313785923877));
#63334=CARTESIAN_POINT('Ctrl Pts',(22.2133329272025,2.43281494121461,-5.88604361231919));
#63335=CARTESIAN_POINT('Ctrl Pts',(22.1798096238833,1.41796332086578,-6.1211344104118));
#63336=CARTESIAN_POINT('Ctrl Pts',(22.146286320564,0.403111700516944,-6.35622520850441));
#63337=CARTESIAN_POINT('Ctrl Pts',(22.1127630172448,-0.671462860913124,
-6.33350105160919));
#63338=CARTESIAN_POINT('Ctrl Pts',(22.0792397139255,-1.67546866036334,-6.05571723396893));
#63339=CARTESIAN_POINT('Ctrl Pts',(22.0457164106062,-2.67947445981354,-5.77793341632867));
#63340=CARTESIAN_POINT('Ctrl Pts',(22.0121931072869,-3.61291149728388,-5.24508993794336));
#63341=CARTESIAN_POINT('Ctrl Pts',(21.9786698039677,-4.36260093374578,-4.5217938412237));
#63342=CARTESIAN_POINT('Ctrl Pts',(21.9451465006484,-5.11229037020769,-3.79849774450404));
#63343=CARTESIAN_POINT('Ctrl Pts',(21.9116231973291,-5.67823220566115,-2.88474902945002));
#63344=CARTESIAN_POINT('Ctrl Pts',(21.8780998940099,-5.99180623614691,-1.89133933447148));
#63345=CARTESIAN_POINT('Ctrl Pts',(21.8574994063634,-6.18450138554061,-1.28087669735034));
#63346=CARTESIAN_POINT('Ctrl Pts',(21.8368989187169,-6.28189599985327,-0.640332037631833));
#63347=CARTESIAN_POINT('Ctrl Pts',(21.8162984310705,-6.28226794133467,0.000102037604138849));
#63348=CARTESIAN_POINT('Ctrl Pts',(21.6300381542954,-6.28215947560979,1.245194739236E-5));
#63349=CARTESIAN_POINT('Ctrl Pts',(21.6472340266974,-6.28212240337534,-0.534604356999154));
#63350=CARTESIAN_POINT('Ctrl Pts',(21.6644298990994,-6.21459485201875,-1.06923036080506));
#63351=CARTESIAN_POINT('Ctrl Pts',(21.6816257715014,-6.07969017924126,-1.58627672545295));
#63352=CARTESIAN_POINT('Ctrl Pts',(21.7151490748206,-5.81669391135876,-2.59425711208423));
#63353=CARTESIAN_POINT('Ctrl Pts',(21.7486723781399,-5.29762827057744,-3.5354253957339));
#63354=CARTESIAN_POINT('Ctrl Pts',(21.7821956814592,-4.58542974242937,-4.29566532710693));
#63355=CARTESIAN_POINT('Ctrl Pts',(21.8157189847784,-3.87323121428129,-5.05590525847996));
#63356=CARTESIAN_POINT('Ctrl Pts',(21.8492422880977,-2.96789979876645,-5.63521683757636));
#63357=CARTESIAN_POINT('Ctrl Pts',(21.882765591417,-1.97920654034809,-5.96335878477205));
#63358=CARTESIAN_POINT('Ctrl Pts',(21.9162888947362,-0.990513281929732,
-6.29150073196775));
#63359=CARTESIAN_POINT('Ctrl Pts',(21.9498121980555,0.0815418193921472,
-6.36847304726274));
#63360=CARTESIAN_POINT('Ctrl Pts',(21.9833355013748,1.10697254401,-6.18494287055884));
#63361=CARTESIAN_POINT('Ctrl Pts',(22.016858804694,2.13240326862785,-6.00141269385496));
#63362=CARTESIAN_POINT('Ctrl Pts',(22.0503821080133,3.11120961654167,-5.55738002515219));
#63363=CARTESIAN_POINT('Ctrl Pts',(22.0839054113326,3.92471173935929,-4.90668363441203));
#63364=CARTESIAN_POINT('Ctrl Pts',(22.1174287146519,4.73821386217691,-4.25598724367186));
#63365=CARTESIAN_POINT('Ctrl Pts',(22.1509520179711,5.38641175989832,-3.39862713089432));
#63366=CARTESIAN_POINT('Ctrl Pts',(22.1844753212904,5.79071171641843,-2.43855784073391));
#63367=CARTESIAN_POINT('Ctrl Pts',(22.2179986246096,6.19501167293854,-1.47848855057352));
#63368=CARTESIAN_POINT('Ctrl Pts',(22.2515219279289,6.35541368825735,-0.415710083030268));
#63369=CARTESIAN_POINT('Ctrl Pts',(22.2850452312482,6.25246908705679,0.620916130141472));
#63370=CARTESIAN_POINT('Ctrl Pts',(22.3185685345674,6.14952448585624,1.65754234331321));
#63371=CARTESIAN_POINT('Ctrl Pts',(22.3520918378867,5.78323326813632,2.66801630211346));
#63372=CARTESIAN_POINT('Ctrl Pts',(22.385615141206,5.19800808638858,3.52981847396006));
#63373=CARTESIAN_POINT('Ctrl Pts',(22.4191384445253,4.61278290464085,4.39162064580665));
#63374=CARTESIAN_POINT('Ctrl Pts',(22.4526617478445,3.80862375886531,5.10475103069959));
#63375=CARTESIAN_POINT('Ctrl Pts',(22.4861850511638,2.8830345993656,5.58274287641222));
#63376=CARTESIAN_POINT('Ctrl Pts',(22.519708354483,1.95744543986588,6.06073472212486));
#63377=CARTESIAN_POINT('Ctrl Pts',(22.5532316578023,0.910426266642013,6.30358802865718));
#63378=CARTESIAN_POINT('Ctrl Pts',(22.5867549611216,-0.131072296204699,
6.28185693711966));
#63379=CARTESIAN_POINT('Ctrl Pts',(22.6202782644409,-1.17257085905141,6.26012584558213));
#63380=CARTESIAN_POINT('Ctrl Pts',(22.6538015677601,-2.20854881152097,5.97381035597475));
#63381=CARTESIAN_POINT('Ctrl Pts',(22.6873248710794,-3.11339427277617,5.45762609817814));
#63382=CARTESIAN_POINT('Ctrl Pts',(22.7208481743987,-4.01823973403137,4.94144184038154));
#63383=CARTESIAN_POINT('Ctrl Pts',(22.7543714777179,-4.79195270407223,4.19538881439572));
#63384=CARTESIAN_POINT('Ctrl Pts',(22.7878947810372,-5.34072081829846,3.30992562850951));
#63385=CARTESIAN_POINT('Ctrl Pts',(22.8214180843564,-5.8894889325247,2.42446244262331));
#63386=CARTESIAN_POINT('Ctrl Pts',(22.8549413876757,-6.2133121909363,1.39958909683672));
#63387=CARTESIAN_POINT('Ctrl Pts',(22.888464690995,-6.27292716282903,0.359571043206212));
#63388=CARTESIAN_POINT('Ctrl Pts',(22.8923225120951,-6.27978758151336,0.239887026580249));
#63389=CARTESIAN_POINT('Ctrl Pts',(22.8961803331953,-6.28314905621492,0.120002446659774));
#63390=CARTESIAN_POINT('Ctrl Pts',(22.9000381542954,-6.2830493926505,0.000112281392144475));
#63391=CARTESIAN_POINT('Origin',(37.,0.,0.));
#63392=CARTESIAN_POINT('',(24.3562984310705,-6.28232352063531,-0.000120941246437023));
#63393=CARTESIAN_POINT('',(24.1700381542954,-6.28260548706583,-0.00016035527560624));
#63394=CARTESIAN_POINT('',(37.,-6.28269,-7.69407619853508E-16));
#63395=CARTESIAN_POINT('Ctrl Pts',(24.3562984310705,-6.28232352063531,-0.000120941246437023));
#63396=CARTESIAN_POINT('Ctrl Pts',(24.3347915317127,-6.28185779185402,0.668474984502739));
#63397=CARTESIAN_POINT('Ctrl Pts',(24.3132846323549,-6.17554954378264,1.33721551995562));
#63398=CARTESIAN_POINT('Ctrl Pts',(24.2917777329971,-5.96582038543131,1.9717742209544));
#63399=CARTESIAN_POINT('Ctrl Pts',(24.2582544296778,-5.6389106773723,2.96087559970648));
#63400=CARTESIAN_POINT('Ctrl Pts',(24.2247311263586,-5.06072765769983,3.86692817607369));
#63401=CARTESIAN_POINT('Ctrl Pts',(24.1912078230393,-4.30137576869091,4.58007346514953));
#63402=CARTESIAN_POINT('Ctrl Pts',(24.1576845197201,-3.54202387968198,5.29321875422537));
#63403=CARTESIAN_POINT('Ctrl Pts',(24.1241612164008,-2.60150312133661,5.81345675600984));
#63404=CARTESIAN_POINT('Ctrl Pts',(24.0906379130815,-1.59385123079055,6.07770883670447));
#63405=CARTESIAN_POINT('Ctrl Pts',(24.0571146097623,-0.586199340244509,
6.34196091739909));
#63406=CARTESIAN_POINT('Ctrl Pts',(24.023591306443,0.48858368250222,6.35022707700387));
#63407=CARTESIAN_POINT('Ctrl Pts',(23.9900680031237,1.50018085854362,6.10150504722461));
#63408=CARTESIAN_POINT('Ctrl Pts',(23.9565446998044,2.51177803458502,5.85278301744535));
#63409=CARTESIAN_POINT('Ctrl Pts',(23.9230213964852,3.46018936392109,5.34707279828205));
#63410=CARTESIAN_POINT('Ctrl Pts',(23.8894980931659,4.23042038107967,4.64569153614333));
#63411=CARTESIAN_POINT('Ctrl Pts',(23.8559747898466,5.00065139823827,3.9443102740046));
#63412=CARTESIAN_POINT('Ctrl Pts',(23.8224514865274,5.59270210321936,3.04725796889044));
#63413=CARTESIAN_POINT('Ctrl Pts',(23.7889281832081,5.93478660287112,2.06330182669177));
#63414=CARTESIAN_POINT('Ctrl Pts',(23.7554048798889,6.27687110252287,1.07934568449311));
#63415=CARTESIAN_POINT('Ctrl Pts',(23.7218815765696,6.36898939684528,0.00848570520994477));
#63416=CARTESIAN_POINT('Ctrl Pts',(23.6883582732503,6.1999721823008,-1.01943679958313));
#63417=CARTESIAN_POINT('Ctrl Pts',(23.654834969931,6.03095496775632,-2.04735930437621));
#63418=CARTESIAN_POINT('Ctrl Pts',(23.6213116666118,5.60080224434495,-3.0323443346792));
#63419=CARTESIAN_POINT('Ctrl Pts',(23.5877883632925,4.96166984463642,-3.85496287951956));
#63420=CARTESIAN_POINT('Ctrl Pts',(23.5542650599732,4.32253744492788,-4.67758142435991));
#63421=CARTESIAN_POINT('Ctrl Pts',(23.520741756654,3.47442536892218,-5.33783348373762));
#63422=CARTESIAN_POINT('Ctrl Pts',(23.4872184533347,2.52016684079541,-5.7556637796351));
#63423=CARTESIAN_POINT('Ctrl Pts',(23.4536951500154,1.56590831266863,-6.17349407553258));
#63424=CARTESIAN_POINT('Ctrl Pts',(23.4201718466962,0.505503332420783,-6.34890260794982));
#63425=CARTESIAN_POINT('Ctrl Pts',(23.3866485433769,-0.532474452506596,
-6.26062116782958));
#63426=CARTESIAN_POINT('Ctrl Pts',(23.3531252400576,-1.57045223743399,-6.17233972770935));
#63427=CARTESIAN_POINT('Ctrl Pts',(23.3196019367384,-2.58600282704091,-5.82036831505163));
#63428=CARTESIAN_POINT('Ctrl Pts',(23.2860786334191,-3.45599114944506,-5.24738331214763));
#63429=CARTESIAN_POINT('Ctrl Pts',(23.2525553300998,-4.32597947184921,-4.67439830924364));
#63430=CARTESIAN_POINT('Ctrl Pts',(23.2190320267806,-5.05040552705059,-3.88039971609336));
#63431=CARTESIAN_POINT('Ctrl Pts',(23.1855087234613,-5.54143296765939,-2.9616595203679));
#63432=CARTESIAN_POINT('Ctrl Pts',(23.1524386259977,-6.02582214505017,-2.05533989168984));
#63433=CARTESIAN_POINT('Ctrl Pts',(23.1193685285341,-6.28308074218897,-1.02762865739354));
#63434=CARTESIAN_POINT('Ctrl Pts',(23.0862984310705,-6.28322123118156,1.47945420200454E-5));
#63435=CARTESIAN_POINT('Ctrl Pts',(22.9000381542954,-6.2830493926505,0.000112281392144475));
#63436=CARTESIAN_POINT('Ctrl Pts',(22.9297036365145,-6.28228300986044,-0.921806976571348));
#63437=CARTESIAN_POINT('Ctrl Pts',(22.9593691187337,-6.07685444261615,-1.84405650430791));
#63438=CARTESIAN_POINT('Ctrl Pts',(22.9890346009528,-5.68395407028917,-2.67797921054549));
#63439=CARTESIAN_POINT('Ctrl Pts',(23.022557904272,-5.2399593204827,-3.62034864919228));
#63440=CARTESIAN_POINT('Ctrl Pts',(23.0560812075913,-4.55656313549588,-4.4499247650114));
#63441=CARTESIAN_POINT('Ctrl Pts',(23.0896045109106,-3.71662700861485,-5.06612181102126));
#63442=CARTESIAN_POINT('Ctrl Pts',(23.1231278142299,-2.87669088173383,-5.68231885703111));
#63443=CARTESIAN_POINT('Ctrl Pts',(23.1566511175491,-1.88021481295859,-6.08513683323169));
#63444=CARTESIAN_POINT('Ctrl Pts',(23.1901744208684,-0.848021096730545,
-6.22573423338731));
#63445=CARTESIAN_POINT('Ctrl Pts',(23.2236977241877,0.184172619497497,-6.36633163354292));
#63446=CARTESIAN_POINT('Ctrl Pts',(23.2572210275069,1.25208398317834,-6.24470845765358));
#63447=CARTESIAN_POINT('Ctrl Pts',(23.2907443308262,2.22622920111004,-5.8756114634475));
#63448=CARTESIAN_POINT('Ctrl Pts',(23.3242676341455,3.20037441904174,-5.50651446924142));
#63449=CARTESIAN_POINT('Ctrl Pts',(23.3577909374647,4.0807534912243,-4.88994365671861));
#63450=CARTESIAN_POINT('Ctrl Pts',(23.391314240784,4.76062083408337,-4.10065797151653));
#63451=CARTESIAN_POINT('Ctrl Pts',(23.4248375441033,5.44048817694244,-3.31137228631445));
#63452=CARTESIAN_POINT('Ctrl Pts',(23.4583608474225,5.91984379047802,-2.34937172843309));
#63453=CARTESIAN_POINT('Ctrl Pts',(23.4918841507418,6.14056601287044,-1.33129845145675));
#63454=CARTESIAN_POINT('Ctrl Pts',(23.5254074540611,6.36128823526285,-0.313225174480436));
#63455=CARTESIAN_POINT('Ctrl Pts',(23.5589307573803,6.32337706651211,0.760920821590882));
#63456=CARTESIAN_POINT('Ctrl Pts',(23.5924540606996,6.03142921951174,1.76089979706136));
#63457=CARTESIAN_POINT('Ctrl Pts',(23.6259773640189,5.73948137251136,2.76087877253185));
#63458=CARTESIAN_POINT('Ctrl Pts',(23.6595006673381,5.19349684726135,3.68669072740151));
#63459=CARTESIAN_POINT('Ctrl Pts',(23.6930239706574,4.4596760324487,4.42608136062515));
#63460=CARTESIAN_POINT('Ctrl Pts',(23.7265472739767,3.72585521763604,5.16547199384878));
#63461=CARTESIAN_POINT('Ctrl Pts',(23.7600705772959,2.80419811326075,5.71844130542639));
#63462=CARTESIAN_POINT('Ctrl Pts',(23.7935938806152,1.80645524653388,6.01794200433511));
#63463=CARTESIAN_POINT('Ctrl Pts',(23.8271171839345,0.808712379806998,6.31744270324383));
#63464=CARTESIAN_POINT('Ctrl Pts',(23.8606404872537,-0.265116249271454,
6.36347478948366));
#63465=CARTESIAN_POINT('Ctrl Pts',(23.894163790573,-1.28482938161696,6.15045689241088));
#63466=CARTESIAN_POINT('Ctrl Pts',(23.9276870938923,-2.30454251396245,5.9374389953381));
#63467=CARTESIAN_POINT('Ctrl Pts',(23.9612103972115,-3.27014014957498,5.46537111495272));
#63468=CARTESIAN_POINT('Ctrl Pts',(23.9947337005308,-4.06454399074362,4.79149127856668));
#63469=CARTESIAN_POINT('Ctrl Pts',(24.0282570038501,-4.85894783191226,4.11761144218065));
#63470=CARTESIAN_POINT('Ctrl Pts',(24.0617803071694,-5.482157878637,3.24191964979396));
#63471=CARTESIAN_POINT('Ctrl Pts',(24.0953036104886,-5.858610180991,2.27059315432319));
#63472=CARTESIAN_POINT('Ctrl Pts',(24.1202151250909,-6.1383557937021,1.54879035508707));
#63473=CARTESIAN_POINT('Ctrl Pts',(24.1451266396931,-6.28183856374847,0.774176826311881));
#63474=CARTESIAN_POINT('Ctrl Pts',(24.1700381542954,-6.28260548706583,-0.00016035527560624));
#63475=CARTESIAN_POINT('Origin',(37.,0.,0.));
#63476=CARTESIAN_POINT('',(25.6262984310704,-6.28256558997173,0.000158582405482416));
#63477=CARTESIAN_POINT('',(25.4400381542954,-6.28229618588959,0.000112427966882737));
#63478=CARTESIAN_POINT('',(37.,-6.28269,-7.69407619853508E-16));
#63479=CARTESIAN_POINT('Ctrl Pts',(25.6262984310704,-6.28256558997173,0.000158582405482416));
#63480=CARTESIAN_POINT('Ctrl Pts',(25.6172611415298,-6.28283770681108,0.281074340762559));
#63481=CARTESIAN_POINT('Ctrl Pts',(25.6082238519892,-6.2643418990228,0.561954538374488));
#63482=CARTESIAN_POINT('Ctrl Pts',(25.5991865624485,-6.22678609035292,0.84026271762793));
#63483=CARTESIAN_POINT('Ctrl Pts',(25.5656632591293,-6.0874749883041,1.8726308261621));
#63484=CARTESIAN_POINT('Ctrl Pts',(25.53213995581,-5.6858990072367,2.86960806101203));
#63485=CARTESIAN_POINT('Ctrl Pts',(25.4986166524908,-5.0707490620111,3.71031136156545));
#63486=CARTESIAN_POINT('Ctrl Pts',(25.4650933491715,-4.45559911678551,4.55101466211884));
#63487=CARTESIAN_POINT('Ctrl Pts',(25.4315700458522,-3.62687520740172,5.23544402837575));
#63488=CARTESIAN_POINT('Ctrl Pts',(25.3980467425329,-2.68505975117786,5.68061269426572));
#63489=CARTESIAN_POINT('Ctrl Pts',(25.3645234392137,-1.74324429495397,6.1257813601557));
#63490=CARTESIAN_POINT('Ctrl Pts',(25.3310001358944,-0.688337291889995,
6.33168932567874));
#63491=CARTESIAN_POINT('Ctrl Pts',(25.2974768325751,0.351754237939646,6.27337033864091));
#63492=CARTESIAN_POINT('Ctrl Pts',(25.2639535292559,1.39184576776926,6.21505135160309));
#63493=CARTESIAN_POINT('Ctrl Pts',(25.2304302259366,2.41712182436454,5.8925054120044));
#63494=CARTESIAN_POINT('Ctrl Pts',(25.1969069226173,3.30326812715684,5.3448410761928));
#63495=CARTESIAN_POINT('Ctrl Pts',(25.163383619298,4.18941442994916,4.79717674038119));
#63496=CARTESIAN_POINT('Ctrl Pts',(25.1298603159788,4.9364309789385,4.02439400835665));
#63497=CARTESIAN_POINT('Ctrl Pts',(25.0963370126595,5.45374233908651,3.12019245376039));
#63498=CARTESIAN_POINT('Ctrl Pts',(25.0628137093403,5.97105369923453,2.21599089916413));
#63499=CARTESIAN_POINT('Ctrl Pts',(25.029290406021,6.25865987054123,1.18037052199615));
#63500=CARTESIAN_POINT('Ctrl Pts',(24.9957671027017,6.28168872852549,0.138899847242213));
#63501=CARTESIAN_POINT('Ctrl Pts',(24.9622437993825,6.30471758650975,-0.90257082751171));
#63502=CARTESIAN_POINT('Ctrl Pts',(24.9287204960632,6.06316913117159,-1.94989179985159));
#63503=CARTESIAN_POINT('Ctrl Pts',(24.8951971927439,5.58633100875483,-2.87607585266319));
#63504=CARTESIAN_POINT('Ctrl Pts',(24.8616738894247,5.10949288633808,-3.80225990547479));
#63505=CARTESIAN_POINT('Ctrl Pts',(24.8281505861054,4.39736509684273,-4.60730703875809));
#63506=CARTESIAN_POINT('Ctrl Pts',(24.7946272827861,3.53629282823508,-5.19360563410635));
#63507=CARTESIAN_POINT('Ctrl Pts',(24.7611039794669,2.67522055962742,-5.77990422945461));
#63508=CARTESIAN_POINT('Ctrl Pts',(24.7275806761476,1.66520381190747,-6.14745428686781));
#63509=CARTESIAN_POINT('Ctrl Pts',(24.6940573728283,0.628706681010569,-6.25169052008341));
#63510=CARTESIAN_POINT('Ctrl Pts',(24.6605340695091,-0.407790449886316,
-6.35592675329901));
#63511=CARTESIAN_POINT('Ctrl Pts',(24.6270107661898,-1.47076796396015,-6.19684916231701));
#63512=CARTESIAN_POINT('Ctrl Pts',(24.5934874628705,-2.43134029515023,-5.79374583657472));
#63513=CARTESIAN_POINT('Ctrl Pts',(24.5599641595512,-3.39191262634031,-5.39064251083242));
#63514=CARTESIAN_POINT('Ctrl Pts',(24.526440856232,-4.25007977464665,-4.74351345032983));
#63515=CARTESIAN_POINT('Ctrl Pts',(24.4929175529127,-4.90178934270455,-3.93082277511924));
#63516=CARTESIAN_POINT('Ctrl Pts',(24.4593942495934,-5.55349891076246,-3.11813209990865));
#63517=CARTESIAN_POINT('Ctrl Pts',(24.4258709462742,-5.99875089857193,-2.13987980999006));
#63518=CARTESIAN_POINT('Ctrl Pts',(24.3923476429549,-6.18355869425389,-1.11467857446229));
#63519=CARTESIAN_POINT('Ctrl Pts',(24.3803312389934,-6.24980291568388,-0.747195929014405));
#63520=CARTESIAN_POINT('Ctrl Pts',(24.368314835032,-6.28258373411747,-0.37368100665398));
#63521=CARTESIAN_POINT('Ctrl Pts',(24.3562984310705,-6.28232352063531,-0.000120941246437023));
#63522=CARTESIAN_POINT('Ctrl Pts',(24.1700381542954,-6.28260548706583,-0.00016035527560624));
#63523=CARTESIAN_POINT('Ctrl Pts',(24.1786499430124,-6.28287060870442,-0.267844930461688));
#63524=CARTESIAN_POINT('Ctrl Pts',(24.1872617317294,-6.26608045776481,-0.535496480747446));
#63525=CARTESIAN_POINT('Ctrl Pts',(24.1958735204464,-6.23196844560772,-0.800921855252021));
#63526=CARTESIAN_POINT('Ctrl Pts',(24.2293968237657,-6.09917984988718,-1.83414917080157));
#63527=CARTESIAN_POINT('Ctrl Pts',(24.2629201270849,-5.70390810046283,-2.83364260334581));
#63528=CARTESIAN_POINT('Ctrl Pts',(24.2964434304042,-5.09407972682174,-3.67821400438507));
#63529=CARTESIAN_POINT('Ctrl Pts',(24.3299667337235,-4.48425135318065,-4.52278540542433));
#63530=CARTESIAN_POINT('Ctrl Pts',(24.3634900370428,-3.65986635532282,-5.21243477495862));
#63531=CARTESIAN_POINT('Ctrl Pts',(24.397013340362,-2.72088105941141,-5.66354242376686));
#63532=CARTESIAN_POINT('Ctrl Pts',(24.4305366436813,-1.78189576349997,-6.11465007257511));
#63533=CARTESIAN_POINT('Ctrl Pts',(24.4640599470005,-0.72831016953494,-6.32721600065731));
#63534=CARTESIAN_POINT('Ctrl Pts',(24.4975832503198,0.312128922693782,-6.27546668072492));
#63535=CARTESIAN_POINT('Ctrl Pts',(24.5311065536391,1.35256801492247,-6.22371736079254));
#63536=CARTESIAN_POINT('Ctrl Pts',(24.5646298569584,2.37986060541485,-5.90765279284559));
#63537=CARTESIAN_POINT('Ctrl Pts',(24.5981531602776,3.26944790973518,-5.36559566970891));
#63538=CARTESIAN_POINT('Ctrl Pts',(24.6316764635969,4.15903521405553,-4.82353854657221));
#63539=CARTESIAN_POINT('Ctrl Pts',(24.6651997669162,4.91091723220384,-4.05548886824577));
#63540=CARTESIAN_POINT('Ctrl Pts',(24.6987230702354,5.43392859310039,-3.15457232764708));
#63541=CARTESIAN_POINT('Ctrl Pts',(24.7322463735547,5.95693995399695,-2.25365578704838));
#63542=CARTESIAN_POINT('Ctrl Pts',(24.7657696768739,6.25108065764178,-1.21987238417744));
#63543=CARTESIAN_POINT('Ctrl Pts',(24.7992929801932,6.2806862703203,-0.178567911677147));
#63544=CARTESIAN_POINT('Ctrl Pts',(24.8328162835125,6.31029188299883,0.862736560823136));
#63545=CARTESIAN_POINT('Ctrl Pts',(24.8663395868318,6.07536240471107,1.91156210295276));
#63546=CARTESIAN_POINT('Ctrl Pts',(24.899862890151,5.60438293358239,2.84073906915807));
#63547=CARTESIAN_POINT('Ctrl Pts',(24.9333861934703,5.13340346245372,3.76991603536338));
#63548=CARTESIAN_POINT('Ctrl Pts',(24.9669094967896,4.42637399848413,4.57944442564439));
#63549=CARTESIAN_POINT('Ctrl Pts',(25.0004328001088,3.56902155986432,5.17116927111213));
#63550=CARTESIAN_POINT('Ctrl Pts',(25.0339561034281,2.7116691212445,5.76289411657988));
#63551=CARTESIAN_POINT('Ctrl Pts',(25.0674794067474,1.70399370797445,6.13681541723436));
#63552=CARTESIAN_POINT('Ctrl Pts',(25.1010027100666,0.668175530195226,6.24759537631232));
#63553=CARTESIAN_POINT('Ctrl Pts',(25.1345260133859,-0.367642647583973,
6.35837533539027));
#63554=CARTESIAN_POINT('Ctrl Pts',(25.1680493167052,-1.43160358987234,6.2060139528917));
#63555=CARTESIAN_POINT('Ctrl Pts',(25.2015726200244,-2.39470249036147,5.80898498086604));
#63556=CARTESIAN_POINT('Ctrl Pts',(25.2350959233437,-3.35780139085063,5.41195600884038));
#63557=CARTESIAN_POINT('Ctrl Pts',(25.268619226663,-4.22003824954055,4.7702594472876));
#63558=CARTESIAN_POINT('Ctrl Pts',(25.3021425299822,-4.87686721843417,3.9617007281006));
#63559=CARTESIAN_POINT('Ctrl Pts',(25.3356658333015,-5.5336961873278,3.1531420089136));
#63560=CARTESIAN_POINT('Ctrl Pts',(25.3691891366208,-5.98511726642513,2.17772113209237));
#63561=CARTESIAN_POINT('Ctrl Pts',(25.40271243994,-6.17639584418372,1.15370745911635));
#63562=CARTESIAN_POINT('Ctrl Pts',(25.4151543447252,-6.2473873520683,0.773653008739074));
#63563=CARTESIAN_POINT('Ctrl Pts',(25.4275962495103,-6.28254517710532,0.386905077530623));
#63564=CARTESIAN_POINT('Ctrl Pts',(25.4400381542954,-6.28229618588959,0.000112427966882737));
#63565=CARTESIAN_POINT('Origin',(37.,0.,0.));
#63566=CARTESIAN_POINT('',(26.8962984310705,-6.28308193949819,-0.000102270523308912));
#63567=CARTESIAN_POINT('',(26.7100381542954,-6.28322420806427,-9.06020636693901E-7));
#63568=CARTESIAN_POINT('',(37.,-6.28269,-7.69407619853508E-16));
#63569=CARTESIAN_POINT('Ctrl Pts',(26.8962984310705,-6.28308193949819,-0.000102270523308912));
#63570=CARTESIAN_POINT('Ctrl Pts',(26.8662074480277,-6.28235777825568,0.935026311892883));
#63571=CARTESIAN_POINT('Ctrl Pts',(26.8361164649849,-6.07079837144568,1.87047159745313));
#63572=CARTESIAN_POINT('Ctrl Pts',(26.8060254819422,-5.66692843813987,2.71382175660999));
#63573=CARTESIAN_POINT('Ctrl Pts',(26.7725021786229,-5.2169911842954,3.65336843574593));
#63574=CARTESIAN_POINT('Ctrl Pts',(26.7389788753036,-4.52836959479689,4.47861214632833));
#63575=CARTESIAN_POINT('Ctrl Pts',(26.7054555719844,-3.68455874097844,5.08949244364578));
#63576=CARTESIAN_POINT('Ctrl Pts',(26.6719322686651,-2.84074788715999,5.70037274096323));
#63577=CARTESIAN_POINT('Ctrl Pts',(26.6384089653458,-1.84174776902159,6.09688962501574));
#63578=CARTESIAN_POINT('Ctrl Pts',(26.6048856620266,-0.808686720903557,
6.23096559427849));
#63579=CARTESIAN_POINT('Ctrl Pts',(26.5713623587073,0.224374327214448,6.36504156354124));
#63580=CARTESIAN_POINT('Ctrl Pts',(26.537839055388,1.29149630531209,6.23667661801425));
#63581=CARTESIAN_POINT('Ctrl Pts',(26.5043157520688,2.26329113284964,5.86143495209256));
#63582=CARTESIAN_POINT('Ctrl Pts',(26.4707924487495,3.23508596038721,5.48619328617085));
#63583=CARTESIAN_POINT('Ctrl Pts',(26.4372691454302,4.11155363736469,4.86407489985442));
#63584=CARTESIAN_POINT('Ctrl Pts',(26.403745842111,4.78642283519279,4.07051137971547));
#63585=CARTESIAN_POINT('Ctrl Pts',(26.3702225387917,5.4612920330209,3.27694785957651));
#63586=CARTESIAN_POINT('Ctrl Pts',(26.3366992354724,5.93456275169962,2.31193920561507));
#63587=CARTESIAN_POINT('Ctrl Pts',(26.3031759321531,6.1488511202917,1.29249230177033));
#63588=CARTESIAN_POINT('Ctrl Pts',(26.2696526288339,6.36313948888378,0.273045397925603));
#63589=CARTESIAN_POINT('Ctrl Pts',(26.2361293255146,6.31844550738921,-0.800839755802381));
#63590=CARTESIAN_POINT('Ctrl Pts',(26.2026060221954,6.02018830182727,-1.79895504673967));
#63591=CARTESIAN_POINT('Ctrl Pts',(26.1690827188761,5.72193109626534,-2.79707033767695));
#63592=CARTESIAN_POINT('Ctrl Pts',(26.1355594155568,5.17011066663604,-3.71941576582354));
#63593=CARTESIAN_POINT('Ctrl Pts',(26.1020361122376,4.43163500252052,-4.45415734500737));
#63594=CARTESIAN_POINT('Ctrl Pts',(26.0685128089183,3.69315933840497,-5.18889892419122));
#63595=CARTESIAN_POINT('Ctrl Pts',(26.034989505599,2.76802843980317,-5.7360366544123));
#63596=CARTESIAN_POINT('Ctrl Pts',(26.0014662022797,1.76841402998099,-6.02923032137723));
#63597=CARTESIAN_POINT('Ctrl Pts',(25.9679428989605,0.768799620158812,-6.32242398834215));
#63598=CARTESIAN_POINT('Ctrl Pts',(25.9344195956412,-0.30529830088375,-6.36167359205092));
#63599=CARTESIAN_POINT('Ctrl Pts',(25.9008962923219,-1.32364582252742,-6.14222013494744));
#63600=CARTESIAN_POINT('Ctrl Pts',(25.8673729890027,-2.34199334417108,-5.92276667784397));
#63601=CARTESIAN_POINT('Ctrl Pts',(25.8338496856834,-3.30459046641586,-5.44461015992825));
#63602=CARTESIAN_POINT('Ctrl Pts',(25.8003263823641,-4.09472270250518,-4.76572685319215));
#63603=CARTESIAN_POINT('Ctrl Pts',(25.7668030790449,-4.88485493859451,-4.08684354645604));
#63604=CARTESIAN_POINT('Ctrl Pts',(25.7332797757256,-5.50252228852838,-3.20723345089954));
#63605=CARTESIAN_POINT('Ctrl Pts',(25.6997564724063,-5.87283285198019,-2.23354891201208));
#63606=CARTESIAN_POINT('Ctrl Pts',(25.6752704586277,-6.14331423839656,-1.52235250012592));
#63607=CARTESIAN_POINT('Ctrl Pts',(25.6507844448491,-6.28182830512015,-0.760966431774124));
#63608=CARTESIAN_POINT('Ctrl Pts',(25.6262984310704,-6.28256558997173,0.000158582405482416));
#63609=CARTESIAN_POINT('Ctrl Pts',(25.4400381542954,-6.28229618588959,0.000112427966882737));
#63610=CARTESIAN_POINT('Ctrl Pts',(25.4611195528296,-6.28187429847437,-0.655263910009739));
#63611=CARTESIAN_POINT('Ctrl Pts',(25.4822009513637,-6.17980133808627,-1.31076863198916));
#63612=CARTESIAN_POINT('Ctrl Pts',(25.5032823498978,-5.97815379453737,-1.93405887555916));
#63613=CARTESIAN_POINT('Ctrl Pts',(25.5368056532171,-5.65749709071257,-2.92520506812781));
#63614=CARTESIAN_POINT('Ctrl Pts',(25.5703289565364,-5.08504760664311,-3.83489098413436));
#63615=CARTESIAN_POINT('Ctrl Pts',(25.6038522598556,-4.33021459588196,-4.55281759780484));
#63616=CARTESIAN_POINT('Ctrl Pts',(25.6373755631749,-3.57538158512081,-5.27074421147534));
#63617=CARTESIAN_POINT('Ctrl Pts',(25.6708988664942,-2.63816504766797,-5.79691152280978));
#63618=CARTESIAN_POINT('Ctrl Pts',(25.7044221698134,-1.63220208529813,-6.06752197177885));
#63619=CARTESIAN_POINT('Ctrl Pts',(25.7379454731327,-0.626239122928279,
-6.33813242074792));
#63620=CARTESIAN_POINT('Ctrl Pts',(25.771468776452,0.448470264358575,-6.35318600735159));
#63621=CARTESIAN_POINT('Ctrl Pts',(25.8049920797712,1.4616180259242,-6.11085749069344));
#63622=CARTESIAN_POINT('Ctrl Pts',(25.8385153830905,2.47476578748983,-5.86852897403529));
#63623=CARTESIAN_POINT('Ctrl Pts',(25.8720386864098,3.42635192333425,-5.36881835411532));
#63624=CARTESIAN_POINT('Ctrl Pts',(25.905561989729,4.20099702406263,-4.67231532851622));
#63625=CARTESIAN_POINT('Ctrl Pts',(25.9390852930483,4.97564212479099,-3.97581230291713));
#63626=CARTESIAN_POINT('Ctrl Pts',(25.9726085963676,5.57334619040331,-3.08251687163894));
#63627=CARTESIAN_POINT('Ctrl Pts',(26.0061318996868,5.92163786020453,-2.10074072123691));
#63628=CARTESIAN_POINT('Ctrl Pts',(26.0396552030061,6.26992953000576,-1.11896457083487));
#63629=CARTESIAN_POINT('Ctrl Pts',(26.0731785063254,6.36880880399585,-0.048707701308994));
#63630=CARTESIAN_POINT('Ctrl Pts',(26.1067018096447,6.20628661276258,0.980261702564567));
#63631=CARTESIAN_POINT('Ctrl Pts',(26.1402251129639,6.0437644215293,2.00923110643813));
#63632=CARTESIAN_POINT('Ctrl Pts',(26.1737484162832,5.61984076507263,2.9969130446594));
#63633=CARTESIAN_POINT('Ctrl Pts',(26.2072717196024,4.98591620427515,3.82355150733151));
#63634=CARTESIAN_POINT('Ctrl Pts',(26.2407950229217,4.35199164347768,4.65018997000362));
#63635=CARTESIAN_POINT('Ctrl Pts',(26.274318326241,3.50806617833942,5.31578495712655));
#63636=CARTESIAN_POINT('Ctrl Pts',(26.3078416295603,2.5564654082707,5.73963336299332));
#63637=CARTESIAN_POINT('Ctrl Pts',(26.3413649328795,1.604864638202,6.16348176886008));
#63638=CARTESIAN_POINT('Ctrl Pts',(26.3748882361988,0.545588563202851,6.34558359347067));
#63639=CARTESIAN_POINT('Ctrl Pts',(26.408411539518,-0.492926048560667,6.26385906897027));
#63640=CARTESIAN_POINT('Ctrl Pts',(26.4419348428373,-1.53144066032422,6.18213454446987));
#63641=CARTESIAN_POINT('Ctrl Pts',(26.4754581461566,-2.54919380885212,5.83658367085848));
#63642=CARTESIAN_POINT('Ctrl Pts',(26.5089814494759,-3.42278336294098,5.26910434283143));
#63643=CARTESIAN_POINT('Ctrl Pts',(26.5425047527951,-4.29637291702982,4.7016250148044));
#63644=CARTESIAN_POINT('Ctrl Pts',(26.5760280561144,-5.0257988766796,3.91221723236171));
#63645=CARTESIAN_POINT('Ctrl Pts',(26.6095513594336,-5.52261865823816,2.99659634935212));
#63646=CARTESIAN_POINT('Ctrl Pts',(26.6430469577209,-6.01902784756412,2.08173217297243));
#63647=CARTESIAN_POINT('Ctrl Pts',(26.6765425560082,-6.2832151704884,1.04086342518149));
#63648=CARTESIAN_POINT('Ctrl Pts',(26.7100381542954,-6.28322420274766,-9.06011619686462E-7));
#63649=CARTESIAN_POINT('Origin',(37.,0.,0.));
#63650=CARTESIAN_POINT('',(28.1662984310705,-6.28216368284996,-2.4584581325704E-5));
#63651=CARTESIAN_POINT('',(27.9800381542954,-6.2822927855414,-0.000111271035758665));
#63652=CARTESIAN_POINT('',(37.,-6.28269,-7.69407619853508E-16));
#63653=CARTESIAN_POINT('Ctrl Pts',(28.1662984310705,-6.28216368284996,-2.4584581325704E-5));
#63654=CARTESIAN_POINT('Ctrl Pts',(28.1486770578448,-6.28208861679347,0.547819922382556));
#63655=CARTESIAN_POINT('Ctrl Pts',(28.1310556846192,-6.21113725184404,1.09568350878778));
#63656=CARTESIAN_POINT('Ctrl Pts',(28.1134343113936,-6.06955109855608,1.62464024068863));
#63657=CARTESIAN_POINT('Ctrl Pts',(28.0799110080743,-5.80019436331722,2.63093962151618));
#63658=CARTESIAN_POINT('Ctrl Pts',(28.046387704755,-5.27519530128862,3.56881107339447));
#63659=CARTESIAN_POINT('Ctrl Pts',(28.0128644014358,-4.55820982277412,4.32453808645659));
#63660=CARTESIAN_POINT('Ctrl Pts',(27.9793410981165,-3.84122434425962,5.0802650995187));
#63661=CARTESIAN_POINT('Ctrl Pts',(27.9458177947972,-2.93225244925926,5.65384767376462));
#63662=CARTESIAN_POINT('Ctrl Pts',(27.912294491478,-1.94150658880723,5.97573916894523));
#63663=CARTESIAN_POINT('Ctrl Pts',(27.8787711881587,-0.950760728355178,
6.29763066412585));
#63664=CARTESIAN_POINT('Ctrl Pts',(27.8452478848394,0.121759097548558,6.36783108024112));
#63665=CARTESIAN_POINT('Ctrl Pts',(27.8117245815202,1.14601032164098,6.17782864705233));
#63666=CARTESIAN_POINT('Ctrl Pts',(27.7782012782009,2.17026154573339,5.98782621386355));
#63667=CARTESIAN_POINT('Ctrl Pts',(27.7446779748816,3.14624416801453,5.53762093137072));
#63668=CARTESIAN_POINT('Ctrl Pts',(27.7111546715624,3.95562071560972,4.8817999963013));
#63669=CARTESIAN_POINT('Ctrl Pts',(27.6776313682431,4.76499726320491,4.22597906123187));
#63670=CARTESIAN_POINT('Ctrl Pts',(27.6441080649238,5.40776773611416,3.36454247358585));
#63671=CARTESIAN_POINT('Ctrl Pts',(27.6105847616046,5.80599649115486,2.40193904884065));
#63672=CARTESIAN_POINT('Ctrl Pts',(27.5770614582853,6.20422524619555,1.43933562409545));
#63673=CARTESIAN_POINT('Ctrl Pts',(27.543538154966,6.35791228336769,0.375565362251069));
#63674=CARTESIAN_POINT('Ctrl Pts',(27.5100148516468,6.24842311556325,-0.660390050305834));
#63675=CARTESIAN_POINT('Ctrl Pts',(27.4764915483275,6.13893394775881,-1.69634546286274));
#63676=CARTESIAN_POINT('Ctrl Pts',(27.4429682450082,5.76626857497779,-2.70448602613216));
#63677=CARTESIAN_POINT('Ctrl Pts',(27.409444941689,5.17561251326937,-3.56257513073585));
#63678=CARTESIAN_POINT('Ctrl Pts',(27.3759216383697,4.58495645156096,-4.42066423533953));
#63679=CARTESIAN_POINT('Ctrl Pts',(27.3423983350504,3.77630970092515,-5.12870188127748));
#63680=CARTESIAN_POINT('Ctrl Pts',(27.3088750317312,2.84772033182337,-5.60083880872927));
#63681=CARTESIAN_POINT('Ctrl Pts',(27.2753517284119,1.91913096272157,-6.07297573618107));
#63682=CARTESIAN_POINT('Ctrl Pts',(27.2418284250926,0.87059897515379,-6.3092119451467));
#63683=CARTESIAN_POINT('Ctrl Pts',(27.2083051217734,-0.170741578690559,
-6.28090389696852));
#63684=CARTESIAN_POINT('Ctrl Pts',(27.1747818184541,-1.21208213253486,-6.25259584879034));
#63685=CARTESIAN_POINT('Ctrl Pts',(27.1412585151348,-2.24623125265574,-5.95974354346838));
#63686=CARTESIAN_POINT('Ctrl Pts',(27.1077352118156,-3.14779880335115,-5.4378551969751));
#63687=CARTESIAN_POINT('Ctrl Pts',(27.0742119084963,-4.04936635404659,-4.9159668504818));
#63688=CARTESIAN_POINT('Ctrl Pts',(27.040688605177,-4.81835233531656,-4.16504246281716));
#63689=CARTESIAN_POINT('Ctrl Pts',(27.0071653018578,-5.36151752791466,-3.2761312927769));
#63690=CARTESIAN_POINT('Ctrl Pts',(26.9736419985385,-5.90468272051275,-2.38722012273665));
#63691=CARTESIAN_POINT('Ctrl Pts',(26.9401186952192,-6.22202712443898,-1.36032217032077));
#63692=CARTESIAN_POINT('Ctrl Pts',(26.9065953919,-6.27507286730687,-0.319948370268094));
#63693=CARTESIAN_POINT('Ctrl Pts',(26.9031630716235,-6.28050401402572,-0.213428554632629));
#63694=CARTESIAN_POINT('Ctrl Pts',(26.899730751347,-6.28316454076491,-0.106767472853189));
#63695=CARTESIAN_POINT('Ctrl Pts',(26.8962984310705,-6.28308193949819,-0.000102270523308912));
#63696=CARTESIAN_POINT('Ctrl Pts',(26.7100381542954,-6.28322420274766,-9.06011619686462E-7));
#63697=CARTESIAN_POINT('Ctrl Pts',(26.7435891626467,-6.28323324994852,-1.04258708610992));
#63698=CARTESIAN_POINT('Ctrl Pts',(26.777140170998,-6.01813621291833,-2.08516881317694));
#63699=CARTESIAN_POINT('Ctrl Pts',(26.8106911793493,-5.52015237330997,-3.00113716792668));
#63700=CARTESIAN_POINT('Ctrl Pts',(26.8442144826685,-5.02257974811507,-3.9163491539757));
#63701=CARTESIAN_POINT('Ctrl Pts',(26.8777377859878,-4.29250482183851,-4.70515678554019));
#63702=CARTESIAN_POINT('Ctrl Pts',(26.911261089307,-3.41844886505665,-5.27191747680705));
#63703=CARTESIAN_POINT('Ctrl Pts',(26.9447843926263,-2.54439290827479,-5.8386781680739));
#63704=CARTESIAN_POINT('Ctrl Pts',(26.9783076959456,-1.52635592098762,-6.18339191904313));
#63705=CARTESIAN_POINT('Ctrl Pts',(27.0118309992649,-0.487774449725965,
-6.26426233577947));
#63706=CARTESIAN_POINT('Ctrl Pts',(27.0453543025841,0.550807021535724,-6.34513275251581));
#63707=CARTESIAN_POINT('Ctrl Pts',(27.0788776059034,1.60993297677191,-6.16215983501923));
#63708=CARTESIAN_POINT('Ctrl Pts',(27.1124009092227,2.56118484977315,-5.73752897078204));
#63709=CARTESIAN_POINT('Ctrl Pts',(27.1459242125419,3.51243672277437,-5.31289810654485));
#63710=CARTESIAN_POINT('Ctrl Pts',(27.1794475158612,4.35581451354066,-4.64660929556708));
#63711=CARTESIAN_POINT('Ctrl Pts',(27.2129708191805,4.98905902794354,-3.81944976939948));
#63712=CARTESIAN_POINT('Ctrl Pts',(27.2464941224997,5.62230354234643,-2.99229024323187));
#63713=CARTESIAN_POINT('Ctrl Pts',(27.280017425819,6.04541478038589,-2.00426000187443));
#63714=CARTESIAN_POINT('Ctrl Pts',(27.3135407291383,6.20709068656277,-0.975157286829399));
#63715=CARTESIAN_POINT('Ctrl Pts',(27.3470640324575,6.36876659273964,0.0539454282156333));
#63716=CARTESIAN_POINT('Ctrl Pts',(27.3805873357768,6.26900716705394,1.1241206169483));
#63717=CARTESIAN_POINT('Ctrl Pts',(27.4141106390961,5.91990819693216,2.10560999835346));
#63718=CARTESIAN_POINT('Ctrl Pts',(27.4476339424153,5.57080922681039,3.08709937975862));
#63719=CARTESIAN_POINT('Ctrl Pts',(27.4811572457346,4.97237071225256,3.97990295383629));
#63720=CARTESIAN_POINT('Ctrl Pts',(27.5146805490539,4.19715306557227,4.67576867150504));
#63721=CARTESIAN_POINT('Ctrl Pts',(27.5482038523731,3.42193541889198,5.37163438917379));
#63722=CARTESIAN_POINT('Ctrl Pts',(27.5817271556924,2.46993864008926,5.8705622504336));
#63723=CARTESIAN_POINT('Ctrl Pts',(27.6152504590117,1.45659192884083,6.11205746685242));
#63724=CARTESIAN_POINT('Ctrl Pts',(27.6487737623309,0.443245217592412,6.35355268327125));
#63725=CARTESIAN_POINT('Ctrl Pts',(27.6822970656502,-0.631451426101716,
6.33761525484909));
#63726=CARTESIAN_POINT('Ctrl Pts',(27.7158203689695,-1.63719149675844,6.06617758792244));
#63727=CARTESIAN_POINT('Ctrl Pts',(27.7493436722887,-2.64293156741516,5.79473992099578));
#63728=CARTESIAN_POINT('Ctrl Pts',(27.782866975608,-3.57971506503448,5.26780201556465));
#63729=CARTESIAN_POINT('Ctrl Pts',(27.8163902789273,-4.33395739373514,4.54925486586091));
#63730=CARTESIAN_POINT('Ctrl Pts',(27.8499135822465,-5.0881997224358,3.83070771615717));
#63731=CARTESIAN_POINT('Ctrl Pts',(27.8834368855658,-5.6599008822178,2.92055132218081));
#63732=CARTESIAN_POINT('Ctrl Pts',(27.9169601888851,-5.97974235352591,1.92914175495713));
#63733=CARTESIAN_POINT('Ctrl Pts',(27.9379861773552,-6.18034857135421,1.30732456913029));
#63734=CARTESIAN_POINT('Ctrl Pts',(27.9590121658253,-6.28187663832541,0.653543498152181));
#63735=CARTESIAN_POINT('Ctrl Pts',(27.9800381542954,-6.2822927855414,-0.000111271035758665));
#63736=CARTESIAN_POINT('Origin',(37.,0.,0.));
#63737=CARTESIAN_POINT('',(29.4362984310705,-6.2829384025201,0.000137440727676699));
#63738=CARTESIAN_POINT('',(29.2500381542954,-6.2826107429555,0.000160513984483283));
#63739=CARTESIAN_POINT('',(37.,-6.28269,-7.69407619853508E-16));
#63740=CARTESIAN_POINT('Ctrl Pts',(29.4362984310705,-6.2829384025201,0.000137440727676699));
#63741=CARTESIAN_POINT('Ctrl Pts',(29.431146667662,-6.28309165294254,0.160247852387589));
#63742=CARTESIAN_POINT('Ctrl Pts',(29.4259949042535,-6.27709430813338,0.320346810608086));
#63743=CARTESIAN_POINT('Ctrl Pts',(29.420843140845,-6.26486526914223,0.479968341813839));
#63744=CARTESIAN_POINT('Ctrl Pts',(29.3873198375257,-6.18528906369617,1.51864977622924));
#63745=CARTESIAN_POINT('Ctrl Pts',(29.3537965342065,-5.84184412917577,2.53711551071983));
#63746=CARTESIAN_POINT('Ctrl Pts',(29.3202732308872,-5.27617301606801,3.41187701334088));
#63747=CARTESIAN_POINT('Ctrl Pts',(29.2867499275679,-4.71050190296023,4.28663851596196));
#63748=CARTESIAN_POINT('Ctrl Pts',(29.2532266242487,-3.92260461126508,5.0176957867135));
#63749=CARTESIAN_POINT('Ctrl Pts',(29.2197033209294,-3.00801334847831,5.51640844617441));
#63750=CARTESIAN_POINT('Ctrl Pts',(29.1861800176101,-2.09342208569153,6.01512110563532));
#63751=CARTESIAN_POINT('Ctrl Pts',(29.1526567142909,-1.05213685181313,6.28148915380559));
#63752=CARTESIAN_POINT('Ctrl Pts',(29.1191334109716,-0.0104130332667599,
6.28321557949322));
#63753=CARTESIAN_POINT('Ctrl Pts',(29.0856101076523,1.03131078527958,6.28494200518084));
#63754=CARTESIAN_POINT('Ctrl Pts',(29.0520868043331,2.07347318849388,6.02202680838582));
#63755=CARTESIAN_POINT('Ctrl Pts',(29.0185635010138,2.98971243354806,5.52634834355709));
#63756=CARTESIAN_POINT('Ctrl Pts',(28.9850401976945,3.90595167860227,5.03066987872835));
#63757=CARTESIAN_POINT('Ctrl Pts',(28.9515168943753,4.69626776549635,4.30222814586588));
#63758=CARTESIAN_POINT('Ctrl Pts',(28.917993591056,5.26483520885776,3.42934639154749));
#63759=CARTESIAN_POINT('Ctrl Pts',(28.8844702877367,5.83340265221916,2.55646463722912));
#63760=CARTESIAN_POINT('Ctrl Pts',(28.8509469844174,6.1802214520479,1.53914286145485));
#63761=CARTESIAN_POINT('Ctrl Pts',(28.8174236810982,6.26323997814055,0.500730891667414));
#63762=CARTESIAN_POINT('Ctrl Pts',(28.7839003777789,6.3462585042332,-0.537681078120038));
#63763=CARTESIAN_POINT('Ctrl Pts',(28.7503770744597,6.16547675658973,-1.5971832419207));
#63764=CARTESIAN_POINT('Ctrl Pts',(28.7168537711404,5.74281444430087,-2.54931141839858));
#63765=CARTESIAN_POINT('Ctrl Pts',(28.6833304678211,5.32015213201201,-3.50143959487647));
#63766=CARTESIAN_POINT('Ctrl Pts',(28.6498071645018,4.65560925507778,-4.34619378403158));
#63767=CARTESIAN_POINT('Ctrl Pts',(28.6162838611826,3.82976135129761,-4.98114790402325));
#63768=CARTESIAN_POINT('Ctrl Pts',(28.5827605578633,3.00391344751746,-5.6161020240149));
#63769=CARTESIAN_POINT('Ctrl Pts',(28.5492372545441,2.01676051689141,-6.04125607484308));
#63770=CARTESIAN_POINT('Ctrl Pts',(28.5157139512248,0.987994427373088,-6.20506031083726));
#63771=CARTESIAN_POINT('Ctrl Pts',(28.4821906479055,-0.0407716621452466,
-6.36886454683144));
#63772=CARTESIAN_POINT('Ctrl Pts',(28.4486673445863,-1.11115091055585,-6.27131896799162));
#63773=CARTESIAN_POINT('Ctrl Pts',(28.415144041267,-2.09336029469551,-5.92425093376711));
#63774=CARTESIAN_POINT('Ctrl Pts',(28.3816207379477,-3.07556967883516,-5.5771828995426));
#63775=CARTESIAN_POINT('Ctrl Pts',(28.3480974346284,-3.96960919870387,-4.9805924099334));
#63776=CARTESIAN_POINT('Ctrl Pts',(28.3145741313092,-4.66707694732499,-4.20681580502353));
#63777=CARTESIAN_POINT('Ctrl Pts',(28.2810508279899,-5.3645446959461,-3.43303920011367));
#63778=CARTESIAN_POINT('Ctrl Pts',(28.2475275246706,-5.86544067331962,-2.48207647990313));
#63779=CARTESIAN_POINT('Ctrl Pts',(28.2140042213514,-6.10903145778184,-1.46923146490945));
#63780=CARTESIAN_POINT('Ctrl Pts',(28.1981022912577,-6.22457984479734,-0.988783864900291));
#63781=CARTESIAN_POINT('Ctrl Pts',(28.1822003611641,-6.28223142417565,-0.494411993574757));
#63782=CARTESIAN_POINT('Ctrl Pts',(28.1662984310705,-6.28216368284996,-2.4584581325704E-5));
#63783=CARTESIAN_POINT('Ctrl Pts',(27.9800381542954,-6.2822927855414,-0.000111271035758665));
#63784=CARTESIAN_POINT('Ctrl Pts',(27.9925354691446,-6.28254013290341,-0.388627105371091));
#63785=CARTESIAN_POINT('Ctrl Pts',(28.0050327839937,-6.24706653565671,-0.777098319653106));
#63786=CARTESIAN_POINT('Ctrl Pts',(28.0175300988429,-6.17544494012033,-1.15878657086317));
#63787=CARTESIAN_POINT('Ctrl Pts',(28.0510534021621,-5.9833242725724,-2.18264258898881));
#63788=CARTESIAN_POINT('Ctrl Pts',(28.0845767054814,-5.53110115464228,-3.1576918847691));
#63789=CARTESIAN_POINT('Ctrl Pts',(28.1181000088007,-4.8736074447357,-3.96571015076587));
#63790=CARTESIAN_POINT('Ctrl Pts',(28.15162331212,-4.21611373482911,-4.77372841676265));
#63791=CARTESIAN_POINT('Ctrl Pts',(28.1851466154392,-3.35334943294606,-5.41471565297589));
#63792=CARTESIAN_POINT('Ctrl Pts',(28.2186699187585,-2.38992433934372,-5.81095243290488));
#63793=CARTESIAN_POINT('Ctrl Pts',(28.2521932220777,-1.42649924574139,-6.20718921283386));
#63794=CARTESIAN_POINT('Ctrl Pts',(28.285716525397,-0.362413360419771,-6.35867553647858));
#63795=CARTESIAN_POINT('Ctrl Pts',(28.3192398287163,0.673313361023692,-6.24704375229898));
#63796=CARTESIAN_POINT('Ctrl Pts',(28.3527631320355,1.70904008246716,-6.13541196811938));
#63797=CARTESIAN_POINT('Ctrl Pts',(28.3862864353548,2.71640764003249,-5.76066207611546));
#63798=CARTESIAN_POINT('Ctrl Pts',(28.4198097386741,3.57327315095031,-5.168232339395));
#63799=CARTESIAN_POINT('Ctrl Pts',(28.4533330419934,4.43013866186816,-4.57580260267451));
#63800=CARTESIAN_POINT('Ctrl Pts',(28.4868563453126,5.13650212613849,-3.76569302123748));
#63801=CARTESIAN_POINT('Ctrl Pts',(28.5203796486319,5.60671727774752,-2.83612903315032));
#63802=CARTESIAN_POINT('Ctrl Pts',(28.5539029519511,6.07693242935653,-1.90656504506317));
#63803=CARTESIAN_POINT('Ctrl Pts',(28.5874262552704,6.31099926830424,-0.857546650325907));
#63804=CARTESIAN_POINT('Ctrl Pts',(28.6209495585897,6.28053729111394,0.183733122212116));
#63805=CARTESIAN_POINT('Ctrl Pts',(28.654472861909,6.25007531392364,1.22501289475014));
#63806=CARTESIAN_POINT('Ctrl Pts',(28.6879961652282,5.95508452059534,2.25855404508894));
#63807=CARTESIAN_POINT('Ctrl Pts',(28.7215194685475,5.43133241785183,3.15904015360085));
#63808=CARTESIAN_POINT('Ctrl Pts',(28.7550427718668,4.90758031510832,4.05952626211275));
#63809=CARTESIAN_POINT('Ctrl Pts',(28.788566075186,4.15506690294963,4.82695732879775));
#63810=CARTESIAN_POINT('Ctrl Pts',(28.8220893785053,3.2650341087074,5.36828266713368));
#63811=CARTESIAN_POINT('Ctrl Pts',(28.8556126818245,2.37500131446517,5.90960800546961));
#63812=CARTESIAN_POINT('Ctrl Pts',(28.8891359851438,1.34744913813939,6.22482761545645));
#63813=CARTESIAN_POINT('Ctrl Pts',(28.9226592884631,0.306967838836412,6.27572125505832));
#63814=CARTESIAN_POINT('Ctrl Pts',(28.9561825917824,-0.73351346046657,6.32661489466019));
#63815=CARTESIAN_POINT('Ctrl Pts',(28.9897058951016,-1.78692388274679,6.1131825638771));
#63816=CARTESIAN_POINT('Ctrl Pts',(29.0232291984209,-2.72553786770569,5.66130284095216));
#63817=CARTESIAN_POINT('Ctrl Pts',(29.0567525017402,-3.6641518526646,5.20942311802722));
#63818=CARTESIAN_POINT('Ctrl Pts',(29.0902758050594,-4.48796940030219,4.51909600296044));
#63819=CARTESIAN_POINT('Ctrl Pts',(29.1237991083787,-5.09710298755033,3.67402336132696));
#63820=CARTESIAN_POINT('Ctrl Pts',(29.157322411698,-5.70623657479846,2.82895071969347));
#63821=CARTESIAN_POINT('Ctrl Pts',(29.1908457150172,-6.10068620165712,1.82913255149328));
#63822=CARTESIAN_POINT('Ctrl Pts',(29.2243690183365,-6.23262502064645,0.795796379284606));
#63823=CARTESIAN_POINT('Ctrl Pts',(29.2329253969895,-6.26630065468368,0.532051023374284));
#63824=CARTESIAN_POINT('Ctrl Pts',(29.2414817756425,-6.28287481385524,0.266122110498242));
#63825=CARTESIAN_POINT('Ctrl Pts',(29.2500381542954,-6.2826107429555,0.000160513984483283));
#63826=CARTESIAN_POINT('Origin',(37.,0.,0.));
#63827=CARTESIAN_POINT('',(30.7062984310705,-6.28273062840727,-0.000159623917656282));
#63828=CARTESIAN_POINT('',(30.5200381542954,-6.2830449876847,-0.000113525223425687));
#63829=CARTESIAN_POINT('',(37.,-6.28269,-7.69407619853508E-16));
#63830=CARTESIAN_POINT('Ctrl Pts',(30.7062984310705,-6.28273062840727,-0.000159623917656282));
#63831=CARTESIAN_POINT('Ctrl Pts',(30.6800929741599,-6.28189621740857,0.814351134667963));
#63832=CARTESIAN_POINT('Ctrl Pts',(30.6538875172492,-6.12272898283887,1.62917848446481));
#63833=CARTESIAN_POINT('Ctrl Pts',(30.6276820603386,-5.81392593643026,2.38268161015097));
#63834=CARTESIAN_POINT('Ctrl Pts',(30.5941587570194,-5.4188899625879,3.34659969486711));
#63835=CARTESIAN_POINT('Ctrl Pts',(30.5606354537001,-4.77897829200318,4.21016204306709));
#63836=CARTESIAN_POINT('Ctrl Pts',(30.5271121503808,-3.97177993930735,4.86866209172127));
#63837=CARTESIAN_POINT('Ctrl Pts',(30.4935888470616,-3.1645815866115,5.52716214037547));
#63838=CARTESIAN_POINT('Ctrl Pts',(30.4600655437423,-2.19009655180453,5.98059988948387));
#63839=CARTESIAN_POINT('Ctrl Pts',(30.426542240423,-1.16648072592444,6.17399620713318));
#63840=CARTESIAN_POINT('Ctrl Pts',(30.3930189371038,-0.142864900044355,
6.36739252478249));
#63841=CARTESIAN_POINT('Ctrl Pts',(30.3594956337845,0.929881716908839,6.3007474109727));
#63842=CARTESIAN_POINT('Ctrl Pts',(30.3259723304652,1.92168905935509,5.98214155706826));
#63843=CARTESIAN_POINT('Ctrl Pts',(30.2924490271459,2.91349640180132,5.66353570316382));
#63844=CARTESIAN_POINT('Ctrl Pts',(30.2589257238267,3.8243644697406,5.09296910916473));
#63845=CARTESIAN_POINT('Ctrl Pts',(30.2254024205074,4.543850901986,4.33962272901333));
#63846=CARTESIAN_POINT('Ctrl Pts',(30.1918791171881,5.26333733423141,3.58627634886191));
#63847=CARTESIAN_POINT('Ctrl Pts',(30.1583558138689,5.79144213078293,2.65015018255818));
#63848=CARTESIAN_POINT('Ctrl Pts',(30.1248325105496,6.06413281236254,1.64474912484432));
#63849=CARTESIAN_POINT('Ctrl Pts',(30.0913092072304,6.33682349394214,0.639348067130484));
#63850=CARTESIAN_POINT('Ctrl Pts',(30.0577859039111,6.35410006054985,-0.435327881993504));
#63851=CARTESIAN_POINT('Ctrl Pts',(30.0242626005918,6.11386773592056,-1.44897472625222));
#63852=CARTESIAN_POINT('Ctrl Pts',(29.9907392972725,5.87363541129127,-2.46262157051093));
#63853=CARTESIAN_POINT('Ctrl Pts',(29.9572159939533,5.375894195425,-3.41523930990441));
#63854=CARTESIAN_POINT('Ctrl Pts',(29.923692690634,4.68099499651056,-4.19132345355154));
#63855=CARTESIAN_POINT('Ctrl Pts',(29.8901693873147,3.98609579759611,-4.96740759719869));
#63856=CARTESIAN_POINT('Ctrl Pts',(29.8566460839955,3.09403861563348,-5.56695814509948));
#63857=CARTESIAN_POINT('Ctrl Pts',(29.8231227806762,2.11298499998145,-5.91727985137609));
#63858=CARTESIAN_POINT('Ctrl Pts',(29.7895994773569,1.13193138432942,-6.26760155765271));
#63859=CARTESIAN_POINT('Ctrl Pts',(29.7560761740377,0.0618813349879865,
-6.36869442230514));
#63860=CARTESIAN_POINT('Ctrl Pts',(29.7225528707184,-0.967422040125088,
-6.20830097900612));
#63861=CARTESIAN_POINT('Ctrl Pts',(29.6890295673991,-1.99672541523813,-6.04790753570709));
#63862=CARTESIAN_POINT('Ctrl Pts',(29.6555062640799,-2.98528211612282,-5.62602778445662));
#63863=CARTESIAN_POINT('Ctrl Pts',(29.6219829607606,-3.81323006828586,-4.99381446351071));
#63864=CARTESIAN_POINT('Ctrl Pts',(29.5884596574413,-4.64117802044892,-4.36160114256479));
#63865=CARTESIAN_POINT('Ctrl Pts',(29.5549363541221,-5.30851722389033,-3.51905425192342));
#63866=CARTESIAN_POINT('Ctrl Pts',(29.5214130508028,-5.73433308742517,-2.56833223943262));
#63867=CARTESIAN_POINT('Ctrl Pts',(29.493041510892,-6.09471081189538,-1.76371441091639));
#63868=CARTESIAN_POINT('Ctrl Pts',(29.4646699709812,-6.28209442927599,-0.881614801049781));
#63869=CARTESIAN_POINT('Ctrl Pts',(29.4362984310705,-6.2829384025201,0.000137440727676699));
#63870=CARTESIAN_POINT('Ctrl Pts',(29.2500381542954,-6.2826107429555,0.000160513984483283));
#63871=CARTESIAN_POINT('Ctrl Pts',(29.2750050789617,-6.28184020222472,-0.775897140030194));
#63872=CARTESIAN_POINT('Ctrl Pts',(29.299972003628,-6.13770353553637,-1.55223307308622));
#63873=CARTESIAN_POINT('Ctrl Pts',(29.3249389282943,-5.85674085145818,-2.27541053968984));
#63874=CARTESIAN_POINT('Ctrl Pts',(29.3584622316136,-5.47948985216053,-3.24642711023853));
#63875=CARTESIAN_POINT('Ctrl Pts',(29.3919855349328,-4.85555984244519,-4.12160607511872));
#63876=CARTESIAN_POINT('Ctrl Pts',(29.4255088382521,-4.06060206744173,-4.79483236152825));
#63877=CARTESIAN_POINT('Ctrl Pts',(29.4590321415714,-3.2656442924383,-5.46805864793777));
#63878=CARTESIAN_POINT('Ctrl Pts',(29.4925554448906,-2.29965875214676,-5.93933225587664));
#63879=CARTESIAN_POINT('Ctrl Pts',(29.5260787482099,-1.27977077755342,-6.1515114632252));
#63880=CARTESIAN_POINT('Ctrl Pts',(29.5596020515292,-0.259882802960086,
-6.36369067057376));
#63881=CARTESIAN_POINT('Ctrl Pts',(29.5931253548484,0.813907605935034,-6.31677547733201));
#63882=CARTESIAN_POINT('Ctrl Pts',(29.6266486581677,1.81140382422821,-6.01645433048753));
#63883=CARTESIAN_POINT('Ctrl Pts',(29.660171961487,2.80890004252139,-5.71613318364305));
#63884=CARTESIAN_POINT('Ctrl Pts',(29.6936952648062,3.73010207021262,-5.16240608319584));
#63885=CARTESIAN_POINT('Ctrl Pts',(29.7272185681255,4.46331455794289,-4.42241220174304));
#63886=CARTESIAN_POINT('Ctrl Pts',(29.7607418714448,5.19652704567314,-3.68241832029027));
#63887=CARTESIAN_POINT('Ctrl Pts',(29.7942651747641,5.74174999344244,-2.75615765783192));
#63888=CARTESIAN_POINT('Ctrl Pts',(29.8277884780833,6.03287535350555,-1.75593892101519));
#63889=CARTESIAN_POINT('Ctrl Pts',(29.8613117814026,6.32400071356866,-0.755720184198445));
#63890=CARTESIAN_POINT('Ctrl Pts',(29.8948350847218,6.36102848592557,0.318456626976721));
#63891=CARTESIAN_POINT('Ctrl Pts',(29.9283583880411,6.13946906911527,1.33634803649634));
#63892=CARTESIAN_POINT('Ctrl Pts',(29.9618816913604,5.91790965230497,2.35423944601598));
#63893=CARTESIAN_POINT('Ctrl Pts',(29.9954049946797,5.43776304632746,3.3158454538801));
#63894=CARTESIAN_POINT('Ctrl Pts',(30.0289282979989,4.75724682049554,4.10457174552421));
#63895=CARTESIAN_POINT('Ctrl Pts',(30.0624516013182,4.07673059466362,4.89329803716833));
#63896=CARTESIAN_POINT('Ctrl Pts',(30.0959749046374,3.1958447489773,5.50914461259242));
#63897=CARTESIAN_POINT('Ctrl Pts',(30.1294982079567,2.22139631308013,5.87744033959552));
#63898=CARTESIAN_POINT('Ctrl Pts',(30.163021511276,1.24694787718298,6.24573606659861));
#63899=CARTESIAN_POINT('Ctrl Pts',(30.1965448145952,0.178936851075004,6.36648094518072));
#63900=CARTESIAN_POINT('Ctrl Pts',(30.2300681179145,-0.85314088801549,6.2250347107841));
#63901=CARTESIAN_POINT('Ctrl Pts',(30.2635914212338,-1.88521862710601,6.08358847638747));
#63902=CARTESIAN_POINT('Ctrl Pts',(30.2971147245531,-2.88136307917904,5.67995112901209));
#63903=CARTESIAN_POINT('Ctrl Pts',(30.3306380278723,-3.72079215817558,5.06306352329593));
#63904=CARTESIAN_POINT('Ctrl Pts',(30.3641613311916,-4.56022123717211,4.44617591757977));
#63905=CARTESIAN_POINT('Ctrl Pts',(30.3976846345109,-5.24293494309215,3.61603805352283));
#63906=CARTESIAN_POINT('Ctrl Pts',(30.4312079378301,-5.68615453294266,2.67330378983877));
#63907=CARTESIAN_POINT('Ctrl Pts',(30.4608180099852,-6.0776363601075,1.84061647066497));
#63908=CARTESIAN_POINT('Ctrl Pts',(30.4904280821403,-6.28227375269624,0.920085612915368));
#63909=CARTESIAN_POINT('Ctrl Pts',(30.5200381542954,-6.2830449876847,-0.000113525223425687));
#63910=CARTESIAN_POINT('Origin',(37.,0.,0.));
#63911=CARTESIAN_POINT('',(31.9762984310705,-6.28222702961327,8.28361765500829E-5));
#63912=CARTESIAN_POINT('',(31.7900381542954,-6.28215913048763,-1.08654762067814E-5));
#63913=CARTESIAN_POINT('',(37.,-6.28269,-7.69407619853508E-16));
#63914=CARTESIAN_POINT('Ctrl Pts',(31.9762984310705,-6.28222702961327,8.28361765500829E-5));
#63915=CARTESIAN_POINT('Ctrl Pts',(31.962562583977,-6.28242667605806,0.427114891079368));
#63916=CARTESIAN_POINT('Ctrl Pts',(31.9488267368835,-6.23951894558398,0.854107376943399));
#63917=CARTESIAN_POINT('Ctrl Pts',(31.9350908897901,-6.15310136954611,1.27210454984562));
#63918=CARTESIAN_POINT('Ctrl Pts',(31.9015675864708,-5.94219318209182,2.29225612247456));
#63919=CARTESIAN_POINT('Ctrl Pts',(31.8680442831515,-5.47212362906995,3.2588281532623));
#63920=CARTESIAN_POINT('Ctrl Pts',(31.8345209798322,-4.79988844145972,4.05462419950228));
#63921=CARTESIAN_POINT('Ctrl Pts',(31.800997676513,-4.12765325384953,4.85042024574221));
#63922=CARTESIAN_POINT('Ctrl Pts',(31.7674743731937,-3.253252431651,5.4754403074344));
#63923=CARTESIAN_POINT('Ctrl Pts',(31.7339510698744,-2.28270669820105,5.85390097111628));
#63924=CARTESIAN_POINT('Ctrl Pts',(31.7004277665552,-1.31216096475108,6.23236163479817));
#63925=CARTESIAN_POINT('Ctrl Pts',(31.6669044632359,-0.245470320049679,
6.36426290046972));
#63926=CARTESIAN_POINT('Ctrl Pts',(31.6333811599166,0.788029454352046,6.23361179644046));
#63927=CARTESIAN_POINT('Ctrl Pts',(31.5998578565974,1.82152922875377,6.10296069241121));
#63928=CARTESIAN_POINT('Ctrl Pts',(31.5663345532781,2.82183813285582,5.70975721868114));
#63929=CARTESIAN_POINT('Ctrl Pts',(31.5328112499588,3.66766914258312,5.10167712719961));
#63930=CARTESIAN_POINT('Ctrl Pts',(31.4992879466396,4.5135001523104,4.49359703571811));
#63931=CARTESIAN_POINT('Ctrl Pts',(31.4657646433203,5.20485326766293,3.67064032648515));
#63932=CARTESIAN_POINT('Ctrl Pts',(31.432241340001,5.65790222097252,2.73259014628289));
#63933=CARTESIAN_POINT('Ctrl Pts',(31.3987180366818,6.11095117428214,1.79453996608057));
#63934=CARTESIAN_POINT('Ctrl Pts',(31.3651947333625,6.32569596554878,0.741396314908916));
#63935=CARTESIAN_POINT('Ctrl Pts',(31.3316714300432,6.27609888126061,-0.299147592815625));
#63936=CARTESIAN_POINT('Ctrl Pts',(31.298148126724,6.22650179697245,-1.33969150054011));
#63937=CARTESIAN_POINT('Ctrl Pts',(31.2646248234047,5.9125628371295,-2.36763566481748));
#63938=CARTESIAN_POINT('Ctrl Pts',(31.2311015200854,5.37234696548889,-3.25834229817102));
#63939=CARTESIAN_POINT('Ctrl Pts',(31.1975782167662,4.83213109384825,-4.14904893152461));
#63940=CARTESIAN_POINT('Ctrl Pts',(31.1640549134469,4.06563831040993,-4.90251803395436));
#63941=CARTESIAN_POINT('Ctrl Pts',(31.1305316101276,3.16580553525635,-5.42739180109455));
#63942=CARTESIAN_POINT('Ctrl Pts',(31.0970083068084,2.26597276010281,-5.95226556823471));
#63943=CARTESIAN_POINT('Ctrl Pts',(31.0634850034891,1.23279999323403,-6.24854400008536));
#63944=CARTESIAN_POINT('Ctrl Pts',(31.0299617001698,0.191558987940454,-6.28030346430707));
#63945=CARTESIAN_POINT('Ctrl Pts',(30.9964383968505,-0.849682017353119,
-6.31206292852878));
#63946=CARTESIAN_POINT('Ctrl Pts',(30.9629150935313,-1.89899126107148,-6.07930342512155));
#63947=CARTESIAN_POINT('Ctrl Pts',(30.929391790212,-2.82914044905153,-5.6102469436905));
#63948=CARTESIAN_POINT('Ctrl Pts',(30.8958684868928,-3.75928963703158,-5.14119046225945));
#63949=CARTESIAN_POINT('Ctrl Pts',(30.8623451835735,-4.57027876927331,-4.43583700280456));
#63950=CARTESIAN_POINT('Ctrl Pts',(30.8288218802542,-5.16377576255377,-3.5797103686905));
#63951=CARTESIAN_POINT('Ctrl Pts',(30.795298576935,-5.75727275583425,-2.72358373457642));
#63952=CARTESIAN_POINT('Ctrl Pts',(30.7617752736157,-6.13327761015345,-1.71668392580315));
#63953=CARTESIAN_POINT('Ctrl Pts',(30.7282519702964,-6.24619989876305,-0.681097110800348));
#63954=CARTESIAN_POINT('Ctrl Pts',(30.7209341238878,-6.27084985513186,-0.455037489442588));
#63955=CARTESIAN_POINT('Ctrl Pts',(30.7136162774791,-6.28296363680513,-0.227610900567938));
#63956=CARTESIAN_POINT('Ctrl Pts',(30.7062984310705,-6.28273062840727,-0.000159623917656282));
#63957=CARTESIAN_POINT('Ctrl Pts',(30.5200381542954,-6.2830449876847,-0.000113525223425687));
#63958=CARTESIAN_POINT('Ctrl Pts',(30.5239513854596,-6.28314691316384,-0.121725925414179));
#63959=CARTESIAN_POINT('Ctrl Pts',(30.5278646166237,-6.27968812365058,-0.243332531808624));
#63960=CARTESIAN_POINT('Ctrl Pts',(30.5317778477879,-6.27262932827603,-0.364729811397658));
#63961=CARTESIAN_POINT('Ctrl Pts',(30.5653011511072,-6.21215905997791,-1.40469848563893));
#63962=CARTESIAN_POINT('Ctrl Pts',(30.5988244544264,-5.88749304960068,-2.42930517081028));
#63963=CARTESIAN_POINT('Ctrl Pts',(30.6323477577457,-5.33799691116167,-3.31431674734011));
#63964=CARTESIAN_POINT('Ctrl Pts',(30.665871061065,-4.78850077272267,-4.19932832386993));
#63965=CARTESIAN_POINT('Ctrl Pts',(30.6993943643842,-4.01417450622188,-4.94474479175823));
#63966=CARTESIAN_POINT('Ctrl Pts',(30.7329176677035,-3.10890483819142,-5.46018472511148));
#63967=CARTESIAN_POINT('Ctrl Pts',(30.7664409710228,-2.20363517016098,-5.97562465846471));
#63968=CARTESIAN_POINT('Ctrl Pts',(30.7999642743421,-1.16742210060086,-6.2610880572829));
#63969=CARTESIAN_POINT('Ctrl Pts',(30.8334875776613,-0.125906018194264,
-6.28196260732688));
#63970=CARTESIAN_POINT('Ctrl Pts',(30.8670108809806,0.915610064212363,-6.30283715737087));
#63971=CARTESIAN_POINT('Ctrl Pts',(30.9005341842998,1.96242915946547,-6.05912285864064));
#63972=CARTESIAN_POINT('Ctrl Pts',(30.9340574876191,2.88762490283157,-5.5803699649591));
#63973=CARTESIAN_POINT('Ctrl Pts',(30.9675807909384,3.81282064619766,-5.10161707127757));
#63974=CARTESIAN_POINT('Ctrl Pts',(31.0011040942577,4.61639303767675,-4.38782558264473));
#63975=CARTESIAN_POINT('Ctrl Pts',(31.0346273975769,5.20090927067106,-3.52554240983122));
#63976=CARTESIAN_POINT('Ctrl Pts',(31.0681507008962,5.78542550366535,-2.66325923701774));
#63977=CARTESIAN_POINT('Ctrl Pts',(31.1016740042154,6.15088557817489,-1.6524843800236));
#63978=CARTESIAN_POINT('Ctrl Pts',(31.1351973075347,6.25297761746464,-0.61577385520735));
#63979=CARTESIAN_POINT('Ctrl Pts',(31.168720610854,6.35506965675439,0.42093666960893));
#63980=CARTESIAN_POINT('Ctrl Pts',(31.2022439141733,6.19379366082435,1.48358286224732));
#63981=CARTESIAN_POINT('Ctrl Pts',(31.2357672174925,5.78870427476552,2.44331932922858));
#63982=CARTESIAN_POINT('Ctrl Pts',(31.2692905208118,5.3836148887067,3.40305579620984));
#63983=CARTESIAN_POINT('Ctrl Pts',(31.3028138241311,4.73471211251909,4.25988253753397));
#63984=CARTESIAN_POINT('Ctrl Pts',(31.3363371274503,3.92067512851839,4.90990967960593));
#63985=CARTESIAN_POINT('Ctrl Pts',(31.3698604307696,3.10663814451772,5.55993682167786));
#63986=CARTESIAN_POINT('Ctrl Pts',(31.4033837340889,2.12746695270396,6.00316436449764));
#63987=CARTESIAN_POINT('Ctrl Pts',(31.4369070374081,1.10188563863521,6.18585115926985));
#63988=CARTESIAN_POINT('Ctrl Pts',(31.4704303407274,0.076304324566436,6.36853795404207));
#63989=CARTESIAN_POINT('Ctrl Pts',(31.5039536440467,-0.995687111757333,
6.29068400076671));
#63990=CARTESIAN_POINT('Ctrl Pts',(31.5374769473659,-1.98411017008232,5.96172905776895));
#63991=CARTESIAN_POINT('Ctrl Pts',(31.5710002506852,-2.97253322840731,5.63277411477118));
#63992=CARTESIAN_POINT('Ctrl Pts',(31.6045235540045,-3.87738790873352,5.05271818205102));
#63993=CARTESIAN_POINT('Ctrl Pts',(31.6380468573237,-4.58896097053383,4.29189279178638));
#63994=CARTESIAN_POINT('Ctrl Pts',(31.671570160643,-5.30053403233411,3.53106740152177));
#63995=CARTESIAN_POINT('Ctrl Pts',(31.7050934639623,-5.81882547560849,2.58947255371271));
#63996=CARTESIAN_POINT('Ctrl Pts',(31.7386167672815,-6.08099268594003,1.5812762183801));
#63997=CARTESIAN_POINT('Ctrl Pts',(31.7557572296195,-6.21503875986478,1.0657855117973));
#63998=CARTESIAN_POINT('Ctrl Pts',(31.7728976919575,-6.28212688791591,0.532883337562788));
#63999=CARTESIAN_POINT('Ctrl Pts',(31.7900381542954,-6.28215913048763,-1.08654762067814E-5));
#64000=CARTESIAN_POINT('Origin',(37.,0.,0.));
#64001=CARTESIAN_POINT('',(33.2462984310705,-6.28320205698061,4.08552788717063E-5));
#64002=CARTESIAN_POINT('',(33.0600381542954,-6.28298144306473,0.000129065751391986));
#64003=CARTESIAN_POINT('',(37.,-6.28269,-7.69407619853508E-16));
#64004=CARTESIAN_POINT('Ctrl Pts',(33.2462984310705,-6.28320205698061,4.08552788717063E-5));
#64005=CARTESIAN_POINT('Ctrl Pts',(33.2450321937941,-6.28321600959046,0.0393891522380337));
#64006=CARTESIAN_POINT('Ctrl Pts',(33.2437659565178,-6.28285406172601,0.0787371917293483));
#64007=CARTESIAN_POINT('Ctrl Pts',(33.2424997192415,-6.28211461241435,0.118078135732937));
#64008=CARTESIAN_POINT('Ctrl Pts',(33.2089764159222,-6.26253788376541,1.15961941977684));
#64009=CARTESIAN_POINT('Ctrl Pts',(33.1754531126029,-5.97836590406743,2.19618739214224));
#64010=CARTESIAN_POINT('Ctrl Pts',(33.1419298092837,-5.4640544035471,3.10209863233354));
#64011=CARTESIAN_POINT('Ctrl Pts',(33.1084065059644,-4.94974290302676,4.00800987252487));
#64012=CARTESIAN_POINT('Ctrl Pts',(33.0748832026451,-4.20529188168404,4.7832643805421));
#64013=CARTESIAN_POINT('Ctrl Pts',(33.0413598993259,-3.32096570543438,5.3338628809688));
#64014=CARTESIAN_POINT('Ctrl Pts',(33.0078365960066,-2.43663952918469,5.88446138139552));
#64015=CARTESIAN_POINT('Ctrl Pts',(32.9743132926873,-1.41243819802804,6.21040387423169));
#64016=CARTESIAN_POINT('Ctrl Pts',(32.940789989368,-0.37254568253624,6.27216997251124));
#64017=CARTESIAN_POINT('Ctrl Pts',(32.9072666860488,0.667346832955501,6.3339360707908));
#64018=CARTESIAN_POINT('Ctrl Pts',(32.8737433827295,1.72293053278239,6.13152577451377));
#64019=CARTESIAN_POINT('Ctrl Pts',(32.8402200794102,2.66621634767878,5.68948124498346));
#64020=CARTESIAN_POINT('Ctrl Pts',(32.806696776091,3.60950216257517,5.24743671545314));
#64021=CARTESIAN_POINT('Ctrl Pts',(32.7731734727717,4.44049009254105,4.56575795266955));
#64022=CARTESIAN_POINT('Ctrl Pts',(32.7396501694525,5.05842320873721,3.72709821321586));
#64023=CARTESIAN_POINT('Ctrl Pts',(32.7061268661332,5.67635632493336,2.88843847376217));
#64024=CARTESIAN_POINT('Ctrl Pts',(32.6726035628139,6.08123462735978,1.89279775763838));
#64025=CARTESIAN_POINT('Ctrl Pts',(32.6390802594947,6.22396679611268,0.86089707313647));
#64026=CARTESIAN_POINT('Ctrl Pts',(32.6055569561754,6.36669896486559,-0.171003611365471));
#64027=CARTESIAN_POINT('Ctrl Pts',(32.5720336528561,6.24728499994497,-1.23916426424554));
#64028=CARTESIAN_POINT('Ctrl Pts',(32.5385103495368,5.88020379319996,-2.21407086609369));
#64029=CARTESIAN_POINT('Ctrl Pts',(32.5049870462176,5.51312258645496,-3.18897746794185));
#64030=CARTESIAN_POINT('Ctrl Pts',(32.4714637428983,4.89837413788557,-4.07063001875808));
#64031=CARTESIAN_POINT('Ctrl Pts',(32.4379404395791,4.11049643228429,-4.75212852623183));
#64032=CARTESIAN_POINT('Ctrl Pts',(32.4044171362598,3.322618726683,-5.43362703370557));
#64033=CARTESIAN_POINT('Ctrl Pts',(32.3708938329405,2.36161176404983,-5.91497149783683));
#64034=CARTESIAN_POINT('Ctrl Pts',(32.3373705296213,1.34399722497286,-6.13779910952724));
#64035=CARTESIAN_POINT('Ctrl Pts',(32.303847226302,0.326382685895892,-6.36062672121764));
#64036=CARTESIAN_POINT('Ctrl Pts',(32.2703239229827,-0.747839429624867,
-6.32493748046721));
#64037=CARTESIAN_POINT('Ctrl Pts',(32.2368006196634,-1.74842015244313,-6.03505869235576));
#64038=CARTESIAN_POINT('Ctrl Pts',(32.2032773163442,-2.74900087526137,-5.74517990424432));
#64039=CARTESIAN_POINT('Ctrl Pts',(32.1697540130249,-3.67594020537711,-5.20111156877187));
#64040=CARTESIAN_POINT('Ctrl Pts',(32.1362307097056,-4.41684714798181,-4.46882173743965));
#64041=CARTESIAN_POINT('Ctrl Pts',(32.1027074063864,-5.1577540905865,-3.73653190610742));
#64042=CARTESIAN_POINT('Ctrl Pts',(32.0691841030671,-5.71262864568015,-2.81602057891541));
#64043=CARTESIAN_POINT('Ctrl Pts',(32.0356607997479,-6.01419251228362,-1.81889935808437));
#64044=CARTESIAN_POINT('Ctrl Pts',(32.0158733435221,-6.1921935211003,-1.23033884777023));
#64045=CARTESIAN_POINT('Ctrl Pts',(31.9960858872963,-6.28193942483286,-0.615086948103771));
#64046=CARTESIAN_POINT('Ctrl Pts',(31.9762984310705,-6.28222702961327,8.28361765500829E-5));
#64047=CARTESIAN_POINT('Ctrl Pts',(31.7900381542954,-6.28215913048763,-1.08654762067814E-5));
#64048=CARTESIAN_POINT('Ctrl Pts',(31.8064209952767,-6.28218994791338,-0.509350743019272));
#64049=CARTESIAN_POINT('Ctrl Pts',(31.822803836258,-6.22096171370733,-1.01868333845915));
#64050=CARTESIAN_POINT('Ctrl Pts',(31.8391866772393,-6.09838890969872,-1.51279847677552));
#64051=CARTESIAN_POINT('Ctrl Pts',(31.8727099805586,-5.84757494573717,-2.5238790137423));
#64052=CARTESIAN_POINT('Ctrl Pts',(31.9062332838779,-5.33990404042537,-3.47124226481969));
#64053=CARTESIAN_POINT('Ctrl Pts',(31.9397565871971,-4.63693107252356,-4.24002084357331));
#64054=CARTESIAN_POINT('Ctrl Pts',(31.9732798905164,-3.93395810462173,-5.00879942232696));
#64055=CARTESIAN_POINT('Ctrl Pts',(32.0068031938357,-3.03568307412986,-5.59899332875682));
#64056=CARTESIAN_POINT('Ctrl Pts',(32.040326497155,-2.05102144186464,-5.93904180573619));
#64057=CARTESIAN_POINT('Ctrl Pts',(32.0738498004742,-1.06635980959946,-6.27909028271555));
#64058=CARTESIAN_POINT('Ctrl Pts',(32.1073731037935,0.00468842443907186,
-6.36899333024443));
#64059=CARTESIAN_POINT('Ctrl Pts',(32.1408964071127,1.0322591228683,-6.19785024250553));
#64060=CARTESIAN_POINT('Ctrl Pts',(32.174419710432,2.05982982129758,-6.02670715476662));
#64061=CARTESIAN_POINT('Ctrl Pts',(32.2079430137513,3.04392298411755,-5.59451793175988));
#64062=CARTESIAN_POINT('Ctrl Pts',(32.2414663170705,3.86521773890408,-4.95368533075446));
#64063=CARTESIAN_POINT('Ctrl Pts',(32.2749896203898,4.68651249369057,-4.31285272974907));
#64064=CARTESIAN_POINT('Ctrl Pts',(32.3085129237091,5.34500884044363,-3.46337675074502));
#64065=CARTESIAN_POINT('Ctrl Pts',(32.3420362270284,5.76086438054576,-2.5082559905699));
#64066=CARTESIAN_POINT('Ctrl Pts',(32.3755595303476,6.17671992064788,-1.55313523039478));
#64067=CARTESIAN_POINT('Ctrl Pts',(32.4090828336669,6.34993465409905,-0.492369689048594));
#64068=CARTESIAN_POINT('Ctrl Pts',(32.4426061369861,6.25950636902242,0.545423268149143));
#64069=CARTESIAN_POINT('Ctrl Pts',(32.4761294403054,6.16907808394578,1.58321622534691));
#64070=CARTESIAN_POINT('Ctrl Pts',(32.5096527436247,5.81500678034133,2.59803659839622));
#64071=CARTESIAN_POINT('Ctrl Pts',(32.543176046944,5.24022345137374,3.46683785385809));
#64072=CARTESIAN_POINT('Ctrl Pts',(32.5766993502632,4.66544012240614,4.33563910931996));
#64073=CARTESIAN_POINT('Ctrl Pts',(32.6102226535825,3.86994476807541,5.05842124719439));
#64074=CARTESIAN_POINT('Ctrl Pts',(32.6437459569018,2.95019085770154,5.54754724435989));
#64075=CARTESIAN_POINT('Ctrl Pts',(32.677269260221,2.03043694732766,6.03667324152539));
#64076=CARTESIAN_POINT('Ctrl Pts',(32.7107925635403,0.98642448091063,6.29214309798196));
#64077=CARTESIAN_POINT('Ctrl Pts',(32.7443158668595,-0.0552604793544102,
6.28298120359215));
#64078=CARTESIAN_POINT('Ctrl Pts',(32.7778391701788,-1.09694543961945,6.27381930920233));
#64079=CARTESIAN_POINT('Ctrl Pts',(32.8113624734981,-2.1363028937325,6.00002566396611));
#64080=CARTESIAN_POINT('Ctrl Pts',(32.8448857768174,-3.04731119773671,5.49479762952369));
#64081=CARTESIAN_POINT('Ctrl Pts',(32.8784090801366,-3.9583195017409,4.98956959508127));
#64082=CARTESIAN_POINT('Ctrl Pts',(32.9119323834559,-4.74097865563625,4.25290717143266));
#64083=CARTESIAN_POINT('Ctrl Pts',(32.9454556867752,-5.30039157388068,3.37413036037516));
#64084=CARTESIAN_POINT('Ctrl Pts',(32.9789789900944,-5.8598044921251,2.49535354931767));
#64085=CARTESIAN_POINT('Ctrl Pts',(33.0125022934137,-6.19597117471861,1.47446235085129));
#64086=CARTESIAN_POINT('Ctrl Pts',(33.0460255967329,-6.26813155608769,0.435239383383873));
#64087=CARTESIAN_POINT('Ctrl Pts',(33.0506964492538,-6.27818577109184,0.290442876575982));
#64088=CARTESIAN_POINT('Ctrl Pts',(33.0553673017746,-6.28311476046551,0.145290490185292));
#64089=CARTESIAN_POINT('Ctrl Pts',(33.0600381542954,-6.28298144306473,0.000129065751391986));
#64090=CARTESIAN_POINT('Origin',(37.,0.,0.));
#64091=CARTESIAN_POINT('',(34.5162984310705,-6.28238146749754,-0.000135238015052663));
#64092=CARTESIAN_POINT('',(34.3300381542954,-6.28268367435609,-0.00016098647794763));
#64093=CARTESIAN_POINT('',(37.,-6.28269,-7.69407619853508E-16));
#64094=CARTESIAN_POINT('Ctrl Pts',(34.5162984310705,-6.28238146749754,-0.000135238015052663));
#64095=CARTESIAN_POINT('Ctrl Pts',(34.493978500292,-6.28183396867322,0.693717463406439));
#64096=CARTESIAN_POINT('Ctrl Pts',(34.4716585695136,-6.16718126832808,1.38774665406166));
#64097=CARTESIAN_POINT('Ctrl Pts',(34.4493386387351,-5.94159291191415,2.04361936738219));
#64098=CARTESIAN_POINT('Ctrl Pts',(34.4158153354158,-5.6027716596253,3.02870395952131));
#64099=CARTESIAN_POINT('Ctrl Pts',(34.3822920320965,-5.01369752830549,3.92771371652569));
#64100=CARTESIAN_POINT('Ctrl Pts',(34.3487687287773,-4.24579550283129,4.6316440923052));
#64101=CARTESIAN_POINT('Ctrl Pts',(34.315245425458,-3.47789347735709,5.33557446808473));
#64102=CARTESIAN_POINT('Ctrl Pts',(34.2817221221387,-2.53116355772858,5.84442546263936));
#64103=CARTESIAN_POINT('Ctrl Pts',(34.2481988188195,-1.52039633921443,6.09649911189622));
#64104=CARTESIAN_POINT('Ctrl Pts',(34.2146755155002,-0.509629120700321,
6.34857276115307));
#64105=CARTESIAN_POINT('Ctrl Pts',(34.181152212181,0.565175396699438,6.34386906511209));
#64106=CARTESIAN_POINT('Ctrl Pts',(34.1476289088617,1.57369762786122,6.08295834489372));
#64107=CARTESIAN_POINT('Ctrl Pts',(34.1141056055424,2.58221985902306,5.82204762467532));
#64108=CARTESIAN_POINT('Ctrl Pts',(34.0805823022231,3.52445980394702,5.3049298802795));
#64109=CARTESIAN_POINT('Ctrl Pts',(34.0470589989039,4.28617127486464,4.59430541563938));
#64110=CARTESIAN_POINT('Ctrl Pts',(34.0135356955846,5.04788274578218,3.88368095099931));
#64111=CARTESIAN_POINT('Ctrl Pts',(33.9800123922653,5.62906574269343,2.97954976611496));
#64112=CARTESIAN_POINT('Ctrl Pts',(33.9464890889461,5.95925207737237,1.99153737800253));
#64113=CARTESIAN_POINT('Ctrl Pts',(33.9129657856268,6.28943841205133,1.00352498989004));
#64114=CARTESIAN_POINT('Ctrl Pts',(33.8794424823075,6.36862808449797,-0.0683686014504739));
#64115=CARTESIAN_POINT('Ctrl Pts',(33.8459191789883,6.18721938101251,-1.09417675942749));
#64116=CARTESIAN_POINT('Ctrl Pts',(33.812395875669,6.00581067752706,-2.11998491740448));
#64117=CARTESIAN_POINT('Ctrl Pts',(33.7788725723497,5.56380359810951,-3.0997076420179));
#64118=CARTESIAN_POINT('Ctrl Pts',(33.7453492690305,4.91479131089306,-3.91455397459509));
#64119=CARTESIAN_POINT('Ctrl Pts',(33.7118259657112,4.26577902367657,-4.72940030717232));
#64120=CARTESIAN_POINT('Ctrl Pts',(33.6783026623919,3.40976152866115,-5.3793702477133));
#64121=CARTESIAN_POINT('Ctrl Pts',(33.6447793590727,2.45053057867523,-5.78565522068381));
#64122=CARTESIAN_POINT('Ctrl Pts',(33.6112560557534,1.49129962868933,-6.1919401936543));
#64123=CARTESIAN_POINT('Ctrl Pts',(33.5777327524341,0.428855223732931,-6.35454019905433));
#64124=CARTESIAN_POINT('Ctrl Pts',(33.5442094491149,-0.607981709384303,
-6.25374005621454));
#64125=CARTESIAN_POINT('Ctrl Pts',(33.5106861457956,-1.64481864250154,-6.15293991337474));
#64126=CARTESIAN_POINT('Ctrl Pts',(33.4771628424763,-2.65604810377963,-5.7887396222951));
#64127=CARTESIAN_POINT('Ctrl Pts',(33.4436395391571,-3.51905895628623,-5.20529831151201));
#64128=CARTESIAN_POINT('Ctrl Pts',(33.4101162358378,-4.38206980879284,-4.62185700072892));
#64129=CARTESIAN_POINT('Ctrl Pts',(33.3765929325185,-5.09686205252798,-3.81917467024236));
#64130=CARTESIAN_POINT('Ctrl Pts',(33.3430696291993,-5.57676743559559,-2.89457620713786));
#64131=CARTESIAN_POINT('Ctrl Pts',(33.3108125631563,-6.03854590320481,-2.00490154102544));
#64132=CARTESIAN_POINT('Ctrl Pts',(33.2785554971134,-6.28284661786531,-1.00234679939667));
#64133=CARTESIAN_POINT('Ctrl Pts',(33.2462984310705,-6.28320205698061,4.08552788717063E-5));
#64134=CARTESIAN_POINT('Ctrl Pts',(33.0600381542954,-6.28298144306473,0.000129065751391986));
#64135=CARTESIAN_POINT('Ctrl Pts',(33.0888906050939,-6.28215792450375,-0.896551537551931));
#64136=CARTESIAN_POINT('Ctrl Pts',(33.1177430558923,-6.08817246169332,-1.79357700458562));
#64137=CARTESIAN_POINT('Ctrl Pts',(33.1465955066908,-5.71585503173087,-2.60919676941154));
#64138=CARTESIAN_POINT('Ctrl Pts',(33.18011881001,-5.2832640458603,-3.55685521827101));
#64139=CARTESIAN_POINT('Ctrl Pts',(33.2136421133293,-4.60992799397454,-4.39461737952143));
#64140=CARTESIAN_POINT('Ctrl Pts',(33.2471654166485,-3.77748858255121,-5.02090495169605));
#64141=CARTESIAN_POINT('Ctrl Pts',(33.2806887199678,-2.94504917112791,-5.64719252387065));
#64142=CARTESIAN_POINT('Ctrl Pts',(33.3142120232871,-1.95350640016708,-6.06200550696946));
#64143=CARTESIAN_POINT('Ctrl Pts',(33.3477353266064,-0.923084403873464,
-6.2150480053332));
#64144=CARTESIAN_POINT('Ctrl Pts',(33.3812586299256,0.107337592420149,-6.36809050369695));
#64145=CARTESIAN_POINT('Ctrl Pts',(33.4147819332449,1.17663881404652,-6.25936251732563));
#64146=CARTESIAN_POINT('Ctrl Pts',(33.4483052365642,2.15516694812606,-5.90204726776868));
#64147=CARTESIAN_POINT('Ctrl Pts',(33.4818285398834,3.13369508220566,-5.5447320182117));
#64148=CARTESIAN_POINT('Ctrl Pts',(33.5153518432027,4.02145012873839,-4.93882950546908));
#64149=CARTESIAN_POINT('Ctrl Pts',(33.548875146522,4.71079217043467,-4.15780514842171));
#64150=CARTESIAN_POINT('Ctrl Pts',(33.5823984498412,5.40013421213092,-3.37678079137438));
#64151=CARTESIAN_POINT('Ctrl Pts',(33.6159217531605,5.89106324899072,-2.42063459002235));
#64152=CARTESIAN_POINT('Ctrl Pts',(33.6494450564798,6.12405434659775,-1.40529885974049));
#64153=CARTESIAN_POINT('Ctrl Pts',(33.682968359799,6.35704544420478,-0.389963129458594));
#64154=CARTESIAN_POINT('Ctrl Pts',(33.7164916631183,6.332098602559,0.684562129753203));
#64155=CARTESIAN_POINT('Ctrl Pts',(33.7500149664376,6.05223861547249,1.6879911927064));
#64156=CARTESIAN_POINT('Ctrl Pts',(33.7835382697568,5.77237862838598,2.69142025565957));
#64157=CARTESIAN_POINT('Ctrl Pts',(33.8170615730761,5.23760549585876,3.62375312235421));
#64158=CARTESIAN_POINT('Ctrl Pts',(33.8505848763954,4.51276023003573,4.37194483399306));
#64159=CARTESIAN_POINT('Ctrl Pts',(33.8841081797146,3.78791496421269,5.1201365456319));
#64160=CARTESIAN_POINT('Ctrl Pts',(33.9176314830339,2.87299756509385,5.68418710221493));
#64161=CARTESIAN_POINT('Ctrl Pts',(33.9511547863532,1.87894137352877,5.99570561653193));
#64162=CARTESIAN_POINT('Ctrl Pts',(33.9846780896725,0.884885181963638,6.30722413084894));
#64163=CARTESIAN_POINT('Ctrl Pts',(34.0182013929917,-0.188309802047724,
6.36621060289987));
#64164=CARTESIAN_POINT('Ctrl Pts',(34.051724696311,-1.21051914861245,6.16551294833717));
#64165=CARTESIAN_POINT('Ctrl Pts',(34.0852479996302,-2.23272849517715,5.96481529377447));
#64166=CARTESIAN_POINT('Ctrl Pts',(34.1187713029495,-3.2039522042952,5.50443351259817));
#64167=CARTESIAN_POINT('Ctrl Pts',(34.1522946062688,-4.00642981926466,4.84018869762095));
#64168=CARTESIAN_POINT('Ctrl Pts',(34.185817909588,-4.80890743423408,4.17594388264377));
#64169=CARTESIAN_POINT('Ctrl Pts',(34.2193412129073,-5.44263895505492,3.30783603386572));
#64170=CARTESIAN_POINT('Ctrl Pts',(34.2528645162266,-5.8307847075948,2.34112285430504));
#64171=CARTESIAN_POINT('Ctrl Pts',(34.2785890622495,-6.12863343627561,1.5993028301337));
#64172=CARTESIAN_POINT('Ctrl Pts',(34.3043136082725,-6.28186993566055,0.799419438509327));
#64173=CARTESIAN_POINT('Ctrl Pts',(34.3300381542954,-6.28268367435609,-0.00016098647794763));
#64174=CARTESIAN_POINT('Origin',(37.,0.,0.));
#64175=CARTESIAN_POINT('',(35.7862984310705,-6.28249223374509,0.000152535273694049));
#64176=CARTESIAN_POINT('',(35.6000381542954,-6.28225017164793,9.44259478526101E-5));
#64177=CARTESIAN_POINT('',(37.,-6.28269,-7.69407619853508E-16));
#64178=CARTESIAN_POINT('Ctrl Pts',(35.7862984310705,-6.28249223374509,0.000152535273694049));
#64179=CARTESIAN_POINT('Ctrl Pts',(35.7764481101091,-6.28277209891908,0.306350889573917));
#64180=CARTESIAN_POINT('Ctrl Pts',(35.7665977891478,-6.26078533904793,0.612509400593861));
#64181=CARTESIAN_POINT('Ctrl Pts',(35.7567474681865,-6.21619340497281,0.915339282244856));
#64182=CARTESIAN_POINT('Ctrl Pts',(35.7232241648672,-6.06443500669699,1.94595117972385));
#64183=CARTESIAN_POINT('Ctrl Pts',(35.689700861548,-5.65085788080548,2.93801006724945));
#64184=CARTESIAN_POINT('Ctrl Pts',(35.6561775582287,-5.0256080758031,3.77122923170559));
#64185=CARTESIAN_POINT('Ctrl Pts',(35.6226542549094,-4.40035827080072,4.60444839616172));
#64186=CARTESIAN_POINT('Ctrl Pts',(35.5891309515902,-3.56343578668749,5.27882783754836));
#64187=CARTESIAN_POINT('Ctrl Pts',(35.5556076482709,-2.61631711443867,5.71259933885997));
#64188=CARTESIAN_POINT('Ctrl Pts',(35.5220843449516,-1.66919844218988,6.14637084017157));
#64189=CARTESIAN_POINT('Ctrl Pts',(35.4885610416324,-0.611883581805538,
6.33953440140814));
#64190=CARTESIAN_POINT('Ctrl Pts',(35.4550377383131,0.427428494976258,6.26866902391013));
#64191=CARTESIAN_POINT('Ctrl Pts',(35.4215144349938,1.46674057175808,6.19780364641211));
#64192=CARTESIAN_POINT('Ctrl Pts',(35.3879911316745,2.48804986493734,5.8629093301795));
#64193=CARTESIAN_POINT('Ctrl Pts',(35.3544678283553,3.36752306230223,5.30459186691217));
#64194=CARTESIAN_POINT('Ctrl Pts',(35.320944525036,4.24699625966712,4.74627440364483));
#64195=CARTESIAN_POINT('Ctrl Pts',(35.2874212217168,4.98463336121762,3.96453379334279));
#64196=CARTESIAN_POINT('Ctrl Pts',(35.2538979183975,5.49099618588033,3.05415574853278));
#64197=CARTESIAN_POINT('Ctrl Pts',(35.2203746150782,5.99735901054301,2.14377770372282));
#64198=CARTESIAN_POINT('Ctrl Pts',(35.186851311759,6.27244755831792,1.10476222440484));
#64199=CARTESIAN_POINT('Ctrl Pts',(35.1533280084397,6.2829074611894,0.0630894902391272));
#64200=CARTESIAN_POINT('Ctrl Pts',(35.1198047051204,6.29336736406087,-0.978583243926678));
#64201=CARTESIAN_POINT('Ctrl Pts',(35.0862814018011,6.03919862202889,-2.0229132329403));
#64202=CARTESIAN_POINT('Ctrl Pts',(35.0527580984819,5.55121908566695,-2.94327591512843));
#64203=CARTESIAN_POINT('Ctrl Pts',(35.0192347951626,5.06323954930503,-3.86363859731651));
#64204=CARTESIAN_POINT('Ctrl Pts',(34.9857114918434,4.3414492186132,-4.6600339726791));
#64205=CARTESIAN_POINT('Ctrl Pts',(34.9521881885241,3.4733648605189,-5.2358994447335));
#64206=CARTESIAN_POINT('Ctrl Pts',(34.9186648852048,2.6052805024246,-5.81176491678791));
#64207=CARTESIAN_POINT('Ctrl Pts',(34.8851415818855,1.59090211692786,-6.1671004855341));
#64208=CARTESIAN_POINT('Ctrl Pts',(34.8516182785663,0.553222646667127,-6.25882186620315));
#64209=CARTESIAN_POINT('Ctrl Pts',(34.818094975247,-0.484456823593634,-6.3505432468722));
#64210=CARTESIAN_POINT('Ctrl Pts',(34.7845716719278,-1.54543737861837,-6.17865043946409));
#64211=CARTESIAN_POINT('Ctrl Pts',(34.7510483686085,-2.50107558277158,-5.76398537289191));
#64212=CARTESIAN_POINT('Ctrl Pts',(34.7175250652892,-3.45671378692479,-5.34932030631973));
#64213=CARTESIAN_POINT('Ctrl Pts',(34.68400176197,-4.30700964020647,-4.6918829805835));
#64214=CARTESIAN_POINT('Ctrl Pts',(34.6504784586507,-4.94886513638575,-3.87138738845827));
#64215=CARTESIAN_POINT('Ctrl Pts',(34.6169551553314,-5.590720632565,-3.05089179633308));
#64216=CARTESIAN_POINT('Ctrl Pts',(34.5834318520122,-6.02413577164186,-2.06733793781892));
#64217=CARTESIAN_POINT('Ctrl Pts',(34.5499085486929,-6.19655915455137,-1.03998129492494));
#64218=CARTESIAN_POINT('Ctrl Pts',(34.5387051761521,-6.25418245542611,-0.696642242296477));
#64219=CARTESIAN_POINT('Ctrl Pts',(34.5275018036113,-6.28265628166948,-0.348410973259297));
#64220=CARTESIAN_POINT('Ctrl Pts',(34.5162984310705,-6.28238146749754,-0.000135238015052663));
#64221=CARTESIAN_POINT('Ctrl Pts',(34.3300381542954,-6.28268367435609,-0.00016098647794763));
#64222=CARTESIAN_POINT('Ctrl Pts',(34.3378369115917,-6.28293037066643,-0.242565018323604));
#64223=CARTESIAN_POINT('Ctrl Pts',(34.345635668888,-6.26916812957207,-0.484941204979767));
#64224=CARTESIAN_POINT('Ctrl Pts',(34.3534344261844,-6.24117932363999,-0.725663265874277));
#64225=CARTESIAN_POINT('Ctrl Pts',(34.3869577295036,-6.12086820288638,-1.7604176961495));
#64226=CARTESIAN_POINT('Ctrl Pts',(34.4204810328229,-5.73768597712025,-2.76460804635658));
#64227=CARTESIAN_POINT('Ctrl Pts',(34.4540043361422,-5.13809332628862,-3.61647666875083));
#64228=CARTESIAN_POINT('Ctrl Pts',(34.4875276394615,-4.538500675457,-4.46834529114505));
#64229=CARTESIAN_POINT('Ctrl Pts',(34.5210509427807,-3.72249759955989,-5.16789218572647));
#64230=CARTESIAN_POINT('Ctrl Pts',(34.5545742461,-2.78902412033039,-5.63029759262208));
#64231=CARTESIAN_POINT('Ctrl Pts',(34.5880975494192,-1.85555064110086,-6.09270299951771));
#64232=CARTESIAN_POINT('Ctrl Pts',(34.6216208527385,-0.804606758538935,
-6.31796691872752));
#64233=CARTESIAN_POINT('Ctrl Pts',(34.6551441560578,0.236381033936069,-6.27877619700416));
#64234=CARTESIAN_POINT('Ctrl Pts',(34.688667459377,1.2773688264111,-6.23958547528079));
#64235=CARTESIAN_POINT('Ctrl Pts',(34.7221907626963,2.30840052879923,-5.93594011262423));
#64236=CARTESIAN_POINT('Ctrl Pts',(34.7557140660156,3.20446399095668,-5.40465697856327));
#64237=CARTESIAN_POINT('Ctrl Pts',(34.7892373693349,4.10052745311406,-4.87337384450235));
#64238=CARTESIAN_POINT('Ctrl Pts',(34.8227606726541,4.86162267504081,-4.11445293903707));
#64239=CARTESIAN_POINT('Ctrl Pts',(34.8562839759734,5.3954671886646,-3.21991309530465));
#64240=CARTESIAN_POINT('Ctrl Pts',(34.8898072792927,5.92931170228845,-2.32537325157215));
#64241=CARTESIAN_POINT('Ctrl Pts',(34.9233305826119,6.23590550760931,-1.29521446957246));
#64242=CARTESIAN_POINT('Ctrl Pts',(34.9568538859312,6.27807423769439,-0.254343058227982));
#64243=CARTESIAN_POINT('Ctrl Pts',(34.9903771892504,6.32024296777946,0.786528353116469));
#64244=CARTESIAN_POINT('Ctrl Pts',(35.0239004925697,6.0979866226288,1.83811239380565));
#64245=CARTESIAN_POINT('Ctrl Pts',(35.057423795889,5.63825368842958,2.77290495152301));
#64246=CARTESIAN_POINT('Ctrl Pts',(35.0909470992083,5.17852075423038,3.70769750924034));
#64247=CARTESIAN_POINT('Ctrl Pts',(35.1244704025275,4.48131123098262,4.52569858398577));
#64248=CARTESIAN_POINT('Ctrl Pts',(35.1579937058468,3.63116147329114,5.12772589752581));
#64249=CARTESIAN_POINT('Ctrl Pts',(35.191517009166,2.78101171559963,5.72975321106586));
#64250=CARTESIAN_POINT('Ctrl Pts',(35.2250403124853,1.77792172346437,6.1158067634005));
#64251=CARTESIAN_POINT('Ctrl Pts',(35.2585636158046,0.743515726687463,6.23907772747215));
#64252=CARTESIAN_POINT('Ctrl Pts',(35.2920869191239,-0.290890270089445,
6.3623486915438));
#64253=CARTESIAN_POINT('Ctrl Pts',(35.3256102224431,-1.35661227150802,6.22283706735246));
#64254=CARTESIAN_POINT('Ctrl Pts',(35.3591335257624,-2.32443194359826,5.83745857928351));
#64255=CARTESIAN_POINT('Ctrl Pts',(35.3926568290817,-3.29225161568848,5.45208009121458));
#64256=CARTESIAN_POINT('Ctrl Pts',(35.4261801324009,-4.1621689584504,4.82083473926805));
#64257=CARTESIAN_POINT('Ctrl Pts',(35.4597034357202,-4.82870686849902,4.02026075067041));
#64258=CARTESIAN_POINT('Ctrl Pts',(35.4932267390395,-5.49524477854764,3.21968676207277));
#64259=CARTESIAN_POINT('Ctrl Pts',(35.5267500423587,-5.95840325588298,2.249784136824));
#64260=CARTESIAN_POINT('Ctrl Pts',(35.560273345678,-6.16202453447816,1.22815315077553));
#64261=CARTESIAN_POINT('Ctrl Pts',(35.5735282818838,-6.24253530730445,0.824205681250167));
#64262=CARTESIAN_POINT('Ctrl Pts',(35.5867832180896,-6.28247082274164,0.412171156905869));
#64263=CARTESIAN_POINT('Ctrl Pts',(35.6000381542954,-6.28225017164793,9.44259478526101E-5));
#64264=CARTESIAN_POINT('Origin',(37.,0.,0.));
#64265=CARTESIAN_POINT('',(37.0562984310705,-6.28313695873549,-8.10514889743041E-5));
#64266=CARTESIAN_POINT('',(36.8700381542954,-6.28321544720413,2.5547018683295E-5));
#64267=CARTESIAN_POINT('',(37.,-6.28269,-7.69407619853508E-16));
#64268=CARTESIAN_POINT('Ctrl Pts',(37.0562984310705,-6.28313695873549,-8.10514889743041E-5));
#64269=CARTESIAN_POINT('Ctrl Pts',(37.025394416607,-6.28251941297775,0.960289475135647));
#64270=CARTESIAN_POINT('Ctrl Pts',(36.9944904021436,-6.05897203089142,1.92093764266805));
#64271=CARTESIAN_POINT('Ctrl Pts',(36.9635863876801,-5.63376854407137,2.78200619005063));
#64272=CARTESIAN_POINT('Ctrl Pts',(36.9300630843609,-5.17252667279488,3.7160551346214));
#64273=CARTESIAN_POINT('Ctrl Pts',(36.8965397810416,-4.47399712145521,4.53292926279806));
#64274=CARTESIAN_POINT('Ctrl Pts',(36.8630164777223,-3.62287629749518,5.13358293813353));
#64275=CARTESIAN_POINT('Ctrl Pts',(36.829493174403,-2.77175547353512,5.73423661346902));
#64276=CARTESIAN_POINT('Ctrl Pts',(36.7959698710837,-1.76804337695468,6.11866983596331));
#64277=CARTESIAN_POINT('Ctrl Pts',(36.7624465677645,-0.733439667452159,
6.24027024285453));
#64278=CARTESIAN_POINT('Ctrl Pts',(36.7289232644452,0.30116404205033,6.36187064974575));
#64279=CARTESIAN_POINT('Ctrl Pts',(36.695399961126,1.3666593644749,6.22063824103392));
#64280=CARTESIAN_POINT('Ctrl Pts',(36.6618766578067,2.33385545058203,5.83369738548689));
#64281=CARTESIAN_POINT('Ctrl Pts',(36.6283533544875,3.30105153668919,5.44675652993986));
#64282=CARTESIAN_POINT('Ctrl Pts',(36.5948300511682,4.16994838647891,4.81410722755762));
#64283=CARTESIAN_POINT('Ctrl Pts',(36.5613067478489,4.83519263089985,4.01245793395268));
#64284=CARTESIAN_POINT('Ctrl Pts',(36.5277834445296,5.5004368753208,3.21080864034775));
#64285=CARTESIAN_POINT('Ctrl Pts',(36.4942601412104,5.96202851437296,2.24015935552012));
#64286=CARTESIAN_POINT('Ctrl Pts',(36.4607368378911,6.16399976049693,1.21820088747378));
#64287=CARTESIAN_POINT('Ctrl Pts',(36.4272135345719,6.36597100662089,0.196242419427446));
#64288=CARTESIAN_POINT('Ctrl Pts',(36.3936902312526,6.30832185981666,-0.877025231837599));
#64289=CARTESIAN_POINT('Ctrl Pts',(36.3601669279333,5.99804225432123,-1.87146882555525));
#64290=CARTESIAN_POINT('Ctrl Pts',(36.326643624614,5.6877626488258,-2.86591241927291));
#64291=CARTESIAN_POINT('Ctrl Pts',(36.2931203212948,5.12485258463917,-3.78153195544317));
#64292=CARTESIAN_POINT('Ctrl Pts',(36.2595970179755,4.3775646647594,-4.50730895940117));
#64293=CARTESIAN_POINT('Ctrl Pts',(36.2260737146563,3.63027674487965,-5.23308596335915));
#64294=CARTESIAN_POINT('Ctrl Pts',(36.192550411337,2.69861096930678,-5.76902043510487));
#64295=CARTESIAN_POINT('Ctrl Pts',(36.1590271080177,1.69553141232668,-6.05013055061307));
#64296=CARTESIAN_POINT('Ctrl Pts',(36.1255038046984,0.692451855346581,-6.33124066612126));
#64297=CARTESIAN_POINT('Ctrl Pts',(36.0919805013792,-0.382041483040742,
-6.35752642539192));
#64298=CARTESIAN_POINT('Ctrl Pts',(36.0584571980599,-1.39766674803318,-6.12580069142724));
#64299=CARTESIAN_POINT('Ctrl Pts',(36.0249338947406,-2.41329201302567,-5.89407495746255));
#64300=CARTESIAN_POINT('Ctrl Pts',(35.9914105914214,-3.37004920462326,-5.40433773026249));
#64301=CARTESIAN_POINT('Ctrl Pts',(35.9578872881021,-4.15193192514676,-4.71596943783516));
#64302=CARTESIAN_POINT('Ctrl Pts',(35.9243639847828,-4.9338146456702,-4.02760114540786));
#64303=CARTESIAN_POINT('Ctrl Pts',(35.8908406814636,-5.54082289511957,-3.14060178775331));
#64304=CARTESIAN_POINT('Ctrl Pts',(35.8573173781443,-5.89935718451418,-2.16251965520987));
#64305=CARTESIAN_POINT('Ctrl Pts',(35.8336443957864,-6.15254153889369,-1.47183231906614));
#64306=CARTESIAN_POINT('Ctrl Pts',(35.8099714134284,-6.28181964212573,-0.735724830331349));
#64307=CARTESIAN_POINT('Ctrl Pts',(35.7862984310705,-6.28249223374509,0.000152535273694049));
#64308=CARTESIAN_POINT('Ctrl Pts',(35.6000381542954,-6.28225017164793,9.44259478526101E-5));
#64309=CARTESIAN_POINT('Ctrl Pts',(35.6203065214089,-6.28191276999605,-0.630019693976204));
#64310=CARTESIAN_POINT('Ctrl Pts',(35.6405748885223,-6.18768209352705,-1.26023250153714));
#64311=CARTESIAN_POINT('Ctrl Pts',(35.6608432556358,-6.00105655529379,-1.86178053095313));
#64312=CARTESIAN_POINT('Ctrl Pts',(35.6943665589551,-5.69238321765922,-2.85672387978495));
#64313=CARTESIAN_POINT('Ctrl Pts',(35.7278898622743,-5.13095246253506,-3.77325123060037));
#64314=CARTESIAN_POINT('Ctrl Pts',(35.7614131655936,-4.38483752733227,-4.50023403659957));
#64315=CARTESIAN_POINT('Ctrl Pts',(35.7949364689129,-3.63872259212945,-5.22721684259882));
#64316=CARTESIAN_POINT('Ctrl Pts',(35.8284597722321,-2.70792347684797,-5.7646551037818));
#64317=CARTESIAN_POINT('Ctrl Pts',(35.8619830755514,-1.70529917358644,-6.04738466230123));
#64318=CARTESIAN_POINT('Ctrl Pts',(35.8955063788707,-0.702674870324941,
-6.33011422082064));
#64319=CARTESIAN_POINT('Ctrl Pts',(35.9290296821899,0.371774620916599,-6.35813507667651));
#64320=CARTESIAN_POINT('Ctrl Pts',(35.9625529855092,1.38777276178361,-6.12804971315688));
#64321=CARTESIAN_POINT('Ctrl Pts',(35.9960762888285,2.40377090265057,-5.89796434963727));
#64322=CARTESIAN_POINT('Ctrl Pts',(36.0295995921477,3.36131769314301,-5.4097727667422));
#64323=CARTESIAN_POINT('Ctrl Pts',(36.063122895467,4.14431099705559,-4.72266798377303));
#64324=CARTESIAN_POINT('Ctrl Pts',(36.0966461987863,4.92730430096823,-4.03556320080382));
#64325=CARTESIAN_POINT('Ctrl Pts',(36.1301695021055,5.53574411830099,-3.14954521776048));
#64326=CARTESIAN_POINT('Ctrl Pts',(36.1636928054248,5.8958573830835,-2.17204333373218));
#64327=CARTESIAN_POINT('Ctrl Pts',(36.1972161087441,6.25597064786602,-1.19454144970389));
#64328=CARTESIAN_POINT('Ctrl Pts',(36.2307394120633,6.36775736009829,-0.125555664690637));
#64329=CARTESIAN_POINT('Ctrl Pts',(36.2642627153826,6.21766342903676,0.905299954981527));
#64330=CARTESIAN_POINT('Ctrl Pts',(36.2977860187019,6.06756949797523,1.93615557465366));
#64331=CARTESIAN_POINT('Ctrl Pts',(36.3313093220211,5.65559492361991,2.92888102898471));
#64332=CARTESIAN_POINT('Ctrl Pts',(36.3648326253404,5.03169144579161,3.76310878392031));
#64333=CARTESIAN_POINT('Ctrl Pts',(36.3983559286597,4.4077879679633,4.59733653885593));
#64334=CARTESIAN_POINT('Ctrl Pts',(36.431879231979,3.57195558666201,5.27306659439609));
#64335=CARTESIAN_POINT('Ctrl Pts',(36.4654025352982,2.62553861836627,5.70836697215044));
#64336=CARTESIAN_POINT('Ctrl Pts',(36.4989258386175,1.67912165007053,6.1436673499048));
#64337=CARTESIAN_POINT('Ctrl Pts',(36.5324491419367,0.622120094780342,6.33853804987336));
#64338=CARTESIAN_POINT('Ctrl Pts',(36.565972445256,-0.417305063873974,6.26935108356007));
#64339=CARTESIAN_POINT('Ctrl Pts',(36.5994957485753,-1.45673022252826,6.20016411724678));
#64340=CARTESIAN_POINT('Ctrl Pts',(36.6330190518946,-2.47857898454668,5.86691948465166));
#64341=CARTESIAN_POINT('Ctrl Pts',(36.6665423552138,-3.35895262735287,5.3100229540436));
#64342=CARTESIAN_POINT('Ctrl Pts',(36.7000656585331,-4.23932627015908,4.75312642343553));
#64343=CARTESIAN_POINT('Ctrl Pts',(36.7335889618523,-4.97822479375304,3.9725779948145));
#64344=CARTESIAN_POINT('Ctrl Pts',(36.7671122651716,-5.48605707018151,3.06301882919158));
#64345=CARTESIAN_POINT('Ctrl Pts',(36.8006355684909,-5.99388934660998,2.15345966356866));
#64346=CARTESIAN_POINT('Ctrl Pts',(36.8341588718101,-6.27065537587296,1.11488976094384));
#64347=CARTESIAN_POINT('Ctrl Pts',(36.8676821751294,-6.28279739604637,0.0732352749950272));
#64348=CARTESIAN_POINT('Ctrl Pts',(36.8684675015181,-6.28308183844643,0.0488331822806146));
#64349=CARTESIAN_POINT('Ctrl Pts',(36.8692528279068,-6.28322105764272,0.0244293967754612));
#64350=CARTESIAN_POINT('Ctrl Pts',(36.8700381542954,-6.28321544720413,2.5547018683295E-5));
#64351=CARTESIAN_POINT('Origin',(37.,0.,0.));
#64352=CARTESIAN_POINT('',(38.3262984310705,-6.28217936372029,-4.73315304236333E-5));
#64353=CARTESIAN_POINT('',(38.1400381542954,-6.2823463260306,-0.000127106979284774));
#64354=CARTESIAN_POINT('',(37.,-6.28269,-7.69407619853508E-16));
#64355=CARTESIAN_POINT('Ctrl Pts',(38.3262984310705,-6.28217936372029,-4.73315304236333E-5));
#64356=CARTESIAN_POINT('Ctrl Pts',(38.3078640264242,-6.282027712414,0.573070045152017));
#64357=CARTESIAN_POINT('Ctrl Pts',(38.2894296217778,-6.20429023609247,1.1462277488213));
#64358=CARTESIAN_POINT('Ctrl Pts',(38.2709952171315,-6.04950488904637,1.69776236471778));
#64359=CARTESIAN_POINT('Ctrl Pts',(38.2374719138122,-5.76802489346411,2.7007381903285));
#64360=CARTESIAN_POINT('Ctrl Pts',(38.203948610493,-5.23174689377087,3.63220626945104));
#64361=CARTESIAN_POINT('Ctrl Pts',(38.1704253071737,-4.50569436660769,4.37922649840903));
#64362=CARTESIAN_POINT('Ctrl Pts',(38.1369020038545,-3.77964183944451,5.12624672736702));
#64363=CARTESIAN_POINT('Ctrl Pts',(38.1033787005352,-2.86381478481141,5.68881910616045));
#64364=CARTESIAN_POINT('Ctrl Pts',(38.0698553972159,-1.86925683889755,5.99873197599983));
#64365=CARTESIAN_POINT('Ctrl Pts',(38.0363320938967,-0.874698892983714,
6.30864484583921));
#64366=CARTESIAN_POINT('Ctrl Pts',(38.0028087905774,0.198589944210873,6.36589820672455));
#64367=CARTESIAN_POINT('Ctrl Pts',(37.9692854872581,1.22047386313528,6.16355011329118));
#64368=CARTESIAN_POINT('Ctrl Pts',(37.9357621839389,2.24235778205969,5.96120201985782));
#64369=CARTESIAN_POINT('Ctrl Pts',(37.9022388806196,3.21283678271391,5.49925247210574));
#64370=CARTESIAN_POINT('Ctrl Pts',(37.8687155773003,4.01424070397671,4.83371265387017));
#64371=CARTESIAN_POINT('Ctrl Pts',(37.8351922739811,4.81564462523956,4.16817283563458));
#64372=CARTESIAN_POINT('Ctrl Pts',(37.8016689706618,5.44797346711096,3.29904274691547));
#64373=CARTESIAN_POINT('Ctrl Pts',(37.7681456673425,5.83455762967741,2.331704036884));
#64374=CARTESIAN_POINT('Ctrl Pts',(37.7346223640233,6.22114179224384,1.36436532685259));
#64375=CARTESIAN_POINT('Ctrl Pts',(37.701099060704,6.36198127550534,0.298817995508832));
#64376=CARTESIAN_POINT('Ctrl Pts',(37.6675757573847,6.23999935273579,-0.735740801848701));
#64377=CARTESIAN_POINT('Ctrl Pts',(37.6340524540655,6.11801742996624,-1.77029959920626));
#64378=CARTESIAN_POINT('Ctrl Pts',(37.6005291507462,5.73321410116562,-2.7738698625776));
#64379=CARTESIAN_POINT('Ctrl Pts',(37.5670058474269,5.13224660432614,-3.62476912947996));
#64380=CARTESIAN_POINT('Ctrl Pts',(37.5334825441077,4.53127910748666,-4.47566839638232));
#64381=CARTESIAN_POINT('Ctrl Pts',(37.4999592407884,3.71414744260832,-5.1738966668157));
#64382=CARTESIAN_POINT('Ctrl Pts',(37.4664359374691,2.77992847235244,-5.63479406351752));
#64383=CARTESIAN_POINT('Ctrl Pts',(37.4329126341498,1.84570950209658,-6.09569146021933));
#64384=CARTESIAN_POINT('Ctrl Pts',(37.3993893308306,0.794403226463186,-6.31925798318959));
#64385=CARTESIAN_POINT('Ctrl Pts',(37.3658660275113,-0.2465199211245,-6.27838628774439));
#64386=CARTESIAN_POINT('Ctrl Pts',(37.3323427241921,-1.28744306871219,-6.2375145922992));
#64387=CARTESIAN_POINT('Ctrl Pts',(37.2988194208728,-2.31798308825416,-5.93220467843854));
#64388=CARTESIAN_POINT('Ctrl Pts',(37.2652961175535,-3.21318744594017,-5.39947524180827));
#64389=CARTESIAN_POINT('Ctrl Pts',(37.2317728142342,-4.10839180362623,-4.86674580517798));
#64390=CARTESIAN_POINT('Ctrl Pts',(37.198249510915,-4.8682604994563,-4.10659684577804));
#64391=CARTESIAN_POINT('Ctrl Pts',(37.1647262075957,-5.40065978111937,-3.21119609775669));
#64392=CARTESIAN_POINT('Ctrl Pts',(37.1312029042765,-5.9330590627824,-2.31579534973541));
#64393=CARTESIAN_POINT('Ctrl Pts',(37.0976796009572,-6.23798893027845,-1.28514281309276));
#64394=CARTESIAN_POINT('Ctrl Pts',(37.0641562976379,-6.27847676841984,-0.244204664288998));
#64395=CARTESIAN_POINT('Ctrl Pts',(37.0615370087821,-6.28164021989209,-0.162872652738991));
#64396=CARTESIAN_POINT('Ctrl Pts',(37.0589177199263,-6.28318929920806,-0.0814778493327739));
#64397=CARTESIAN_POINT('Ctrl Pts',(37.0562984310705,-6.28313695873549,-8.10514889743041E-5));
#64398=CARTESIAN_POINT('Ctrl Pts',(36.8700381542954,-6.28321544720413,2.5547018683295E-5));
#64399=CARTESIAN_POINT('Ctrl Pts',(36.902776131226,-6.28298156430956,-1.01730009221029));
#64400=CARTESIAN_POINT('Ctrl Pts',(36.9355141081566,-6.03106071247253,-2.0347373888128));
#64401=CARTESIAN_POINT('Ctrl Pts',(36.9682520850872,-5.55596476178223,-2.93430777034463));
#64402=CARTESIAN_POINT('Ctrl Pts',(37.0017753884065,-5.06947209626076,-3.85545726046282));
#64403=CARTESIAN_POINT('Ctrl Pts',(37.0352986917257,-4.34896875413393,-4.65301717142637));
#64404=CARTESIAN_POINT('Ctrl Pts',(37.068821995045,-3.48181545551966,-5.23028370731217));
#64405=CARTESIAN_POINT('Ctrl Pts',(37.1023452983643,-2.6146621569054,-5.80755024319796));
#64406=CARTESIAN_POINT('Ctrl Pts',(37.1358686016836,-1.60085890180369,-6.164523404006));
#64407=CARTESIAN_POINT('Ctrl Pts',(37.1693919050028,-0.563328898540168,
-6.25792034763468));
#64408=CARTESIAN_POINT('Ctrl Pts',(37.2029152083221,0.474201104723353,-6.35131729126336));
#64409=CARTESIAN_POINT('Ctrl Pts',(37.2364385116413,1.5354578561487,-6.18113801771268));
#64410=CARTESIAN_POINT('Ctrl Pts',(37.2699618149606,2.49176443140565,-5.76801669065306));
#64411=CARTESIAN_POINT('Ctrl Pts',(37.3034851182799,3.44807100666263,-5.35489536359344));
#64412=CARTESIAN_POINT('Ctrl Pts',(37.3370084215992,4.29942740575116,-4.69883198302491));
#64413=CARTESIAN_POINT('Ctrl Pts',(37.3705317249184,4.94260703171787,-3.87937395146224));
#64414=CARTESIAN_POINT('Ctrl Pts',(37.4040550282377,5.58578665768455,-3.05991591989961));
#64415=CARTESIAN_POINT('Ctrl Pts',(37.4375783315569,6.02078951052939,-2.07706323734282));
#64416=CARTESIAN_POINT('Ctrl Pts',(37.4711016348762,6.19487168157636,-1.04998636851815));
#64417=CARTESIAN_POINT('Ctrl Pts',(37.5046249381955,6.36895385262334,-0.022909499693449));
#64418=CARTESIAN_POINT('Ctrl Pts',(37.5381482415148,6.28211534187248,1.04839155539914));
#64419=CARTESIAN_POINT('Ctrl Pts',(37.571671544834,5.94488528137579,2.03402200493313));
#64420=CARTESIAN_POINT('Ctrl Pts',(37.6051948481533,5.60765522087911,3.01965245446706));
#64421=CARTESIAN_POINT('Ctrl Pts',(37.6387181514726,5.02003361063657,3.91961229844241));
#64422=CARTESIAN_POINT('Ctrl Pts',(37.6722414547918,4.25326931796938,4.62478179313262));
#64423=CARTESIAN_POINT('Ctrl Pts',(37.7057647581111,3.48650502530215,5.32995128782288));
#64424=CARTESIAN_POINT('Ctrl Pts',(37.7392880614304,2.54059805021029,5.84033043322802));
#64425=CARTESIAN_POINT('Ctrl Pts',(37.7728113647496,1.53023920629164,6.09403597764229));
#64426=CARTESIAN_POINT('Ctrl Pts',(37.8063346680689,0.519880362372982,6.34774152205655));
#64427=CARTESIAN_POINT('Ctrl Pts',(37.8398579713882,-0.554930350372418,
6.34477346547987));
#64428=CARTESIAN_POINT('Ctrl Pts',(37.8733812747074,-1.5638725956381,6.08549168349467));
#64429=CARTESIAN_POINT('Ctrl Pts',(37.9069045780267,-2.57281484090379,5.82620990150948));
#64430=CARTESIAN_POINT('Ctrl Pts',(37.940427881346,-3.51588861868977,5.31061439411577));
#64431=CARTESIAN_POINT('Ctrl Pts',(37.9739511846652,-4.27874663935198,4.60122089466533));
#64432=CARTESIAN_POINT('Ctrl Pts',(38.0074744879845,-5.0416046600142,3.89182739521488));
#64433=CARTESIAN_POINT('Ctrl Pts',(38.0409977913038,-5.62424692355264,2.98863590370768));
#64434=CARTESIAN_POINT('Ctrl Pts',(38.074521094623,-5.95602830629082,2.00115799974245));
#64435=CARTESIAN_POINT('Ctrl Pts',(38.0963601145138,-6.17216990033383,1.35785774436396));
#64436=CARTESIAN_POINT('Ctrl Pts',(38.1181991344046,-6.28184679862301,0.678786557982193));
#64437=CARTESIAN_POINT('Ctrl Pts',(38.1400381542954,-6.2823463260306,-0.000127106979284774));
#64438=CARTESIAN_POINT('Origin',(37.,0.,0.));
#64439=CARTESIAN_POINT('',(39.5962984310705,-6.28286224794853,0.000148810185861201));
#64440=CARTESIAN_POINT('',(39.4100381542954,-6.282535125309,0.000156527191468202));
#64441=CARTESIAN_POINT('',(37.,-6.28269,-7.69407619853508E-16));
#64442=CARTESIAN_POINT('Ctrl Pts',(39.5962984310705,-6.28286224794853,0.000148810185861201));
#64443=CARTESIAN_POINT('Ctrl Pts',(39.5903336362413,-6.28304804443731,0.18553371703489));
#64444=CARTESIAN_POINT('Ctrl Pts',(39.5843688414121,-6.27500548490837,0.370902559242192));
#64445=CARTESIAN_POINT('Ctrl Pts',(39.578404046583,-6.25861743229305,0.555530634479874));
#64446=CARTESIAN_POINT('Ctrl Pts',(39.5448807432637,-6.16651339948561,1.59317621068257));
#64447=CARTESIAN_POINT('Ctrl Pts',(39.5113574399444,-5.81080378911597,2.60742349239934));
#64448=CARTESIAN_POINT('Ctrl Pts',(39.4778341366252,-5.23461823833893,3.47529543326859));
#64449=CARTESIAN_POINT('Ctrl Pts',(39.4443108333059,-4.65843268756187,4.34316737413788));
#64450=CARTESIAN_POINT('Ctrl Pts',(39.4107875299866,-3.86177119637738,5.06466397415965));
#64451=CARTESIAN_POINT('Ctrl Pts',(39.3772642266674,-2.94122862769708,5.55230408112373));
#64452=CARTESIAN_POINT('Ctrl Pts',(39.3437409233481,-2.02068605901675,6.03994418808783));
#64453=CARTESIAN_POINT('Ctrl Pts',(39.3102176200289,-0.976262412840673,
6.29372780199423));
#64454=CARTESIAN_POINT('Ctrl Pts',(39.2766943167096,0.0654063932673694,
6.28288376888892));
#64455=CARTESIAN_POINT('Ctrl Pts',(39.2431710133903,1.10707519937532,6.27203973578361));
#64456=CARTESIAN_POINT('Ctrl Pts',(39.209647710071,2.14598916541525,5.99656805566658));
#64457=CARTESIAN_POINT('Ctrl Pts',(39.1761244067517,3.0561804201681,5.48986955118509));
#64458=CARTESIAN_POINT('Ctrl Pts',(39.1426011034325,3.96637167492101,4.98317104670358));
#64459=CARTESIAN_POINT('Ctrl Pts',(39.1090778001132,4.74784021838694,4.24524571785757));
#64460=CARTESIAN_POINT('Ctrl Pts',(39.075554496794,5.3058333260259,3.365566693156));
#64461=CARTESIAN_POINT('Ctrl Pts',(39.0420311934747,5.86382643366487,2.48588766845441));
#64462=CARTESIAN_POINT('Ctrl Pts',(39.0085078901554,6.19834410547685,1.46445494789734));
#64463=CARTESIAN_POINT('Ctrl Pts',(38.9749845868362,6.26882621773588,0.425116809212897));
#64464=CARTESIAN_POINT('Ctrl Pts',(38.9414612835169,6.3393083299949,-0.61422132947149));
#64465=CARTESIAN_POINT('Ctrl Pts',(38.9079379801976,6.14575488270097,-1.67146488628317));
#64466=CARTESIAN_POINT('Ctrl Pts',(38.8744146768784,5.7116341480303,-2.61842353501152));
#64467=CARTESIAN_POINT('Ctrl Pts',(38.8408913735591,5.27751341335964,-3.56538218373986));
#64468=CARTESIAN_POINT('Ctrl Pts',(38.8073680702398,4.60282539131222,-4.40205592438488));
#64469=CARTESIAN_POINT('Ctrl Pts',(38.7738447669205,3.76937571416591,-5.02699842600973));
#64470=CARTESIAN_POINT('Ctrl Pts',(38.7403214636013,2.93592603701955,-5.65194092763462));
#64471=CARTESIAN_POINT('Ctrl Pts',(38.706798160282,1.94371470477427,-6.06515219023933));
#64472=CARTESIAN_POINT('Ctrl Pts',(38.6732748569627,0.913046914402851,-6.21653052608507));
#64473=CARTESIAN_POINT('Ctrl Pts',(38.6397515536435,-0.117620875968512,
-6.36790886193081));
#64474=CARTESIAN_POINT('Ctrl Pts',(38.6062282503242,-1.18674512446603,-6.25745427101762));
#64475=CARTESIAN_POINT('Ctrl Pts',(38.572704947005,-2.16469497612578,-5.89855932495248));
#64476=CARTESIAN_POINT('Ctrl Pts',(38.5391816436857,-3.14264482778553,-5.53966437888735));
#64477=CARTESIAN_POINT('Ctrl Pts',(38.5056583403664,-4.02942028260758,-4.93232907767022));
#64478=CARTESIAN_POINT('Ctrl Pts',(38.4721350370471,-4.7175001983755,-4.15019256516793));
#64479=CARTESIAN_POINT('Ctrl Pts',(38.4386117337279,-5.40558011414346,-3.36805605266561));
#64480=CARTESIAN_POINT('Ctrl Pts',(38.4050884304086,-5.8949644908573,-2.41111832887814));
#64481=CARTESIAN_POINT('Ctrl Pts',(38.3715651270894,-6.12631568347861,-1.39540768093492));
#64482=CARTESIAN_POINT('Ctrl Pts',(38.3564762284164,-6.23044726830737,-0.938234504953467));
#64483=CARTESIAN_POINT('Ctrl Pts',(38.3413873297434,-6.28230349309892,-0.469154427224146));
#64484=CARTESIAN_POINT('Ctrl Pts',(38.3262984310705,-6.28217936372029,-4.73315304236333E-5));
#64485=CARTESIAN_POINT('Ctrl Pts',(38.1400381542954,-6.2823463260306,-0.000127106979284774));
#64486=CARTESIAN_POINT('Ctrl Pts',(38.1517224377239,-6.28261358252104,-0.363358594680692));
#64487=CARTESIAN_POINT('Ctrl Pts',(38.1634067211523,-6.25162936468712,-0.726544992666329));
#64488=CARTESIAN_POINT('Ctrl Pts',(38.1750910045808,-6.18897823607404,-1.08418398746365));
#64489=CARTESIAN_POINT('Ctrl Pts',(38.2086143079001,-6.00922628118114,-2.11028375428133));
#64490=CARTESIAN_POINT('Ctrl Pts',(38.2421376112194,-5.56880186945739,-3.09071897149348));
#64491=CARTESIAN_POINT('Ctrl Pts',(38.2756609145386,-4.92110627125931,-3.90661229100649));
#64492=CARTESIAN_POINT('Ctrl Pts',(38.3091842178579,-4.27341067306123,-4.7225056105195));
#64493=CARTESIAN_POINT('Ctrl Pts',(38.3427075211772,-3.41844388838883,-5.37385703233337));
#64494=CARTESIAN_POINT('Ctrl Pts',(38.3762308244964,-2.45987027189365,-5.78169047690418));
#64495=CARTESIAN_POINT('Ctrl Pts',(38.4097541278157,-1.50129665539843,-6.18952392147501));
#64496=CARTESIAN_POINT('Ctrl Pts',(38.443277431135,-0.439116207080419,-6.35383938880275));
#64497=CARTESIAN_POINT('Ctrl Pts',(38.4768007344543,0.597882150879494,-6.25471369919763));
#64498=CARTESIAN_POINT('Ctrl Pts',(38.5103240377735,1.63488050883938,-6.1555880095925));
#64499=CARTESIAN_POINT('Ctrl Pts',(38.5438473410928,2.64669677644117,-5.79302116305454));
#64500=CARTESIAN_POINT('Ctrl Pts',(38.577370644412,3.51064866673838,-5.2109742336725));
#64501=CARTESIAN_POINT('Ctrl Pts',(38.6108939477313,4.37460055703559,-4.62892730429046));
#64502=CARTESIAN_POINT('Ctrl Pts',(38.6444172510506,5.09068807002823,-3.82740029206434));
#64503=CARTESIAN_POINT('Ctrl Pts',(38.6779405543698,5.57208590298025,-2.90357800223784));
#64504=CARTESIAN_POINT('Ctrl Pts',(38.7114638576891,6.05348373593226,-1.97975571241136));
#64505=CARTESIAN_POINT('Ctrl Pts',(38.7449871610084,6.30019188884368,-0.933638144984511));
#64506=CARTESIAN_POINT('Ctrl Pts',(38.7785104643276,6.28229710436072,0.107933395256214));
#64507=CARTESIAN_POINT('Ctrl Pts',(38.8120337676469,6.26440231987777,1.14950493549694));
#64508=CARTESIAN_POINT('Ctrl Pts',(38.8455570709662,5.98190459800044,2.18653044855153));
#64509=CARTESIAN_POINT('Ctrl Pts',(38.8790803742854,5.46905666591529,3.09327103731279));
#64510=CARTESIAN_POINT('Ctrl Pts',(38.9126036776047,4.95620873383013,4.00001162607407));
#64511=CARTESIAN_POINT('Ctrl Pts',(38.946126980924,4.21301059153714,4.77646729054201));
#64512=CARTESIAN_POINT('Ctrl Pts',(38.9796502842433,3.3295746939062,5.32849311559751));
#64513=CARTESIAN_POINT('Ctrl Pts',(39.0131735875625,2.44613879627526,5.88051894065301));
#64514=CARTESIAN_POINT('Ctrl Pts',(39.0466968908818,1.42246514330638,6.20811492629609));
#64515=CARTESIAN_POINT('Ctrl Pts',(39.0802201942011,0.382673724818222,6.27156020026951));
#64516=CARTESIAN_POINT('Ctrl Pts',(39.1137434975203,-0.657117693669971,
6.33500547424293));
#64517=CARTESIAN_POINT('Ctrl Pts',(39.1472668008396,-1.71302687767745,6.13430003654668));
#64518=CARTESIAN_POINT('Ctrl Pts',(39.1807901041589,-2.65702529312174,5.69377933511495));
#64519=CARTESIAN_POINT('Ctrl Pts',(39.2143134074781,-3.60102370856599,5.25325863368324));
#64520=CARTESIAN_POINT('Ctrl Pts',(39.2478367107974,-4.43311135544706,4.57292266851607));
#64521=CARTESIAN_POINT('Ctrl Pts',(39.2813600141166,-5.0523979647231,3.7352618825636));
#64522=CARTESIAN_POINT('Ctrl Pts',(39.3148833174359,-5.67168457399914,2.89760109661113));
#64523=CARTESIAN_POINT('Ctrl Pts',(39.3484066207552,-6.07817014567012,1.90261548987344));
#64524=CARTESIAN_POINT('Ctrl Pts',(39.3819299240745,-6.22256847912821,0.870946638911246));
#64525=CARTESIAN_POINT('Ctrl Pts',(39.3912993341481,-6.26292629193788,0.582606064809031));
#64526=CARTESIAN_POINT('Ctrl Pts',(39.4006687442218,-6.28281132775394,0.29140000254511));
#64527=CARTESIAN_POINT('Ctrl Pts',(39.4100381542954,-6.282535125309,0.000156527191468202));
#64528=CARTESIAN_POINT('Origin',(37.,0.,0.));
#64529=CARTESIAN_POINT('',(40.8662984310705,-6.28281011036189,-0.000154357209955491));
#64530=CARTESIAN_POINT('',(40.6800381542954,-6.28310564591676,-9.39174517631389E-5));
#64531=CARTESIAN_POINT('',(37.,-6.28269,-7.69407619853508E-16));
#64532=CARTESIAN_POINT('Ctrl Pts',(40.8662984310705,-6.28281011036189,-0.000154357209955491));
#64533=CARTESIAN_POINT('Ctrl Pts',(40.8392799427392,-6.28195467965013,0.839596208053496));
#64534=CARTESIAN_POINT('Ctrl Pts',(40.8122614544079,-6.11248623477459,1.6796816398236));
#64535=CARTESIAN_POINT('Ctrl Pts',(40.7852429660766,-5.78475116091983,2.45266395086745));
#64536=CARTESIAN_POINT('Ctrl Pts',(40.7517196627573,-5.37811248615472,3.41174501253935));
#64537=CARTESIAN_POINT('Ctrl Pts',(40.718196359438,-4.72782692174914,4.26752276412259));
#64538=CARTESIAN_POINT('Ctrl Pts',(40.6846730561188,-3.91274131249501,4.91623452157674));
#64539=CARTESIAN_POINT('Ctrl Pts',(40.6511497527995,-3.09765570324088,5.56494627903089));
#64540=CARTESIAN_POINT('Ctrl Pts',(40.6176264494803,-2.11777004913822,6.00659204235594));
#64541=CARTESIAN_POINT('Ctrl Pts',(40.584103146161,-1.09189506399012,6.18762245283939));
#64542=CARTESIAN_POINT('Ctrl Pts',(40.5505798428417,-0.0660200788419529,
6.36865286332285));
#64543=CARTESIAN_POINT('Ctrl Pts',(40.5170565395225,1.00584423735164,6.28906792096469));
#64544=CARTESIAN_POINT('Ctrl Pts',(40.4835332362032,1.99373479759796,5.95851726577133));
#64545=CARTESIAN_POINT('Ctrl Pts',(40.4500099328839,2.98162535784423,5.627966610578));
#64546=CARTESIAN_POINT('Ctrl Pts',(40.4164866295647,3.88554216214322,5.0464502425495));
#64547=CARTESIAN_POINT('Ctrl Pts',(40.3829633262454,4.59588568703246,4.2844767710163));
#64548=CARTESIAN_POINT('Ctrl Pts',(40.3494400229261,5.30622921192172,3.52250329948308));
#64549=CARTESIAN_POINT('Ctrl Pts',(40.3159167196068,5.82299945740124,2.58007272444507));
#64550=CARTESIAN_POINT('Ctrl Pts',(40.2823934162875,6.08353825363188,1.57145434749016));
#64551=CARTESIAN_POINT('Ctrl Pts',(40.2488701129683,6.3440770498625,0.562835970535265));
#64552=CARTESIAN_POINT('Ctrl Pts',(40.215346809649,6.34838439684431,-0.5119702083366));
#64553=CARTESIAN_POINT('Ctrl Pts',(40.1818235063298,6.09593803060969,-1.52264440254924));
#64554=CARTESIAN_POINT('Ctrl Pts',(40.1483002030105,5.84349166437507,-2.53331859676188));
#64555=CARTESIAN_POINT('Ctrl Pts',(40.1147768996912,5.33429158492403,-3.47986080631527));
#64556=CARTESIAN_POINT('Ctrl Pts',(40.081253596372,4.63007808272299,-4.24750319570642));
#64557=CARTESIAN_POINT('Ctrl Pts',(40.0477302930527,3.9258645805219,-5.01514558509763));
#64558=CARTESIAN_POINT('Ctrl Pts',(40.0142069897334,3.02663765557088,-5.60388815432652));
#64559=CARTESIAN_POINT('Ctrl Pts',(39.9806836864142,2.04142818547992,-5.94234612027744));
#64560=CARTESIAN_POINT('Ctrl Pts',(39.9471603830949,1.05621871538901,-6.28080408622833));
#64561=CARTESIAN_POINT('Ctrl Pts',(39.9136370797757,-0.0149732998418345,
-6.36897744890122));
#64562=CARTESIAN_POINT('Ctrl Pts',(39.8801137764564,-1.04226628942212,-6.19617522602309));
#64563=CARTESIAN_POINT('Ctrl Pts',(39.8465904731371,-2.06955927900244,-6.02337300314495));
#64564=CARTESIAN_POINT('Ctrl Pts',(39.8130671698178,-3.05295324293226,-5.5895951947158));
#64565=CARTESIAN_POINT('Ctrl Pts',(39.7795438664985,-3.873212086352,-4.94743717330346));
#64566=CARTESIAN_POINT('Ctrl Pts',(39.7460205631793,-4.69347092977173,-4.30527915189112));
#64567=CARTESIAN_POINT('Ctrl Pts',(39.71249725986,-5.35059465268135,-3.4547409174956));
#64568=CARTESIAN_POINT('Ctrl Pts',(39.6789739565408,-5.76490728651354,-2.49894986495351));
#64569=CARTESIAN_POINT('Ctrl Pts',(39.6514154480507,-6.10550135411715,-1.71322252819967));
#64570=CARTESIAN_POINT('Ctrl Pts',(39.6238569395606,-6.28200383215044,-0.856365399548567));
#64571=CARTESIAN_POINT('Ctrl Pts',(39.5962984310705,-6.28286224794853,0.000148810185861201));
#64572=CARTESIAN_POINT('Ctrl Pts',(39.4100381542954,-6.282535125309,0.000156527191468202));
#64573=CARTESIAN_POINT('Ctrl Pts',(39.434192047541,-6.28182308855144,-0.7506552909351));
#64574=CARTESIAN_POINT('Ctrl Pts',(39.4583459407866,-6.1471227161439,-1.50171575041843));
#64575=CARTESIAN_POINT('Ctrl Pts',(39.4824998340322,-5.88377149391016,-2.20457241494147));
#64576=CARTESIAN_POINT('Ctrl Pts',(39.5160231373515,-5.5182650799889,-3.18007052264519));
#64577=CARTESIAN_POINT('Ctrl Pts',(39.5495464406708,-4.90494115690126,-4.06271464286602));
#64578=CARTESIAN_POINT('Ctrl Pts',(39.5830697439901,-4.11816498633818,-4.74548455592988));
#64579=CARTESIAN_POINT('Ctrl Pts',(39.6165930473094,-3.33138881577507,-5.42825446899375));
#64580=CARTESIAN_POINT('Ctrl Pts',(39.6501163506286,-2.37116039773654,-5.91115017490064));
#64581=CARTESIAN_POINT('Ctrl Pts',(39.6836396539478,-1.35390701461365,-6.13562077715455));
#64582=CARTESIAN_POINT('Ctrl Pts',(39.7171629572671,-0.336653631490792,
-6.36009137940847));
#64583=CARTESIAN_POINT('Ctrl Pts',(39.7506862605864,0.737624716716394,-6.32613687800943));
#64584=CARTESIAN_POINT('Ctrl Pts',(39.7842095639057,1.73867224267262,-6.03787424163757));
#64585=CARTESIAN_POINT('Ctrl Pts',(39.8177328672249,2.73971976862887,-5.7496116052657));
#64586=CARTESIAN_POINT('Ctrl Pts',(39.8512561705442,3.66753647233414,-5.20704083392101));
#64587=CARTESIAN_POINT('Ctrl Pts',(39.8847794738634,4.40962497780978,-4.47594840009877));
#64588=CARTESIAN_POINT('Ctrl Pts',(39.9183027771827,5.15171348328543,-3.74485596627654));
#64589=CARTESIAN_POINT('Ctrl Pts',(39.951826080502,5.70807379053144,-2.82524186997678));
#64590=CARTESIAN_POINT('Ctrl Pts',(39.9853493838213,6.0112474517597,-1.82860892456074));
#64591=CARTESIAN_POINT('Ctrl Pts',(40.0188726871405,6.31442111298794,-0.831975979144762));
#64592=CARTESIAN_POINT('Ctrl Pts',(40.0523959904598,6.36440812819845,0.241675815387561));
#64593=CARTESIAN_POINT('Ctrl Pts',(40.0859192937791,6.15514759331208,1.26216664106418));
#64594=CARTESIAN_POINT('Ctrl Pts',(40.1194425970983,5.94588705842569,2.28265746674088));
#64595=CARTESIAN_POINT('Ctrl Pts',(40.1529659004176,5.47737897344238,3.24998732356193));
#64596=CARTESIAN_POINT('Ctrl Pts',(40.1864892037369,4.80642974201378,4.04686788274043));
#64597=CARTESIAN_POINT('Ctrl Pts',(40.2200125070561,4.13548051058523,4.84374844191888));
#64598=CARTESIAN_POINT('Ctrl Pts',(40.2535358103754,3.26209013271142,5.47017970345478));
#64599=CARTESIAN_POINT('Ctrl Pts',(40.2870591136947,2.29215681578979,5.85020714651191));
#64600=CARTESIAN_POINT('Ctrl Pts',(40.3205824170139,1.32222349886816,6.23023458956905));
#64601=CARTESIAN_POINT('Ctrl Pts',(40.3541057203332,0.25574724289874,6.36385821414741));
#64602=CARTESIAN_POINT('Ctrl Pts',(40.3876290236525,-0.777962165108884,
6.2348762132804));
#64603=CARTESIAN_POINT('Ctrl Pts',(40.4211523269717,-1.81167157311654,6.10589421241339));
#64604=CARTESIAN_POINT('Ctrl Pts',(40.454675630291,-2.81261413316237,5.71430658610099));
#64605=CARTESIAN_POINT('Ctrl Pts',(40.4881989336103,-3.65942599066088,5.10759316548865));
#64606=CARTESIAN_POINT('Ctrl Pts',(40.5217222369295,-4.50623784815938,4.5008797448763));
#64607=CARTESIAN_POINT('Ctrl Pts',(40.5552455402488,-5.19891900311054,3.67904052996403));
#64608=CARTESIAN_POINT('Ctrl Pts',(40.588768843568,-5.65348216361643,2.74172317182855));
#64609=CARTESIAN_POINT('Ctrl Pts',(40.6191919471438,-6.06600780233705,1.89108793465174));
#64610=CARTESIAN_POINT('Ctrl Pts',(40.6496150507196,-6.28242077900449,0.945345537979423));
#64611=CARTESIAN_POINT('Ctrl Pts',(40.6800381542954,-6.28310564591676,-9.39174517631389E-5));
#64612=CARTESIAN_POINT('Origin',(37.,0.,0.));
#64613=CARTESIAN_POINT('',(42.1362984310705,-6.28219522128395,6.19374010119023E-5));
#64614=CARTESIAN_POINT('',(41.9500381542954,-6.28216889122489,-3.39632393438963E-5));
#64615=CARTESIAN_POINT('',(37.,-6.28269,-7.69407619853508E-16));
#64616=CARTESIAN_POINT('Ctrl Pts',(42.1362984310705,-6.28219522128395,6.19374010119023E-5));
#64617=CARTESIAN_POINT('Ctrl Pts',(42.1217495525563,-6.28235233139332,0.452376781104032));
#64618=CARTESIAN_POINT('Ctrl Pts',(42.1072006740422,-6.23417154886657,0.904658649178573));
#64619=CARTESIAN_POINT('Ctrl Pts',(42.092651795528,-6.13730307499778,1.34626053023583));
#64620=CARTESIAN_POINT('Ctrl Pts',(42.0591284922087,-5.91410021929876,2.36379282941863));
#64621=CARTESIAN_POINT('Ctrl Pts',(42.0256051888895,-5.43240140354768,3.32462222441192));
#64622=CARTESIAN_POINT('Ctrl Pts',(41.9920818855702,-4.7506124018243,4.11224856462754));
#64623=CARTESIAN_POINT('Ctrl Pts',(41.9585585822509,-4.06882340010089,4.89987490484318));
#64624=CARTESIAN_POINT('Ctrl Pts',(41.9250352789317,-3.18694421240517,5.51429819028114));
#64625=CARTESIAN_POINT('Ctrl Pts',(41.8915119756124,-2.21190231067177,5.88101986203864));
#64626=CARTESIAN_POINT('Ctrl Pts',(41.8579886722932,-1.23686040893839,6.24774153379614));
#64627=CARTESIAN_POINT('Ctrl Pts',(41.8244653689739,-0.168655793167334,
6.36676159187319));
#64628=CARTESIAN_POINT('Ctrl Pts',(41.7909420656546,0.86319218674972,6.22364890545589));
#64629=CARTESIAN_POINT('Ctrl Pts',(41.7574187623353,1.89504016666674,6.0805362190386));
#64630=CARTESIAN_POINT('Ctrl Pts',(41.7238954590161,2.89053151072977,5.67529078812696));
#64631=CARTESIAN_POINT('Ctrl Pts',(41.6903721556968,3.72896332194492,5.05704844679558));
#64632=CARTESIAN_POINT('Ctrl Pts',(41.6568488523775,4.56739513316007,4.4388061054642));
#64633=CARTESIAN_POINT('Ctrl Pts',(41.6233255490583,5.24876741152739,3.60756685371299));
#64634=CARTESIAN_POINT('Ctrl Pts',(41.589802245739,5.69046406156712,2.66411809303964));
#64635=CARTESIAN_POINT('Ctrl Pts',(41.5562789424197,6.13216071160688,1.72066933236623));
#64636=CARTESIAN_POINT('Ctrl Pts',(41.5227556391005,6.33418173331909,0.66501106277067));
#64637=CARTESIAN_POINT('Ctrl Pts',(41.4892323357812,6.27203216477392,-0.374858604929178));
#64638=CARTESIAN_POINT('Ctrl Pts',(41.4557090324619,6.20988259622875,-1.41472827262897));
#64639=CARTESIAN_POINT('Ctrl Pts',(41.4221857291426,5.88356243742621,-2.43880933843296));
#64640=CARTESIAN_POINT('Ctrl Pts',(41.3886624258234,5.33263786716822,-3.32293241389162));
#64641=CARTESIAN_POINT('Ctrl Pts',(41.3551391225041,4.78171329691024,-4.20705548935028));
#64642=CARTESIAN_POINT('Ctrl Pts',(41.3216158191849,4.00618431519681,-4.95122057446359));
#64643=CARTESIAN_POINT('Ctrl Pts',(41.2880925158656,3.10008347726189,-5.4651979729609));
#64644=CARTESIAN_POINT('Ctrl Pts',(41.2545692125463,2.19398263932697,-5.97917537145821));
#64645=CARTESIAN_POINT('Ctrl Pts',(41.2210459092271,1.15730994517057,-6.26296508333951));
#64646=CARTESIAN_POINT('Ctrl Pts',(41.1875226059078,0.115761512760339,-6.28215772818636));
#64647=CARTESIAN_POINT('Ctrl Pts',(41.1539993025885,-0.92578691964992,-6.30135037303321));
#64648=CARTESIAN_POINT('Ctrl Pts',(41.1204759992693,-1.972211090314,-6.05594595084558));
#64649=CARTESIAN_POINT('Ctrl Pts',(41.08695269595,-2.89663251893485,-5.57569964218817));
#64650=CARTESIAN_POINT('Ctrl Pts',(41.0534293926307,-3.82105394755572,-5.09545333353073));
#64651=CARTESIAN_POINT('Ctrl Pts',(41.0199060893115,-4.62347263413335,-4.38036513840349));
#64652=CARTESIAN_POINT('Ctrl Pts',(40.9863827859922,-5.20659565829271,-3.51713919268141));
#64653=CARTESIAN_POINT('Ctrl Pts',(40.9528594826729,-5.78971868245205,-2.65391324695935));
#64654=CARTESIAN_POINT('Ctrl Pts',(40.9193361793536,-6.15354604419313,-1.64254955064245));
#64655=CARTESIAN_POINT('Ctrl Pts',(40.8858128760344,-6.25396383250134,-0.60567551660371));
#64656=CARTESIAN_POINT('Ctrl Pts',(40.8793080610464,-6.27344875999268,-0.404481926192384));
#64657=CARTESIAN_POINT('Ctrl Pts',(40.8728032460584,-6.28301605891263,-0.202327846566644));
#64658=CARTESIAN_POINT('Ctrl Pts',(40.8662984310705,-6.28281011036189,-0.000154357209955491));
#64659=CARTESIAN_POINT('Ctrl Pts',(40.6800381542954,-6.28310564591676,-9.39174517631389E-5));
#64660=CARTESIAN_POINT('Ctrl Pts',(40.6831383540389,-6.2831754357796,-0.096436854650988));
#64661=CARTESIAN_POINT('Ctrl Pts',(40.6862385537824,-6.28100506553998,-0.192776646053021));
#64662=CARTESIAN_POINT('Ctrl Pts',(40.6893387535259,-6.27657377857455,-0.289012330845967));
#64663=CARTESIAN_POINT('Ctrl Pts',(40.7228620568452,-6.22865706696617,-1.3296349740264));
#64664=CARTESIAN_POINT('Ctrl Pts',(40.7563853601644,-5.91637847768878,-2.35808475902857));
#64665=CARTESIAN_POINT('Ctrl Pts',(40.7899086634837,-5.37760165528307,-3.24966259208051));
#64666=CARTESIAN_POINT('Ctrl Pts',(40.8234319668029,-4.83882483287737,-4.14124042513245));
#64667=CARTESIAN_POINT('Ctrl Pts',(40.8569552701222,-4.07354977734334,-4.89594630623416));
#64668=CARTESIAN_POINT('Ctrl Pts',(40.8904785734415,-3.17456575977914,-5.42227247213828));
#64669=CARTESIAN_POINT('Ctrl Pts',(40.9240018767608,-2.275581742215,-5.94859863804237));
#64670=CARTESIAN_POINT('Ctrl Pts',(40.95752518008,-1.24288876262071,-6.24654508874889));
#64671=CARTESIAN_POINT('Ctrl Pts',(40.9910484833993,-0.201700400286187,
-6.27998594535012));
#64672=CARTESIAN_POINT('Ctrl Pts',(41.0245717867186,0.839487962048451,-6.31342680195135));
#64673=CARTESIAN_POINT('Ctrl Pts',(41.0580950900378,1.88917170712332,-6.08236206444723));
#64674=CARTESIAN_POINT('Ctrl Pts',(41.0916183933571,2.820077132647,-5.61480823280655));
#64675=CARTESIAN_POINT('Ctrl Pts',(41.1251416966764,3.7509825581706,-5.1472544011659));
#64676=CARTESIAN_POINT('Ctrl Pts',(41.1586649999956,4.56310966414304,-4.44321147538874));
#64677=CARTESIAN_POINT('Ctrl Pts',(41.1921883033149,5.15798838851631,-3.58804435719538));
#64678=CARTESIAN_POINT('Ctrl Pts',(41.2257116066342,5.75286711288959,-2.73287723900201));
#64679=CARTESIAN_POINT('Ctrl Pts',(41.2592349099534,6.1304974556637,-1.72658592839243));
#64680=CARTESIAN_POINT('Ctrl Pts',(41.2927582132727,6.2450919003148,-0.691182813655839));
#64681=CARTESIAN_POINT('Ctrl Pts',(41.326281516592,6.3596863449659,0.344220301080751));
#64682=CARTESIAN_POINT('Ctrl Pts',(41.3598048199112,6.21124489149398,1.40873521994435));
#64683=CARTESIAN_POINT('Ctrl Pts',(41.3933281232305,5.8177660022412,2.37328996720524));
#64684=CARTESIAN_POINT('Ctrl Pts',(41.4268514265498,5.4242871129884,3.33784471446619));
#64685=CARTESIAN_POINT('Ctrl Pts',(41.460374729869,4.7857707879547,4.20243929012441));
#64686=CARTESIAN_POINT('Ctrl Pts',(41.4938980331883,3.97963685672385,4.86224197401525));
#64687=CARTESIAN_POINT('Ctrl Pts',(41.5274213365076,3.17350292549306,5.52204465790606));
#64688=CARTESIAN_POINT('Ctrl Pts',(41.5609446398268,2.19975138806514,5.9770554500295));
#64689=CARTESIAN_POINT('Ctrl Pts',(41.5944679431461,1.17644919923661,6.17210448768378));
#64690=CARTESIAN_POINT('Ctrl Pts',(41.6279912464654,0.153147010408017,6.36715352533808));
#64691=CARTESIAN_POINT('Ctrl Pts',(41.6615145497846,-0.919705829821191,
6.30224080852317));
#64692=CARTESIAN_POINT('Ctrl Pts',(41.6950378531039,-1.91202637634447,5.98523697621353));
#64693=CARTESIAN_POINT('Ctrl Pts',(41.7285611564232,-2.90434692286771,5.6682331439039));
#64694=CARTESIAN_POINT('Ctrl Pts',(41.7620844597424,-3.81613517568503,5.09913819609954));
#64695=CARTESIAN_POINT('Ctrl Pts',(41.7956077630617,-4.53683720158905,4.3469546502751));
#64696=CARTESIAN_POINT('Ctrl Pts',(41.829131066381,-5.25753922749303,3.5947711044507));
#64697=CARTESIAN_POINT('Ctrl Pts',(41.8626543697003,-5.78715502648374,2.65949896060625));
#64698=CARTESIAN_POINT('Ctrl Pts',(41.8961776730195,-6.06146891088779,1.65453956362833));
#64699=CARTESIAN_POINT('Ctrl Pts',(41.9141311667782,-6.20837843721501,1.11633090055299));
#64700=CARTESIAN_POINT('Ctrl Pts',(41.9320846605368,-6.28206312737231,0.558134773999001));
#64701=CARTESIAN_POINT('Ctrl Pts',(41.9500381542954,-6.28216889122489,-3.39632393438963E-5));
#64702=CARTESIAN_POINT('Origin',(37.,0.,0.));
#64703=CARTESIAN_POINT('',(43.4062984310705,-6.2831673517952,6.56348350827965E-5));
#64704=CARTESIAN_POINT('',(43.2200381542954,-6.28290773611714,0.000142516273084187));
#64705=CARTESIAN_POINT('',(37.,-6.28269,-7.69407619853508E-16));
#64706=CARTESIAN_POINT('Ctrl Pts',(43.4062984310705,-6.2831673517952,6.56348350827965E-5));
#64707=CARTESIAN_POINT('Ctrl Pts',(43.4042191623735,-6.28320215738342,0.0646799042948801));
#64708=CARTESIAN_POINT('Ctrl Pts',(43.4021398936764,-6.28222608018872,0.129293120214478));
#64709=CARTESIAN_POINT('Ctrl Pts',(43.4000606249794,-6.28023239731441,0.193874921974653));
#64710=CARTESIAN_POINT('Ctrl Pts',(43.3665373216601,-6.24808896351293,1.23510414473776));
#64711=CARTESIAN_POINT('Ctrl Pts',(43.3330140183409,-5.95142955534036,2.26816758466867));
#64712=CARTESIAN_POINT('Ctrl Pts',(43.2994907150216,-5.42622399835116,3.16780674432107));
#64713=CARTESIAN_POINT('Ctrl Pts',(43.2659674117023,-4.90101844136195,4.06744590397347));
#64714=CARTESIAN_POINT('Ctrl Pts',(43.2324441083831,-4.14726673555611,4.83366078334737));
#64715=CARTESIAN_POINT('Ctrl Pts',(43.1989208050638,-3.25636095083704,5.37354815810855));
#64716=CARTESIAN_POINT('Ctrl Pts',(43.1653975017446,-2.36545516611797,5.91343553286973));
#64717=CARTESIAN_POINT('Ctrl Pts',(43.1318741984253,-1.33739530248567,6.2269954030182));
#64718=CARTESIAN_POINT('Ctrl Pts',(43.098350895106,-0.296833175913861,6.27620876925911));
#64719=CARTESIAN_POINT('Ctrl Pts',(43.0648275917867,0.74372895065801,6.32542213550003));
#64720=CARTESIAN_POINT('Ctrl Pts',(43.0313042884675,1.79679334016941,6.11028899783336));
#64721=CARTESIAN_POINT('Ctrl Pts',(42.9977809851482,2.73467638864608,5.65689415660482));
#64722=CARTESIAN_POINT('Ctrl Pts',(42.964257681829,3.67255943712274,5.20349931537627));
#64723=CARTESIAN_POINT('Ctrl Pts',(42.9307343785097,4.49526114456468,4.51184277058584));
#64724=CARTESIAN_POINT('Ctrl Pts',(42.8972110751904,5.10302928304715,3.66578758059048));
#64725=CARTESIAN_POINT('Ctrl Pts',(42.8636877718711,5.71079742152959,2.81973239059516));
#64726=CARTESIAN_POINT('Ctrl Pts',(42.8301644685519,6.10363199105259,1.81927855539492));
#64727=CARTESIAN_POINT('Ctrl Pts',(42.7966411652326,6.23390196914313,0.785730671898131));
#64728=CARTESIAN_POINT('Ctrl Pts',(42.7631178619133,6.36417194723367,-0.247817211598693));
#64729=CARTESIAN_POINT('Ctrl Pts',(42.7295945585941,6.23187733389174,-1.31445914339201));
#64730=CARTESIAN_POINT('Ctrl Pts',(42.6960712552748,5.85305879404355,-2.28486524835001));
#64731=CARTESIAN_POINT('Ctrl Pts',(42.6625479519555,5.47424025419536,-3.25527135330798));
#64732=CARTESIAN_POINT('Ctrl Pts',(42.6290246486363,4.84889778784092,-4.12944163143057));
#64733=CARTESIAN_POINT('Ctrl Pts',(42.595501345317,4.05285389986933,-4.80138331275082));
#64734=CARTESIAN_POINT('Ctrl Pts',(42.5619780419977,3.25681001189774,-5.47332499407108));
#64735=CARTESIAN_POINT('Ctrl Pts',(42.5284547386785,2.29006470230899,-5.94303807858901));
#64736=CARTESIAN_POINT('Ctrl Pts',(42.4949314353592,1.2698354237897,-6.15357005697805));
#64737=CARTESIAN_POINT('Ctrl Pts',(42.4614081320399,0.249606145270341,-6.36410203536712));
#64738=CARTESIAN_POINT('Ctrl Pts',(42.4278848287207,-0.82410710217959,-6.31545290762728));
#64739=CARTESIAN_POINT('Ctrl Pts',(42.3943615254014,-1.82111704944835,-6.0135213595577));
#64740=CARTESIAN_POINT('Ctrl Pts',(42.3608382220821,-2.8181269967171,-5.71158981148812));
#64741=CARTESIAN_POINT('Ctrl Pts',(42.3273149187629,-3.7384336438047,-5.1563758430888));
#64742=CARTESIAN_POINT('Ctrl Pts',(42.2937916154436,-4.47045020586492,-4.41519890905613));
#64743=CARTESIAN_POINT('Ctrl Pts',(42.2602683121243,-5.20246676792509,-3.67402197502349));
#64744=CARTESIAN_POINT('Ctrl Pts',(42.2267450088051,-5.74619324495793,-2.74688207535751));
#64745=CARTESIAN_POINT('Ctrl Pts',(42.1932217054858,-6.03570303565085,-1.74619452383838));
#64746=CARTESIAN_POINT('Ctrl Pts',(42.1742472806807,-6.19956760775252,-1.17979835103651));
#64747=CARTESIAN_POINT('Ctrl Pts',(42.1552728558756,-6.28199032068262,-0.589840162731772));
#64748=CARTESIAN_POINT('Ctrl Pts',(42.1362984310705,-6.28219522128395,6.19374010119023E-5));
#64749=CARTESIAN_POINT('Ctrl Pts',(41.9500381542954,-6.28216889122489,-3.39632393438963E-5));
#64750=CARTESIAN_POINT('Ctrl Pts',(41.965607963856,-6.28226061281764,-0.484094673557285));
#64751=CARTESIAN_POINT('Ctrl Pts',(41.9811777734167,-6.22701450793077,-0.968134784699993));
#64752=CARTESIAN_POINT('Ctrl Pts',(41.9967475829773,-6.11619962718259,-1.43909994292342));
#64753=CARTESIAN_POINT('Ctrl Pts',(42.0302708862965,-5.87760448925595,-2.45313340238563));
#64754=CARTESIAN_POINT('Ctrl Pts',(42.0637941896158,-5.38140224358531,-3.40655367119862));
#64755=CARTESIAN_POINT('Ctrl Pts',(42.0973174929351,-4.68775719888566,-4.18375895213459));
#64756=CARTESIAN_POINT('Ctrl Pts',(42.1308407962544,-3.99411215418602,-4.96096423307055));
#64757=CARTESIAN_POINT('Ctrl Pts',(42.1643640995736,-3.10302431045737,-5.56195452612949));
#64758=CARTESIAN_POINT('Ctrl Pts',(42.1978874028929,-2.12253768521484,-5.91386001695285));
#64759=CARTESIAN_POINT('Ctrl Pts',(42.2314107062122,-1.1420510599723,-6.2657655077762));
#64760=CARTESIAN_POINT('Ctrl Pts',(42.2649340095314,-0.0721656532158725,
-6.36858619636397));
#64761=CARTESIAN_POINT('Ctrl Pts',(42.2984573128507,0.957395389979257,-6.20985511848039));
#64762=CARTESIAN_POINT('Ctrl Pts',(42.33198061617,1.98695643317445,-6.0511240405968));
#64763=CARTESIAN_POINT('Ctrl Pts',(42.3655039194892,2.97619311280833,-5.63084119624184));
#64764=CARTESIAN_POINT('Ctrl Pts',(42.3990272228085,3.80516090725694,-4.99996569939777));
#64765=CARTESIAN_POINT('Ctrl Pts',(42.4325505261278,4.63412870170551,-4.36909020255373));
#64766=CARTESIAN_POINT('Ctrl Pts',(42.466073829447,5.30282761096882,-3.52762205322063));
#64767=CARTESIAN_POINT('Ctrl Pts',(42.4995971327663,5.73017818011631,-2.57758890232512));
#64768=CARTESIAN_POINT('Ctrl Pts',(42.5331204360856,6.15752874926381,-1.62755575142959));
#64769=CARTESIAN_POINT('Ctrl Pts',(42.5666437394049,6.34353097829547,-0.568957598971652));
#64770=CARTESIAN_POINT('Ctrl Pts',(42.6001670427241,6.26563217699923,0.469850984698985));
#64771=CARTESIAN_POINT('Ctrl Pts',(42.6336903460434,6.18773337570298,1.50865956836962));
#64772=CARTESIAN_POINT('Ctrl Pts',(42.6672136493627,5.84593354407884,2.52767858325296));
#64773=CARTESIAN_POINT('Ctrl Pts',(42.7007369526819,5.28167576459567,3.40335241239479));
#64774=CARTESIAN_POINT('Ctrl Pts',(42.7342602560012,4.71741798511252,4.27902624153659));
#64775=CARTESIAN_POINT('Ctrl Pts',(42.7677835593204,3.93070225777035,5.01135488493689));
#64776=CARTESIAN_POINT('Ctrl Pts',(42.8013068626397,3.01691752589568,5.51154380978815));
#64777=CARTESIAN_POINT('Ctrl Pts',(42.834830165959,2.10313279402099,6.01173273463943));
#64778=CARTESIAN_POINT('Ctrl Pts',(42.8683534692782,1.06227905761378,6.27978194094166));
#64779=CARTESIAN_POINT('Ctrl Pts',(42.9018767725975,0.0205593842150595,
6.28319057780292));
#64780=CARTESIAN_POINT('Ctrl Pts',(42.9354000759168,-1.02116028918366,6.28659921466418));
#64781=CARTESIAN_POINT('Ctrl Pts',(42.9689233792361,-2.06374589957381,6.02536728208448));
#64782=CARTESIAN_POINT('Ctrl Pts',(43.0024466825553,-2.98078439043953,5.53116903945113));
#64783=CARTESIAN_POINT('Ctrl Pts',(43.0359699858746,-3.89782288130523,5.03697079681779));
#64784=CARTESIAN_POINT('Ctrl Pts',(43.0694932891938,-4.6893142526465,4.30980624413073));
#64785=CARTESIAN_POINT('Ctrl Pts',(43.1030165925131,-5.2592905163573,3.43784377042135));
#64786=CARTESIAN_POINT('Ctrl Pts',(43.1365398958324,-5.82926678006814,2.56588129671191));
#64787=CARTESIAN_POINT('Ctrl Pts',(43.1700631991517,-6.17772793614856,1.54912090198006));
#64788=CARTESIAN_POINT('Ctrl Pts',(43.2035865024709,-6.2624232194065,0.510844346458796));
#64789=CARTESIAN_POINT('Ctrl Pts',(43.2090703864124,-6.27627803256008,0.34099866999205));
#64790=CARTESIAN_POINT('Ctrl Pts',(43.2145542703539,-6.2830745231639,0.170577225321256));
#64791=CARTESIAN_POINT('Ctrl Pts',(43.2200381542954,-6.28290773611714,0.000142516273084187));
#64792=CARTESIAN_POINT('Origin',(37.,0.,0.));
#64793=CARTESIAN_POINT('',(44.6762984310705,-6.28244611237991,-0.000146669898813401));
#64794=CARTESIAN_POINT('',(44.4900381542954,-6.28276315662069,-0.000157922487962832));
#64795=CARTESIAN_POINT('',(37.,-6.28269,-7.69407619853508E-16));
#64796=CARTESIAN_POINT('Ctrl Pts',(44.6762984310705,-6.28244611237991,-0.000146669898813401));
#64797=CARTESIAN_POINT('Ctrl Pts',(44.6531654688713,-6.28182129015504,0.718959259511916));
#64798=CARTESIAN_POINT('Ctrl Pts',(44.6300325066722,-6.15849154096994,1.43827402723654));
#64799=CARTESIAN_POINT('Ctrl Pts',(44.606899544473,-5.91650025717146,2.11516693349206));
#64800=CARTESIAN_POINT('Ctrl Pts',(44.5733762411537,-5.56581679789122,3.09609129655964));
#64801=CARTESIAN_POINT('Ctrl Pts',(44.5398529378345,-4.96593733257438,3.98792732547428));
#64802=CARTESIAN_POINT('Ctrl Pts',(44.5063296345153,-4.18959698819389,4.6825402855891));
#64803=CARTESIAN_POINT('Ctrl Pts',(44.472806331196,-3.41325664381335,5.37715324570395));
#64804=CARTESIAN_POINT('Ctrl Pts',(44.4392830278767,-2.46045542036912,5.87454313701897));
#64805=CARTESIAN_POINT('Ctrl Pts',(44.4057597245574,-1.44672005610452,6.11440164929595));
#64806=CARTESIAN_POINT('Ctrl Pts',(44.3722364212382,-0.432984691839915,
6.35426016157292));
#64807=CARTESIAN_POINT('Ctrl Pts',(44.3387131179189,0.641684813245083,6.33658729481186));
#64808=CARTESIAN_POINT('Ctrl Pts',(44.3051898145996,1.64698524421207,6.06352587650088));
#64809=CARTESIAN_POINT('Ctrl Pts',(44.2716665112804,2.65228567517911,5.79046445818989));
#64810=CARTESIAN_POINT('Ctrl Pts',(44.2381432079611,3.58821703202816,5.26201448832894));
#64811=CARTESIAN_POINT('Ctrl Pts',(44.2046199046418,4.34129804057951,4.54225029831125));
#64812=CARTESIAN_POINT('Ctrl Pts',(44.1710966013226,5.09437904913085,3.82248610829356));
#64813=CARTESIAN_POINT('Ctrl Pts',(44.1375732980033,5.66460970938452,2.91140769811911));
#64814=CARTESIAN_POINT('Ctrl Pts',(44.104049994684,5.98284979922019,1.91948293288038));
#64815=CARTESIAN_POINT('Ctrl Pts',(44.0705266913647,6.30108988905583,0.927558167641697));
#64816=CARTESIAN_POINT('Ctrl Pts',(44.0370033880455,6.36733940847352,-0.145212952661282));
#64817=CARTESIAN_POINT('Ctrl Pts',(44.0034800847262,6.17356563175858,-1.16875739142789));
#64818=CARTESIAN_POINT('Ctrl Pts',(43.969956781407,5.97979185504364,-2.19230183019453));
#64819=CARTESIAN_POINT('Ctrl Pts',(43.9364334780877,5.52599478219611,-3.16661958742472));
#64820=CARTESIAN_POINT('Ctrl Pts',(43.9029101747684,4.86719711297792,-3.97357505441478));
#64821=CARTESIAN_POINT('Ctrl Pts',(43.8693868714492,4.20839944375971,-4.78053052140487));
#64822=CARTESIAN_POINT('Ctrl Pts',(43.8358635681299,3.34460117817085,-5.42012369815475));
#64823=CARTESIAN_POINT('Ctrl Pts',(43.8023402648106,2.38053748412285,-5.81480418727356));
#64824=CARTESIAN_POINT('Ctrl Pts',(43.7688169614914,1.41647379007491,-6.20948467639234));
#64825=CARTESIAN_POINT('Ctrl Pts',(43.7352936581721,0.352144667567816,-6.35925247788009));
#64826=CARTESIAN_POINT('Ctrl Pts',(43.7017703548528,-0.683400435396939,
-6.24594831026861));
#64827=CARTESIAN_POINT('Ctrl Pts',(43.6682470515336,-1.71894553836169,-6.13264414265714));
#64828=CARTESIAN_POINT('Ctrl Pts',(43.6347237482143,-2.72570662178413,-5.75626800594644));
#64829=CARTESIAN_POINT('Ctrl Pts',(43.601200444895,-3.58161433762367,-5.16245534471501));
#64830=CARTESIAN_POINT('Ctrl Pts',(43.5676771415757,-4.43752205346327,-4.56864268348355));
#64831=CARTESIAN_POINT('Ctrl Pts',(43.5341538382565,-5.14257640171996,-3.75739349773132));
#64832=CARTESIAN_POINT('Ctrl Pts',(43.5006305349372,-5.61128984613312,-2.82707140205752));
#64833=CARTESIAN_POINT('Ctrl Pts',(43.469186500315,-6.05093153757615,-1.95445214053635));
#64834=CARTESIAN_POINT('Ctrl Pts',(43.4377424656927,-6.28264099937016,-0.977072783542306));
#64835=CARTESIAN_POINT('Ctrl Pts',(43.4062984310705,-6.2831673517952,6.56348350827965E-5));
#64836=CARTESIAN_POINT('Ctrl Pts',(43.2200381542954,-6.28290773611714,0.000142516273084187));
#64837=CARTESIAN_POINT('Ctrl Pts',(43.2480775736732,-6.2820549441907,-0.871300120826209));
#64838=CARTESIAN_POINT('Ctrl Pts',(43.276116993051,-6.09915862784975,-1.74308953341376));
#64839=CARTESIAN_POINT('Ctrl Pts',(43.3041564124287,-5.7469236826231,-2.5400343917704));
#64840=CARTESIAN_POINT('Ctrl Pts',(43.337679715748,-5.32579945214628,-3.49284385816776));
#64841=CARTESIAN_POINT('Ctrl Pts',(43.3712030190673,-4.66262158075713,-4.33867007465187));
#64842=CARTESIAN_POINT('Ctrl Pts',(43.4047263223865,-3.83780009992036,-4.97495697652974));
#64843=CARTESIAN_POINT('Ctrl Pts',(43.4382496257058,-3.01297861908352,-5.61124387840767));
#64844=CARTESIAN_POINT('Ctrl Pts',(43.4717729290251,-2.02651352879907,-6.03799146567932));
#64845=CARTESIAN_POINT('Ctrl Pts',(43.5052962323443,-0.998013296675183,
-6.20345677706633));
#64846=CARTESIAN_POINT('Ctrl Pts',(43.5388195356636,0.0304869354486183,
-6.36892208845333));
#64847=CARTESIAN_POINT('Ctrl Pts',(43.5723428389829,1.10102230941182,-6.2731051239557));
#64848=CARTESIAN_POINT('Ctrl Pts',(43.6058661423021,2.08379087189511,-5.92762364927779));
#64849=CARTESIAN_POINT('Ctrl Pts',(43.6393894456214,3.06655943437841,-5.58214217459987));
#64850=CARTESIAN_POINT('Ctrl Pts',(43.6729127489407,3.96156118538184,-4.98699618974166));
#64851=CARTESIAN_POINT('Ctrl Pts',(43.7064360522599,4.6602775478178,-4.21434688920786));
#64852=CARTESIAN_POINT('Ctrl Pts',(43.7399593555792,5.3589939102538,-3.44169758867402));
#64853=CARTESIAN_POINT('Ctrl Pts',(43.7734826588984,5.86142488412234,-2.49154497246454));
#64854=CARTESIAN_POINT('Ctrl Pts',(43.8070059622177,6.10665093009532,-1.47909463633556));
#64855=CARTESIAN_POINT('Ctrl Pts',(43.840529265537,6.3518769760683,-0.466644300206603));
#64856=CARTESIAN_POINT('Ctrl Pts',(43.8740525688563,6.33989809414575,0.608103755841807));
#64857=CARTESIAN_POINT('Ctrl Pts',(43.9075758721756,6.07216671860491,1.6148367926009));
#64858=CARTESIAN_POINT('Ctrl Pts',(43.9410991754948,5.80443534306408,2.62156982935996));
#64859=CARTESIAN_POINT('Ctrl Pts',(43.974622478814,5.28095147390495,3.56028784682966));
#64860=CARTESIAN_POINT('Ctrl Pts',(44.0081457821333,4.56518730494811,4.31717168942946));
#64861=CARTESIAN_POINT('Ctrl Pts',(44.0416690854526,3.84942313599124,5.07405553202931));
#64862=CARTESIAN_POINT('Ctrl Pts',(44.0751923887719,2.94137866723662,5.64910519975927));
#64863=CARTESIAN_POINT('Ctrl Pts',(44.1087156920912,1.95115389968543,5.97259616791668));
#64864=CARTESIAN_POINT('Ctrl Pts',(44.1422389954104,0.960929132134289,6.29608713607408));
#64865=CARTESIAN_POINT('Ctrl Pts',(44.1757622987296,-0.111475934213448,
6.36801940465896));
#64866=CARTESIAN_POINT('Ctrl Pts',(44.2092856020489,-1.13603264664161,6.17967121706609));
#64867=CARTESIAN_POINT('Ctrl Pts',(44.2428089053682,-2.16058935906979,5.99132302947322));
#64868=CARTESIAN_POINT('Ctrl Pts',(44.2763322086875,-3.13729771757836,5.54269438570263));
#64869=CARTESIAN_POINT('Ctrl Pts',(44.3098555120068,-3.94773225408754,4.88818131571524));
#64870=CARTESIAN_POINT('Ctrl Pts',(44.343378815326,-4.75816679059674,4.23366824572783));
#64871=CARTESIAN_POINT('Ctrl Pts',(44.3769021186452,-5.4023275051065,3.37327074952362));
#64872=CARTESIAN_POINT('Ctrl Pts',(44.4104254219645,-5.80211018823849,2.41131165318998));
#64873=CARTESIAN_POINT('Ctrl Pts',(44.4369629994081,-6.11858448712231,1.64980960867396));
#64874=CARTESIAN_POINT('Ctrl Pts',(44.4635005768518,-6.28191792026545,0.824663417087317));
#64875=CARTESIAN_POINT('Ctrl Pts',(44.4900381542954,-6.28276315662069,-0.000157922487962832));
#64876=CARTESIAN_POINT('Origin',(37.,0.,0.));
#64877=CARTESIAN_POINT('',(45.9462984310705,-6.28242372114921,0.000143169579051167));
#64878=CARTESIAN_POINT('',(45.7600381542954,-6.28221291207239,7.44799067214229E-5));
#64879=CARTESIAN_POINT('',(37.,-6.28269,-7.69407619853508E-16));
#64880=CARTESIAN_POINT('Ctrl Pts',(45.9462984310705,-6.28242372114921,0.000143169579051167));
#64881=CARTESIAN_POINT('Ctrl Pts',(45.9356350786884,-6.28270336338794,0.331625072851757));
#64882=CARTESIAN_POINT('Ctrl Pts',(45.9249717263064,-6.25692034458445,0.663063898107308));
#64883=CARTESIAN_POINT('Ctrl Pts',(45.9143083739244,-6.20469555259325,0.990282560321853));
#64884=CARTESIAN_POINT('Ctrl Pts',(45.8807850706052,-6.04051195629183,2.01898817485789));
#64885=CARTESIAN_POINT('Ctrl Pts',(45.8472617672859,-5.61499390834304,3.00598425704312));
#64886=CARTESIAN_POINT('Ctrl Pts',(45.8137384639667,-4.97973528891159,3.8315979567299));
#64887=CARTESIAN_POINT('Ctrl Pts',(45.7802151606474,-4.34447666948014,4.65721165641667));
#64888=CARTESIAN_POINT('Ctrl Pts',(45.7466918573281,-3.49947747856605,5.32144297360496));
#64889=CARTESIAN_POINT('Ctrl Pts',(45.7131685540089,-2.54719350436786,5.74375414698038));
#64890=CARTESIAN_POINT('Ctrl Pts',(45.6796452506896,-1.59490953016972,6.16606532035578));
#64891=CARTESIAN_POINT('Ctrl Pts',(45.6461219473703,-0.535340772687518,
6.34645634991833));
#64892=CARTESIAN_POINT('Ctrl Pts',(45.6125986440511,0.503040512287664,6.26305490097647));
#64893=CARTESIAN_POINT('Ctrl Pts',(45.5790753407318,1.54142179726296,6.17965345203461));
#64894=CARTESIAN_POINT('Ctrl Pts',(45.5455520374125,2.5586156097312,5.83245952458827));
#64895=CARTESIAN_POINT('Ctrl Pts',(45.5120287340933,3.43128763774544,5.26357023290308));
#64896=CARTESIAN_POINT('Ctrl Pts',(45.478505430774,4.30395966575968,4.69468094121789));
#64897=CARTESIAN_POINT('Ctrl Pts',(45.4449821274547,5.03210990931988,3.90409628529387));
#64898=CARTESIAN_POINT('Ctrl Pts',(45.4114588241355,5.52745046480069,2.9876743143828));
#64899=CARTESIAN_POINT('Ctrl Pts',(45.3779355208162,6.0227910202815,2.07125234347174));
#64900=CARTESIAN_POINT('Ctrl Pts',(45.3444122174969,6.28532188768291,1.02899305757366));
#64901=CARTESIAN_POINT('Ctrl Pts',(45.3108889141777,6.28321131232954,-0.0127300534996296));
#64902=CARTESIAN_POINT('Ctrl Pts',(45.2773656108584,6.28110073697618,-1.0544531645728));
#64903=CARTESIAN_POINT('Ctrl Pts',(45.2438423075391,6.01434871886806,-2.09564010082135));
#64904=CARTESIAN_POINT('Ctrl Pts',(45.2103190042198,5.51529882538695,-3.01004739436664));
#64905=CARTESIAN_POINT('Ctrl Pts',(45.1767957009006,5.01624893190582,-3.92445468791197));
#64906=CARTESIAN_POINT('Ctrl Pts',(45.1432723975813,4.28490116305167,-4.71208233875417));
#64907=CARTESIAN_POINT('Ctrl Pts',(45.1097490942621,3.40993112101547,-5.27743083323489));
#64908=CARTESIAN_POINT('Ctrl Pts',(45.0762257909428,2.53496107897927,-5.8427793277156));
#64909=CARTESIAN_POINT('Ctrl Pts',(45.0427024876235,1.51636876376106,-6.18584866583481));
#64910=CARTESIAN_POINT('Ctrl Pts',(45.0091791843042,0.477658055164268,-6.26504183800753));
#64911=CARTESIAN_POINT('Ctrl Pts',(44.975655880985,-0.561052653432527,-6.34423501018025));
#64912=CARTESIAN_POINT('Ctrl Pts',(44.9421325776657,-1.61988175540787,-6.15955201640649));
#64913=CARTESIAN_POINT('Ctrl Pts',(44.9086092743465,-2.57044667788251,-5.73338559019109));
#64914=CARTESIAN_POINT('Ctrl Pts',(44.8750859710272,-3.52101160035721,-5.30721916397567));
#64915=CARTESIAN_POINT('Ctrl Pts',(44.8415626677079,-4.36331234333117,-4.6395693053186));
#64916=CARTESIAN_POINT('Ctrl Pts',(44.8080393643886,-4.99522030425713,-3.81138827221596));
#64917=CARTESIAN_POINT('Ctrl Pts',(44.7745160610694,-5.6271282651831,-2.98320723911332));
#64918=CARTESIAN_POINT('Ctrl Pts',(44.7409927577501,-6.04864344406104,-1.99449503156515));
#64919=CARTESIAN_POINT('Ctrl Pts',(44.7074694544309,-6.2086573068782,-0.96513257918072));
#64920=CARTESIAN_POINT('Ctrl Pts',(44.6970791133107,-6.25825261682677,-0.646088035310425));
#64921=CARTESIAN_POINT('Ctrl Pts',(44.6866887721906,-6.28272675590493,-0.32313841837267));
#64922=CARTESIAN_POINT('Ctrl Pts',(44.6762984310705,-6.28244611237991,-0.000146669898813401));
#64923=CARTESIAN_POINT('Ctrl Pts',(44.4900381542954,-6.28276315662069,-0.000157922487962832));
#64924=CARTESIAN_POINT('Ctrl Pts',(44.4970238801711,-6.28298565581039,-0.217283083474969));
#64925=CARTESIAN_POINT('Ctrl Pts',(44.5040096060467,-6.27194857089511,-0.434385733912797));
#64926=CARTESIAN_POINT('Ctrl Pts',(44.5109953319224,-6.24948139636436,-0.650299009507491));
#64927=CARTESIAN_POINT('Ctrl Pts',(44.5445186352416,-6.14166526960405,-1.68642987940837));
#64928=CARTESIAN_POINT('Ctrl Pts',(44.5780419385609,-5.77062836432919,-2.69517092274707));
#64929=CARTESIAN_POINT('Ctrl Pts',(44.6115652418801,-5.18135874560474,-3.55421272219544));
#64930=CARTESIAN_POINT('Ctrl Pts',(44.6450885451994,-4.59208912688028,-4.41325452164384));
#64931=CARTESIAN_POINT('Ctrl Pts',(44.6786118485187,-3.78458679470619,-5.1225970772019));
#64932=CARTESIAN_POINT('Ctrl Pts',(44.712135151838,-2.85676105929807,-5.59623290931935));
#64933=CARTESIAN_POINT('Ctrl Pts',(44.7456584551572,-1.92893532388997,-6.06986874143678));
#64934=CARTESIAN_POINT('Ctrl Pts',(44.7791817584765,-0.88078618524785,-6.30779785011365));
#64935=CARTESIAN_POINT('Ctrl Pts',(44.8127050617957,0.160598724706423,-6.281171433331));
#64936=CARTESIAN_POINT('Ctrl Pts',(44.846228365115,1.2019836346607,-6.25454501654834));
#64937=CARTESIAN_POINT('Ctrl Pts',(44.8797516684343,2.23660431592705,-5.96336307430617));
#64938=CARTESIAN_POINT('Ctrl Pts',(44.9132749717535,3.13901345621759,-5.44293129177244));
#64939=CARTESIAN_POINT('Ctrl Pts',(44.9467982750728,4.04142259650808,-4.92249950923873));
#64940=CARTESIAN_POINT('Ctrl Pts',(44.9803215783921,4.81162019582283,-4.1728178864134));
#64941=CARTESIAN_POINT('Ctrl Pts',(45.0138448817113,5.35622012674883,-3.28478499739046));
#64942=CARTESIAN_POINT('Ctrl Pts',(45.0473681850306,5.90082005767485,-2.39675210836748));
#64943=CARTESIAN_POINT('Ctrl Pts',(45.0808914883498,6.21982232021221,-1.37036795314681));
#64944=CARTESIAN_POINT('Ctrl Pts',(45.1144147916691,6.27454802733141,-0.330081168778459));
#64945=CARTESIAN_POINT('Ctrl Pts',(45.1479380949884,6.32927373445062,0.710205615589953));
#64946=CARTESIAN_POINT('Ctrl Pts',(45.1814613983077,6.11972288615163,1.764395029106));
#64947=CARTESIAN_POINT('Ctrl Pts',(45.214984701627,5.671303432597,2.70466705911914));
#64948=CARTESIAN_POINT('Ctrl Pts',(45.2485080049462,5.22288397904237,3.64493908913229));
#64949=CARTESIAN_POINT('Ctrl Pts',(45.2820313082655,4.53559592023213,4.47129373564248));
#64950=CARTESIAN_POINT('Ctrl Pts',(45.3155546115847,3.69277263747835,5.08353585343527));
#64951=CARTESIAN_POINT('Ctrl Pts',(45.349077914904,2.84994935472466,5.695777971228));
#64952=CARTESIAN_POINT('Ctrl Pts',(45.3826012182233,1.85159084802752,6.09390756030336));
#64953=CARTESIAN_POINT('Ctrl Pts',(45.4161245215426,0.81874765661607,6.22965157934666));
#64954=CARTESIAN_POINT('Ctrl Pts',(45.4496478248618,-0.214095534795499,
6.36539559838998));
#64955=CARTESIAN_POINT('Ctrl Pts',(45.4831711281811,-1.28142341092133,6.23875404740119));
#64956=CARTESIAN_POINT('Ctrl Pts',(45.5166944315003,-2.25382292617444,5.86508215992932));
#64957=CARTESIAN_POINT('Ctrl Pts',(45.5502177348196,-3.22622244142749,5.49141027245747));
#64958=CARTESIAN_POINT('Ctrl Pts',(45.5837410381389,-4.10369359580792,4.87070804850249));
#64959=CARTESIAN_POINT('Ctrl Pts',(45.6172643414582,-4.77984338952302,4.07823536555993));
#64960=CARTESIAN_POINT('Ctrl Pts',(45.6507876447775,-5.45599318323813,3.28576268261738));
#64961=CARTESIAN_POINT('Ctrl Pts',(45.6843109480967,-5.93082161628803,2.32151954068721));
#64962=CARTESIAN_POINT('Ctrl Pts',(45.7178342514159,-6.14675594553841,1.30242000570432));
#64963=CARTESIAN_POINT('Ctrl Pts',(45.7319022190424,-6.23737222891632,0.87475751881359));
#64964=CARTESIAN_POINT('Ctrl Pts',(45.7459701866689,-6.28239623692835,0.437434604199986));
#64965=CARTESIAN_POINT('Ctrl Pts',(45.7600381542954,-6.28221291207239,7.44799067214229E-5));
#64966=CARTESIAN_POINT('Origin',(37.,0.,0.));
#64967=CARTESIAN_POINT('',(47.2162984310705,-6.28318057928199,-5.75008399550381E-5));
#64968=CARTESIAN_POINT('',(47.0300381542954,-6.28318961685052,5.11731766753689E-5));
#64969=CARTESIAN_POINT('',(37.,-6.28269,-7.69407619853508E-16));
#64970=CARTESIAN_POINT('Ctrl Pts',(47.2162984310705,-6.28318057928199,-5.75008399550381E-5));
#64971=CARTESIAN_POINT('Ctrl Pts',(47.1845813851863,-6.28270696309185,0.985558841135021));
#64972=CARTESIAN_POINT('Ctrl Pts',(47.1528643393022,-6.04681012366187,1.97139394049844));
#64973=CARTESIAN_POINT('Ctrl Pts',(47.1211472934181,-5.59978829242448,2.84978552345151));
#64974=CARTESIAN_POINT('Ctrl Pts',(47.0876239900988,-5.12730896715399,3.77820072252161));
#64975=CARTESIAN_POINT('Ctrl Pts',(47.0541006867795,-4.4189731699039,4.58658631969245));
#64976=CARTESIAN_POINT('Ctrl Pts',(47.0205773834603,-3.56066631121291,5.17692590924784));
#64977=CARTESIAN_POINT('Ctrl Pts',(46.987054080141,-2.70235945252192,5.76726549880322));
#64978=CARTESIAN_POINT('Ctrl Pts',(46.9535307768217,-1.69408153239001,6.13955908074314));
#64979=CARTESIAN_POINT('Ctrl Pts',(46.9200074735025,-0.658085814655917,
6.24866621849789));
#64980=CARTESIAN_POINT('Ctrl Pts',(46.8864841701832,0.377909903078239,6.35777335625264));
#64981=CARTESIAN_POINT('Ctrl Pts',(46.8529608668639,1.44162341841459,6.20369404982219));
#64982=CARTESIAN_POINT('Ctrl Pts',(46.8194375635447,2.40407992545615,5.80511034879328));
#64983=CARTESIAN_POINT('Ctrl Pts',(46.7859142602254,3.36653643249765,5.40652664776439));
#64984=CARTESIAN_POINT('Ctrl Pts',(46.7523909569062,4.22773593124438,4.76343855213707));
#64985=CARTESIAN_POINT('Ctrl Pts',(46.7188676535869,4.88325835314589,3.9538202167118));
#64986=CARTESIAN_POINT('Ctrl Pts',(46.6853443502676,5.53878077504741,3.14420188128653));
#64987=CARTESIAN_POINT('Ctrl Pts',(46.6518210469483,5.98862612010372,2.1680533060633));
#64988=CARTESIAN_POINT('Ctrl Pts',(46.6182977436291,6.17825083384663,1.14373208563958));
#64989=CARTESIAN_POINT('Ctrl Pts',(46.5847744403098,6.36787554758956,0.119410865215797));
#64990=CARTESIAN_POINT('Ctrl Pts',(46.5512511369906,6.29727963001906,-0.953083000408475));
#64991=CARTESIAN_POINT('Ctrl Pts',(46.5177278336713,5.97502280575507,-1.94371009164303));
#64992=CARTESIAN_POINT('Ctrl Pts',(46.484204530352,5.65276598149109,-2.93433718287752));
#64993=CARTESIAN_POINT('Ctrl Pts',(46.4506812270327,5.07884825053365,-3.8430974997223));
#64994=CARTESIAN_POINT('Ctrl Pts',(46.4171579237134,4.3228568907389,-4.55980424490342));
#64995=CARTESIAN_POINT('Ctrl Pts',(46.3836346203942,3.56686553094416,-5.27651099008454));
#64996=CARTESIAN_POINT('Ctrl Pts',(46.3501113170749,2.62880054231211,-5.801164163602));
#64997=CARTESIAN_POINT('Ctrl Pts',(46.3165880137557,1.62240190095777,-6.07014979398504));
#64998=CARTESIAN_POINT('Ctrl Pts',(46.2830647104364,0.616003259603381,-6.33913542436811));
#64999=CARTESIAN_POINT('Ctrl Pts',(46.2495414071171,-0.458729034473312,
-6.35245351161674));
#65000=CARTESIAN_POINT('Ctrl Pts',(46.2160181037979,-1.47148415319569,-6.10848924338433));
#65001=CARTESIAN_POINT('Ctrl Pts',(46.1824948004786,-2.484239271918,-5.86452497515194));
#65002=CARTESIAN_POINT('Ctrl Pts',(46.1489714971593,-3.43501721528601,-5.36327835143854));
#65003=CARTESIAN_POINT('Ctrl Pts',(46.1154481938401,-4.20853656689479,-4.66552530962565));
#65004=CARTESIAN_POINT('Ctrl Pts',(46.0819248905208,-4.98205591850362,-3.96777226781271));
#65005=CARTESIAN_POINT('Ctrl Pts',(46.0484015872015,-5.57831667835322,-3.07351280790027));
#65006=CARTESIAN_POINT('Ctrl Pts',(46.0148782838823,-5.92502248595098,-2.0911755045006));
#65007=CARTESIAN_POINT('Ctrl Pts',(45.992018332945,-6.16144542064411,-1.42130767119992));
#65008=CARTESIAN_POINT('Ctrl Pts',(45.9691583820077,-6.28182422789153,-0.710483261391549));
#65009=CARTESIAN_POINT('Ctrl Pts',(45.9462984310705,-6.28242372114921,0.000143169579051167));
#65010=CARTESIAN_POINT('Ctrl Pts',(45.7600381542954,-6.28221291207239,7.44799067214229E-5));
#65011=CARTESIAN_POINT('Ctrl Pts',(45.7794934899882,-6.28195938244337,-0.604773943310985));
#65012=CARTESIAN_POINT('Ctrl Pts',(45.798948825681,-6.19524418226229,-1.20969353221928));
#65013=CARTESIAN_POINT('Ctrl Pts',(45.8184041613738,-6.02308547606459,-1.78923108437408));
#65014=CARTESIAN_POINT('Ctrl Pts',(45.851927464693,-5.7264404518895,-2.7878267114341));
#65015=CARTESIAN_POINT('Ctrl Pts',(45.8854507680123,-5.17611017808843,-3.71106203751854));
#65016=CARTESIAN_POINT('Ctrl Pts',(45.9189740713315,-4.43882196348974,-4.44699517671334));
#65017=CARTESIAN_POINT('Ctrl Pts',(45.9524973746508,-3.7015337488911,-5.1829283159081));
#65018=CARTESIAN_POINT('Ctrl Pts',(45.9860206779701,-2.77728759349483,-5.73155926821328));
#65019=CARTESIAN_POINT('Ctrl Pts',(46.0195439812894,-1.77814794583397,-6.02636676680047));
#65020=CARTESIAN_POINT('Ctrl Pts',(46.0530672846086,-0.779008298173049,
-6.32117426538768));
#65021=CARTESIAN_POINT('Ctrl Pts',(46.0865905879279,0.295024841752511,-6.36215831025689));
#65022=CARTESIAN_POINT('Ctrl Pts',(46.1201138912471,1.31372541800596,-6.14434960360783));
#65023=CARTESIAN_POINT('Ctrl Pts',(46.1536371945664,2.33242599425934,-5.92654089695879));
#65024=CARTESIAN_POINT('Ctrl Pts',(46.1871604978857,3.29579400684066,-5.4499394387915));
#65025=CARTESIAN_POINT('Ctrl Pts',(46.220683801205,4.08702149887179,-4.77233295077266));
#65026=CARTESIAN_POINT('Ctrl Pts',(46.2542071045243,4.87824899090288,-4.09472646275386));
#65027=CARTESIAN_POINT('Ctrl Pts',(46.2877304078435,5.49733596238385,-3.21611494488349));
#65028=CARTESIAN_POINT('Ctrl Pts',(46.3212537111627,5.86921838448651,-2.24302966553638));
#65029=CARTESIAN_POINT('Ctrl Pts',(46.354777014482,6.24110080658921,-1.26994438618916));
#65030=CARTESIAN_POINT('Ctrl Pts',(46.3883003178013,6.36577867931357,-0.202385345365309));
#65031=CARTESIAN_POINT('Ctrl Pts',(46.4218236211206,6.22813486425494,0.830206382728294));
#65032=CARTESIAN_POINT('Ctrl Pts',(46.4553469244398,6.0904910491963,1.86279811082196));
#65033=CARTESIAN_POINT('Ctrl Pts',(46.4888702277591,5.69052554635458,2.86042252618523));
#65034=CARTESIAN_POINT('Ctrl Pts',(46.5223935310784,5.0767340007985,3.70211809784712));
#65035=CARTESIAN_POINT('Ctrl Pts',(46.5559168343976,4.46294245524248,4.54381366950891));
#65036=CARTESIAN_POINT('Ctrl Pts',(46.5894401377169,3.63532486697211,5.22958039746938));
#65037=CARTESIAN_POINT('Ctrl Pts',(46.6229634410362,2.69422951234673,5.67626936112713));
#65038=CARTESIAN_POINT('Ctrl Pts',(46.6564867443554,1.75313415772135,6.12295832478488));
#65039=CARTESIAN_POINT('Ctrl Pts',(46.6900100476747,0.698561036740914,6.33056952413993));
#65040=CARTESIAN_POINT('Ctrl Pts',(46.723533350994,-0.34162331357906,6.27393019062931));
#65041=CARTESIAN_POINT('Ctrl Pts',(46.7570566543132,-1.38180766389903,6.21729085711869));
#65042=CARTESIAN_POINT('Ctrl Pts',(46.7905799576325,-2.40760324355858,5.8964009907424));
#65043=CARTESIAN_POINT('Ctrl Pts',(46.8241032609518,-3.29463278004108,5.35016834968298));
#65044=CARTESIAN_POINT('Ctrl Pts',(46.857626564271,-4.18166231652358,4.80393570862355));
#65045=CARTESIAN_POINT('Ctrl Pts',(46.8911498675903,-4.92992580982906,4.03236029288097));
#65046=CARTESIAN_POINT('Ctrl Pts',(46.9246731709096,-5.44869663345755,3.12899528951692));
#65047=CARTESIAN_POINT('Ctrl Pts',(46.9581964742288,-5.96746745708607,2.22563028615281));
#65048=CARTESIAN_POINT('Ctrl Pts',(46.9917197775481,-6.25674561103759,1.1904756951672));
#65049=CARTESIAN_POINT('Ctrl Pts',(47.0252430808674,-6.28145624365494,0.149043565171735));
#65050=CARTESIAN_POINT('Ctrl Pts',(47.0268414386767,-6.28263442207732,0.0993891154884421));
#65051=CARTESIAN_POINT('Ctrl Pts',(47.0284397964861,-6.28321116240861,0.0497203951529533));
#65052=CARTESIAN_POINT('Ctrl Pts',(47.0300381542954,-6.28318961685052,5.11731766753689E-5));
#65053=CARTESIAN_POINT('Origin',(37.,0.,0.));
#65054=CARTESIAN_POINT('',(48.4862984310705,-6.28220485483637,-6.9117828764842E-5));
#65055=CARTESIAN_POINT('',(48.3000381542954,-6.28240712885383,-0.000140271569211771));
#65056=CARTESIAN_POINT('',(37.,-6.28269,-7.69407619853508E-16));
#65057=CARTESIAN_POINT('Ctrl Pts',(48.4862984310705,-6.28220485483637,-6.9117828764842E-5));
#65058=CARTESIAN_POINT('Ctrl Pts',(48.4670509950035,-6.28197246600328,0.598318092477962));
#65059=CARTESIAN_POINT('Ctrl Pts',(48.4478035589365,-6.19712683672702,1.19676983422775));
#65060=CARTESIAN_POINT('Ctrl Pts',(48.4285561228695,-6.02857778477818,1.77063727017338));
#65061=CARTESIAN_POINT('Ctrl Pts',(48.3950328195502,-5.73501551638082,2.77014349288841));
#65062=CARTESIAN_POINT('Ctrl Pts',(48.361509516231,-5.18753666879845,3.69507256413081));
#65063=CARTESIAN_POINT('Ctrl Pts',(48.3279862129117,-4.4525228166577,4.43327723211516));
#65064=CARTESIAN_POINT('Ctrl Pts',(48.2944629095924,-3.71750896451704,5.17148190009943));
#65065=CARTESIAN_POINT('Ctrl Pts',(48.2609396062731,-2.79496010781804,5.72296216482569));
#65066=CARTESIAN_POINT('Ctrl Pts',(48.2274163029539,-1.7967348983572,6.02085128156089));
#65067=CARTESIAN_POINT('Ctrl Pts',(48.1938929996346,-0.798509688896358,
6.3187403982961));
#65068=CARTESIAN_POINT('Ctrl Pts',(48.1603696963154,0.275391873326325,6.36303836704025));
#65069=CARTESIAN_POINT('Ctrl Pts',(48.1268463929961,1.29475968611398,6.14837407814961));
#65070=CARTESIAN_POINT('Ctrl Pts',(48.0933230896769,2.3141274989017,5.93370978925896));
#65071=CARTESIAN_POINT('Ctrl Pts',(48.0597997863575,3.27896156225439,5.46008324273347));
#65072=CARTESIAN_POINT('Ctrl Pts',(48.0262764830383,4.07227616126894,4.78492145348372));
#65073=CARTESIAN_POINT('Ctrl Pts',(47.992753179719,4.86559076028345,4.10975966423401));
#65074=CARTESIAN_POINT('Ctrl Pts',(47.9592298763998,5.48738589495984,3.23306263226006));
#65075=CARTESIAN_POINT('Ctrl Pts',(47.9257065730805,5.86226917284815,2.26112949534572));
#65076=CARTESIAN_POINT('Ctrl Pts',(47.8921832697613,6.23715245073648,1.28919635843133));
#65077=CARTESIAN_POINT('Ctrl Pts',(47.8586599664419,6.36512387183669,0.222027116576553));
#65078=CARTESIAN_POINT('Ctrl Pts',(47.8251366631227,6.23066695642113,-0.810984418968658));
#65079=CARTESIAN_POINT('Ctrl Pts',(47.7916133598034,6.09621004100557,-1.84399595451381));
#65080=CARTESIAN_POINT('Ctrl Pts',(47.7580900564842,5.69932478907427,-2.8428497837494));
#65081=CARTESIAN_POINT('Ctrl Pts',(47.7245667531649,5.08813336659879,-3.68643530980162));
#65082=CARTESIAN_POINT('Ctrl Pts',(47.6910434498457,4.4769419441233,-4.53002083585385));
#65083=CARTESIAN_POINT('Ctrl Pts',(47.6575201465264,3.65144435110363,-5.21833805872271));
#65084=CARTESIAN_POINT('Ctrl Pts',(47.6239968432071,2.7117318153874,-5.66792881139697));
#65085=CARTESIAN_POINT('Ctrl Pts',(47.5904735398878,1.77201927967118,-6.11751956407122));
#65086=CARTESIAN_POINT('Ctrl Pts',(47.5569502365686,0.718091801258396,-6.32838384655087));
#65087=CARTESIAN_POINT('Ctrl Pts',(47.5234269332493,-0.32226236671889,-6.27495445534426));
#65088=CARTESIAN_POINT('Ctrl Pts',(47.48990362993,-1.36261653469624,-6.22152506413766));
#65089=CARTESIAN_POINT('Ctrl Pts',(47.4563803266108,-2.38939739223809,-5.90380199924476));
#65090=CARTESIAN_POINT('Ctrl Pts',(47.4228570232915,-3.27810820230869,-5.36030904553129));
#65091=CARTESIAN_POINT('Ctrl Pts',(47.3893337199722,-4.16681901237924,-4.81681609181785));
#65092=CARTESIAN_POINT('Ctrl Pts',(47.355810416653,-4.91745977497856,-4.04755324928385));
#65093=CARTESIAN_POINT('Ctrl Pts',(47.3222871133337,-5.43901562072804,-3.14579330648479));
#65094=CARTESIAN_POINT('Ctrl Pts',(47.2887638100144,-5.96057146647754,-2.24403336368567));
#65095=CARTESIAN_POINT('Ctrl Pts',(47.2552405066951,-6.25304239537717,-1.20977632062147));
#65096=CARTESIAN_POINT('Ctrl Pts',(47.2217172033759,-6.28096643318152,-0.168425398604667));
#65097=CARTESIAN_POINT('Ctrl Pts',(47.2199109459407,-6.28247099854081,-0.11231673211768));
#65098=CARTESIAN_POINT('Ctrl Pts',(47.2181046885056,-6.28320755130102,-0.0561874712158831));
#65099=CARTESIAN_POINT('Ctrl Pts',(47.2162984310705,-6.28318057928199,-5.75008399550381E-5));
#65100=CARTESIAN_POINT('Ctrl Pts',(47.0300381542954,-6.28318961685052,5.11731766753689E-5));
#65101=CARTESIAN_POINT('Ctrl Pts',(47.0619630998053,-6.28275927468073,-0.992021562876977));
#65102=CARTESIAN_POINT('Ctrl Pts',(47.0938880453153,-6.04364615948199,-1.98429442568766));
#65103=CARTESIAN_POINT('Ctrl Pts',(47.1258129908252,-5.59096812202356,-2.86705109542662));
#65104=CARTESIAN_POINT('Ctrl Pts',(47.1593362941445,-5.11562625649168,-3.79400395702412));
#65105=CARTESIAN_POINT('Ctrl Pts',(47.1928595974637,-4.40479941414474,-4.60020001121386));
#65106=CARTESIAN_POINT('Ctrl Pts',(47.226382900783,-3.54467504366722,-5.18788833342367));
#65107=CARTESIAN_POINT('Ctrl Pts',(47.2599062041023,-2.68455067318971,-5.77557665563349));
#65108=CARTESIAN_POINT('Ctrl Pts',(47.2934295074215,-1.67512877458163,-6.14475724586337));
#65109=CARTESIAN_POINT('Ctrl Pts',(47.3269528107408,-0.638801318579545,
-6.25066711644859));
#65110=CARTESIAN_POINT('Ctrl Pts',(47.36047611406,0.397526137422538,-6.3565769870338));
#65111=CARTESIAN_POINT('Ctrl Pts',(47.3939994173793,1.46075915081862,-6.19921613797434));
#65112=CARTESIAN_POINT('Ctrl Pts',(47.4275227206986,2.42198117636517,-5.79766450448829));
#65113=CARTESIAN_POINT('Ctrl Pts',(47.4610460240179,3.38320320191172,-5.39611287100225));
#65114=CARTESIAN_POINT('Ctrl Pts',(47.4945693273371,4.24241423960874,-4.75037045308961));
#65115=CARTESIAN_POINT('Ctrl Pts',(47.5280926306564,4.89543532095221,-3.93873324098551));
#65116=CARTESIAN_POINT('Ctrl Pts',(47.5616159339756,5.54845640229572,-3.12709602888136));
#65117=CARTESIAN_POINT('Ctrl Pts',(47.5951392372949,5.99528752728566,-2.14956402258571));
#65118=CARTESIAN_POINT('Ctrl Pts',(47.6286625406142,6.18175061433953,-1.12466255711813));
#65119=CARTESIAN_POINT('Ctrl Pts',(47.6621858439335,6.36821370139339,-0.0997610916506096));
#65120=CARTESIAN_POINT('Ctrl Pts',(47.6957091472527,6.2943087505112,0.972509832988839));
#65121=CARTESIAN_POINT('Ctrl Pts',(47.729232450572,5.96899670517768,1.96213782870847));
#65122=CARTESIAN_POINT('Ctrl Pts',(47.7627557538913,5.64368465984415,2.95176582442809));
#65123=CARTESIAN_POINT('Ctrl Pts',(47.7962790572105,5.06696552005929,3.8587508912279));
#65124=CARTESIAN_POINT('Ctrl Pts',(47.8298023605298,4.30876623329383,4.57312148013779));
#65125=CARTESIAN_POINT('Ctrl Pts',(47.8633256638491,3.55056694652832,5.28749206904772));
#65126=CARTESIAN_POINT('Ctrl Pts',(47.8968489671683,2.61088751278218,5.80924818006771));
#65127=CARTESIAN_POINT('Ctrl Pts',(47.9303722704876,1.60366365894564,6.0751271093079));
#65128=CARTESIAN_POINT('Ctrl Pts',(47.9638955738069,0.59643980510915,6.34100603854808));
#65129=CARTESIAN_POINT('Ctrl Pts',(47.9974188771261,-0.478328468817734,
6.35100778600848));
#65130=CARTESIAN_POINT('Ctrl Pts',(48.0309421804454,-1.49032597221706,6.10391964411443));
#65131=CARTESIAN_POINT('Ctrl Pts',(48.0644654837646,-2.50232347561639,5.85683150222037));
#65132=CARTESIAN_POINT('Ctrl Pts',(48.0979887870839,-3.45155020848816,5.35265347097187));
#65133=CARTESIAN_POINT('Ctrl Pts',(48.1315120904032,-4.22291283803247,4.65251691965233));
#65134=CARTESIAN_POINT('Ctrl Pts',(48.1650353937225,-4.99427546757683,3.95238036833276));
#65135=CARTESIAN_POINT('Ctrl Pts',(48.1985586970417,-5.5877739937937,3.05628529694214));
#65136=CARTESIAN_POINT('Ctrl Pts',(48.232082000361,-5.93144697582958,2.07288284719442));
#65137=CARTESIAN_POINT('Ctrl Pts',(48.2547340516725,-6.16367045181887,1.40838739042628));
#65138=CARTESIAN_POINT('Ctrl Pts',(48.2773861029839,-6.2818273788379,0.704028710778029));
#65139=CARTESIAN_POINT('Ctrl Pts',(48.3000381542954,-6.28240712885383,-0.000140271569211771));
#65140=CARTESIAN_POINT('Origin',(37.,0.,0.));
#65141=CARTESIAN_POINT('',(49.7562984310704,-6.28278348713276,0.000156540911899483));
#65142=CARTESIAN_POINT('',(49.5700381542954,-6.28246359837908,0.000149097063601992));
#65143=CARTESIAN_POINT('',(37.,-6.28269,-7.69407619853508E-16));
#65144=CARTESIAN_POINT('Ctrl Pts',(49.7562984310704,-6.28278348713276,0.000156540911899483));
#65145=CARTESIAN_POINT('Ctrl Pts',(49.7495206048206,-6.28299901254035,0.210817954556831));
#65146=CARTESIAN_POINT('Ctrl Pts',(49.7427427785708,-6.27261027340816,0.421458208397696));
#65147=CARTESIAN_POINT('Ctrl Pts',(49.7359649523209,-6.25145825089702,0.63101203391033));
#65148=CARTESIAN_POINT('Ctrl Pts',(49.7024416490017,-6.14683980239764,1.66747065580799));
#65149=CARTESIAN_POINT('Ctrl Pts',(49.6689183456824,-5.77891731260458,2.67735179578619));
#65150=CARTESIAN_POINT('Ctrl Pts',(49.6353950423631,-5.19230122504616,3.53820780028988));
#65151=CARTESIAN_POINT('Ctrl Pts',(49.6018717390439,-4.60568513748774,4.39906380479358));
#65152=CARTESIAN_POINT('Ctrl Pts',(49.5683484357246,-3.80037545216395,5.11089467382279));
#65153=CARTESIAN_POINT('Ctrl Pts',(49.5348251324053,-2.87401562180346,5.58739122088992));
#65154=CARTESIAN_POINT('Ctrl Pts',(49.501301829086,-1.94765579144292,6.06388776795708));
#65155=CARTESIAN_POINT('Ctrl Pts',(49.4677785257668,-0.900245816045651,
6.30504999306214));
#65156=CARTESIAN_POINT('Ctrl Pts',(49.4342552224475,0.141216295691665,6.2816370802108));
#65157=CARTESIAN_POINT('Ctrl Pts',(49.4007319191283,1.18267840742892,6.25822416735945));
#65158=CARTESIAN_POINT('Ctrl Pts',(49.367208615809,2.21819265550626,5.97023611655172));
#65159=CARTESIAN_POINT('Ctrl Pts',(49.3336853124897,3.12220338304444,5.45259135499387));
#65160=CARTESIAN_POINT('Ctrl Pts',(49.3001620091704,4.02621411058273,4.93494659343596));
#65161=CARTESIAN_POINT('Ctrl Pts',(49.2666387058512,4.79872131758188,4.18764512112786));
#65162=CARTESIAN_POINT('Ctrl Pts',(49.2331154025319,5.34605883769137,3.30129691993769));
#65163=CARTESIAN_POINT('Ctrl Pts',(49.1995920992126,5.89339635780079,2.41494871874763));
#65164=CARTESIAN_POINT('Ctrl Pts',(49.1660687958934,6.21556419102064,1.38955378867549));
#65165=CARTESIAN_POINT('Ctrl Pts',(49.1325454925741,6.27349962623864,0.349440823647891));
#65166=CARTESIAN_POINT('Ctrl Pts',(49.0990221892548,6.33143506145664,-0.690672141379647));
#65167=CARTESIAN_POINT('Ctrl Pts',(49.0654988859356,6.12513809867287,-1.74550314136252));
#65168=CARTESIAN_POINT('Ctrl Pts',(49.0319755826163,5.67962215583164,-2.68715437156751));
#65169=CARTESIAN_POINT('Ctrl Pts',(48.9984522792971,5.23410621299034,-3.62880560177266));
#65170=CARTESIAN_POINT('Ctrl Pts',(48.9649289759778,4.54937129009149,-4.45727706219976));
#65171=CARTESIAN_POINT('Ctrl Pts',(48.9314056726585,3.70844120181689,-5.07211694485794));
#65172=CARTESIAN_POINT('Ctrl Pts',(48.8978823693393,2.86751111354239,-5.68695682751605));
#65173=CARTESIAN_POINT('Ctrl Pts',(48.86435906602,1.87038585989214,-6.08816513240533));
#65174=CARTESIAN_POINT('Ctrl Pts',(48.8308357627007,0.837966448694264,-6.22709552524375));
#65175=CARTESIAN_POINT('Ctrl Pts',(48.7973124593814,-0.194452962503611,
-6.36602591808218));
#65176=CARTESIAN_POINT('Ctrl Pts',(48.7637891560622,-1.26216653124915,-6.24267839886975));
#65177=CARTESIAN_POINT('Ctrl Pts',(48.7302658527429,-2.23571444689116,-5.87200880122044));
#65178=CARTESIAN_POINT('Ctrl Pts',(48.6967425494236,-3.20926236253323,-5.5013392035711));
#65179=CARTESIAN_POINT('Ctrl Pts',(48.6632192461044,-4.08864462507178,-4.88334752748483));
#65180=CARTESIAN_POINT('Ctrl Pts',(48.6296959427851,-4.76723651367273,-4.09296499769465));
#65181=CARTESIAN_POINT('Ctrl Pts',(48.5961726394658,-5.44582840227364,-3.30258246790451));
#65182=CARTESIAN_POINT('Ctrl Pts',(48.5626493361466,-5.92362991693698,-2.33980908441044));
#65183=CARTESIAN_POINT('Ctrl Pts',(48.5291260328273,-6.14270782966245,-1.32138070556966));
#65184=CARTESIAN_POINT('Ctrl Pts',(48.514850165575,-6.23600195316186,-0.887683936375279));
#65185=CARTESIAN_POINT('Ctrl Pts',(48.5005742983228,-6.28237721816416,-0.443894277194152));
#65186=CARTESIAN_POINT('Ctrl Pts',(48.4862984310705,-6.28220485483637,-6.9117828764842E-5));
#65187=CARTESIAN_POINT('Ctrl Pts',(48.3000381542954,-6.28240712885383,-0.000140271569211771));
#65188=CARTESIAN_POINT('Ctrl Pts',(48.3109094063032,-6.28268536451726,-0.338087522257749));
#65189=CARTESIAN_POINT('Ctrl Pts',(48.321780658311,-6.25588245148254,-0.675991080616301));
#65190=CARTESIAN_POINT('Ctrl Pts',(48.3326519103188,-6.2016103279476,-1.00942353131101));
#65191=CARTESIAN_POINT('Ctrl Pts',(48.3661752136381,-6.03425326017489,-2.03761763196401));
#65192=CARTESIAN_POINT('Ctrl Pts',(48.3996985169573,-5.60569168677457,-3.02329600516527));
#65193=CARTESIAN_POINT('Ctrl Pts',(48.4332218202766,-4.9678885140624,-3.84694557241424));
#65194=CARTESIAN_POINT('Ctrl Pts',(48.4667451235959,-4.33008534135019,-4.67059513966326));
#65195=CARTESIAN_POINT('Ctrl Pts',(48.5002684269152,-3.48304056932611,-5.33221590095997));
#65196=CARTESIAN_POINT('Ctrl Pts',(48.5337917302344,-2.52945801201786,-5.75158662376821));
#65197=CARTESIAN_POINT('Ctrl Pts',(48.5673150335537,-1.57587545470966,-6.17095734657642));
#65198=CARTESIAN_POINT('Ctrl Pts',(48.6008383368729,-0.515755112117303,
-6.34807803089618));
#65199=CARTESIAN_POINT('Ctrl Pts',(48.6343616401922,0.522363880510887,-6.261472869989));
#65200=CARTESIAN_POINT('Ctrl Pts',(48.6678849435115,1.56048287313908,-6.17486770908183));
#65201=CARTESIAN_POINT('Ctrl Pts',(48.7014082468308,2.5766005158031,-5.82453670294771));
#65202=CARTESIAN_POINT('Ctrl Pts',(48.73493155015,3.44751298168156,-5.25295733529293));
#65203=CARTESIAN_POINT('Ctrl Pts',(48.7684548534693,4.31842544756001,-4.68137796763816));
#65204=CARTESIAN_POINT('Ctrl Pts',(48.8019781567885,5.04413273665289,-3.88855023846271));
#65205=CARTESIAN_POINT('Ctrl Pts',(48.8355014601078,5.53664315251252,-2.9706041686847));
#65206=CARTESIAN_POINT('Ctrl Pts',(48.869024763427,6.02915356837218,-2.05265809890663));
#65207=CARTESIAN_POINT('Ctrl Pts',(48.9025480667464,6.28846711099855,-1.00959368852598));
#65208=CARTESIAN_POINT('Ctrl Pts',(48.9360713700656,6.28314212496046,0.032117951648468));
#65209=CARTESIAN_POINT('Ctrl Pts',(48.9695946733849,6.27781713892237,1.07382959182286));
#65210=CARTESIAN_POINT('Ctrl Pts',(49.0031179767041,6.00785362421983,2.11418846179105));
#65211=CARTESIAN_POINT('Ctrl Pts',(49.0366412800234,5.50598454081438,3.02705149635478));
#65212=CARTESIAN_POINT('Ctrl Pts',(49.0701645833427,5.0041154574089,3.93991453091856));
#65213=CARTESIAN_POINT('Ctrl Pts',(49.103687886662,4.27034080530048,4.72528173007786));
#65214=CARTESIAN_POINT('Ctrl Pts',(49.1372111899812,3.39363044523012,5.28792765896791));
#65215=CARTESIAN_POINT('Ctrl Pts',(49.1707344933005,2.51692008515981,5.85057358785794));
#65216=CARTESIAN_POINT('Ctrl Pts',(49.2042577966197,1.49727401712759,6.19049824647874));
#65217=CARTESIAN_POINT('Ctrl Pts',(49.237781099939,0.458323888012076,6.266485916281));
#65218=CARTESIAN_POINT('Ctrl Pts',(49.2713044032583,-0.58062624110344,6.34247358608326));
#65219=CARTESIAN_POINT('Ctrl Pts',(49.3048277065776,-1.63888043130225,6.15452426706698));
#65220=CARTESIAN_POINT('Ctrl Pts',(49.3383510098968,-2.58812581751054,5.72542673326679));
#65221=CARTESIAN_POINT('Ctrl Pts',(49.3718743132161,-3.53737120371888,5.29632919946658));
#65222=CARTESIAN_POINT('Ctrl Pts',(49.4053976165353,-4.37760778593669,4.62608345088244));
#65223=CARTESIAN_POINT('Ctrl Pts',(49.4389209198546,-5.00695724021992,3.79595649604682));
#65224=CARTESIAN_POINT('Ctrl Pts',(49.4724442231739,-5.6363066945031,2.96582954121125));
#65225=CARTESIAN_POINT('Ctrl Pts',(49.5059675264932,-6.05476902085173,1.97582138012422));
#65226=CARTESIAN_POINT('Ctrl Pts',(49.5394908298125,-6.21160584230822,0.945970076203819));
#65227=CARTESIAN_POINT('Ctrl Pts',(49.5496732713068,-6.25924380159368,0.633160787985427));
#65228=CARTESIAN_POINT('Ctrl Pts',(49.5598557128011,-6.28274437057092,0.31667559863472));
#65229=CARTESIAN_POINT('Ctrl Pts',(49.5700381542954,-6.28246359837908,0.000149097063601992));
#65230=CARTESIAN_POINT('Origin',(37.,0.,0.));
#65231=CARTESIAN_POINT('',(51.0262984310705,-6.28288820464993,-0.000145391911651194));
#65232=CARTESIAN_POINT('',(50.8400381542954,-6.28315629679635,-7.16818851180851E-5));
#65233=CARTESIAN_POINT('',(37.,-6.28269,-7.69407619853508E-16));
#65234=CARTESIAN_POINT('Ctrl Pts',(51.0262984310705,-6.28288820464993,-0.000145391911651194));
#65235=CARTESIAN_POINT('Ctrl Pts',(50.9984669113185,-6.28203197644536,0.864843652156353));
#65236=CARTESIAN_POINT('Ctrl Pts',(50.9706353915665,-6.10191477910553,1.73017821842932));
#65237=CARTESIAN_POINT('Ctrl Pts',(50.9428038718145,-5.75473404259442,2.5222891485024));
#65238=CARTESIAN_POINT('Ctrl Pts',(50.9092805684953,-5.33655187933529,3.47639353115891));
#65239=CARTESIAN_POINT('Ctrl Pts',(50.875757265176,-4.67598711202248,4.32426207259923));
#65240=CARTESIAN_POINT('Ctrl Pts',(50.8422339618567,-3.85313293437611,4.96309107710852));
#65241=CARTESIAN_POINT('Ctrl Pts',(50.8087106585375,-3.03027875672973,5.60192008161782));
#65242=CARTESIAN_POINT('Ctrl Pts',(50.7751873552182,-2.04513516874982,6.03170954919608));
#65243=CARTESIAN_POINT('Ctrl Pts',(50.7416640518989,-1.01715040645896,6.200347691887));
#65244=CARTESIAN_POINT('Ctrl Pts',(50.7081407485797,0.010834355831897,6.36898583457792));
#65245=CARTESIAN_POINT('Ctrl Pts',(50.6746174452604,1.08166029243366,6.2764726523815));
#65246=CARTESIAN_POINT('Ctrl Pts',(50.6410941419412,2.06549021943224,5.93402532882005));
#65247=CARTESIAN_POINT('Ctrl Pts',(50.6075708386219,3.04932014643076,5.59157800525862));
#65248=CARTESIAN_POINT('Ctrl Pts',(50.5740475353026,3.94615406382622,4.99919654033207));
#65249=CARTESIAN_POINT('Ctrl Pts',(50.5405242319833,4.64725124514435,4.22870693169346));
#65250=CARTESIAN_POINT('Ctrl Pts',(50.5070009286641,5.34834842646256,3.45821732305477));
#65251=CARTESIAN_POINT('Ctrl Pts',(50.4734776253448,5.85370887170347,2.50961957070406));
#65252=CARTESIAN_POINT('Ctrl Pts',(50.4399543220256,6.10205784439616,1.49793074382345));
#65253=CARTESIAN_POINT('Ctrl Pts',(50.4064310187063,6.35040681708886,0.486241916942795));
#65254=CARTESIAN_POINT('Ctrl Pts',(50.372907715387,6.3417443172332,-0.588537984467577));
#65255=CARTESIAN_POINT('Ctrl Pts',(50.3393844120677,6.07712066920823,-1.59609235996233));
#65256=CARTESIAN_POINT('Ctrl Pts',(50.3058611087484,5.81249702118332,-2.60364673545692));
#65257=CARTESIAN_POINT('Ctrl Pts',(50.2723378054292,5.29191222498908,-3.54397558503604));
#65258=CARTESIAN_POINT('Ctrl Pts',(50.23881450211,4.57848696309705,-4.303064440419));
#65259=CARTESIAN_POINT('Ctrl Pts',(50.2052911987907,3.86506170120498,-5.06215329580199));
#65260=CARTESIAN_POINT('Ctrl Pts',(50.1717678954714,2.95879597361505,-5.64000215698894));
#65261=CARTESIAN_POINT('Ctrl Pts',(50.1382445921521,1.96957410972775,-5.96654709827537));
#65262=CARTESIAN_POINT('Ctrl Pts',(50.1047212888328,0.980352245840442,-6.2930920395618));
#65263=CARTESIAN_POINT('Ctrl Pts',(50.0711979855136,-0.0918257543442044,
-6.36833306094771));
#65264=CARTESIAN_POINT('Ctrl Pts',(50.0376746821943,-1.11695876978463,-6.18314722097487));
#65265=CARTESIAN_POINT('Ctrl Pts',(50.0041513788751,-2.14209178522506,-5.99796138100203));
#65266=CARTESIAN_POINT('Ctrl Pts',(49.9706280755558,-3.12017981592124,-5.55234867967045));
#65267=CARTESIAN_POINT('Ctrl Pts',(49.9371047722365,-3.9326301091344,-4.90033946521847));
#65268=CARTESIAN_POINT('Ctrl Pts',(49.9035814689172,-4.7450804023476,-4.24833025076646));
#65269=CARTESIAN_POINT('Ctrl Pts',(49.870058165598,-5.39189295807774,-3.38992452319404));
#65270=CARTESIAN_POINT('Ctrl Pts',(49.8365348622787,-5.79464203233995,-2.42920360749922));
#65271=CARTESIAN_POINT('Ctrl Pts',(49.8097893852093,-6.11596228016352,-1.66272367632657));
#65272=CARTESIAN_POINT('Ctrl Pts',(49.7830439081399,-6.28193301831962,-0.831118826789475));
#65273=CARTESIAN_POINT('Ctrl Pts',(49.7562984310704,-6.28278348713276,0.000156540911899483));
#65274=CARTESIAN_POINT('Ctrl Pts',(49.5700381542954,-6.28246359837908,0.000149097063601992));
#65275=CARTESIAN_POINT('Ctrl Pts',(49.5933790161204,-6.28181999390192,-0.725413759468975));
#65276=CARTESIAN_POINT('Ctrl Pts',(49.6167198779453,-6.15621775461188,-1.45119369032999));
#65277=CARTESIAN_POINT('Ctrl Pts',(49.6400607397702,-5.90994537476529,-2.13341327280043));
#65278=CARTESIAN_POINT('Ctrl Pts',(49.6735840430895,-5.5562367692015,-3.11325087113057));
#65279=CARTESIAN_POINT('Ctrl Pts',(49.7071073464088,-4.95360824150956,-4.003231621037));
#65280=CARTESIAN_POINT('Ctrl Pts',(49.7406306497281,-4.17512824129216,-4.69544573965404));
#65281=CARTESIAN_POINT('Ctrl Pts',(49.7741539530473,-3.39664824107481,-5.38765985827105));
#65282=CARTESIAN_POINT('Ctrl Pts',(49.8076772563666,-2.44231676833202,-5.88210734559869));
#65283=CARTESIAN_POINT('Ctrl Pts',(49.8412005596858,-1.42784610337591,-6.11883665661577));
#65284=CARTESIAN_POINT('Ctrl Pts',(49.8747238630051,-0.413375438419792,
-6.35556596763286));
#65285=CARTESIAN_POINT('Ctrl Pts',(49.9082471663244,0.661234418749648,-6.3345771023394));
#65286=CARTESIAN_POINT('Ctrl Pts',(49.9417704696436,1.66568748547812,-6.05841495161831));
#65287=CARTESIAN_POINT('Ctrl Pts',(49.9752937729629,2.67014055220664,-5.7822528008972));
#65288=CARTESIAN_POINT('Ctrl Pts',(50.0088170762822,3.60443682849419,-5.25091736474844));
#65289=CARTESIAN_POINT('Ctrl Pts',(50.0423403796014,4.3552932929754,-4.52883283611067));
#65290=CARTESIAN_POINT('Ctrl Pts',(50.0758636829207,5.10614975745656,-3.80674830747294));
#65291=CARTESIAN_POINT('Ctrl Pts',(50.10938698624,5.67356641013141,-2.89391468634623));
#65292=CARTESIAN_POINT('Ctrl Pts',(50.1429102895593,5.98874422608738,-1.90101265639547));
#65293=CARTESIAN_POINT('Ctrl Pts',(50.1764335928785,6.30392204204335,-0.908110626444702));
#65294=CARTESIAN_POINT('Ctrl Pts',(50.2099568961978,6.36686102128044,0.164859812330119));
#65295=CARTESIAN_POINT('Ctrl Pts',(50.243480199517,6.169929839656,1.18780145604941));
#65296=CARTESIAN_POINT('Ctrl Pts',(50.2770035028363,5.97299865803155,2.21074309976876));
#65297=CARTESIAN_POINT('Ctrl Pts',(50.3105268061556,5.51619731554554,3.18365594843258));
#65298=CARTESIAN_POINT('Ctrl Pts',(50.3440501094749,4.85491277836054,3.98857473789601));
#65299=CARTESIAN_POINT('Ctrl Pts',(50.3775734127941,4.19362824117558,4.79349352735939));
#65300=CARTESIAN_POINT('Ctrl Pts',(50.4110967161134,3.32786050929167,5.43041825762241));
#65301=CARTESIAN_POINT('Ctrl Pts',(50.4446200194326,2.36258354756087,5.82212207928221));
#65302=CARTESIAN_POINT('Ctrl Pts',(50.4781433227519,1.39730658583008,6.21382590094201));
#65303=CARTESIAN_POINT('Ctrl Pts',(50.5116666260712,0.332520394252399,6.36030881399858));
#65304=CARTESIAN_POINT('Ctrl Pts',(50.5451899293904,-0.702670159742614,
6.24380982829218));
#65305=CARTESIAN_POINT('Ctrl Pts',(50.5787132327097,-1.73786071373769,6.12731084258576));
#65306=CARTESIAN_POINT('Ctrl Pts',(50.612236536029,-2.74345563015009,5.74782995811634));
#65307=CARTESIAN_POINT('Ctrl Pts',(50.6457598393482,-3.59752695818729,5.15137906879181));
#65308=CARTESIAN_POINT('Ctrl Pts',(50.6792831426675,-4.45159828622444,4.55492817946731));
#65309=CARTESIAN_POINT('Ctrl Pts',(50.7128064459868,-5.15414602588641,3.74150728528773));
#65310=CARTESIAN_POINT('Ctrl Pts',(50.7463297493061,-5.61998656612579,2.80974331956433));
#65311=CARTESIAN_POINT('Ctrl Pts',(50.7775658843025,-6.0540445664117,1.94155008869493));
#65312=CARTESIAN_POINT('Ctrl Pts',(50.8088020192989,-6.28259281421262,0.97061112216302));
#65313=CARTESIAN_POINT('Ctrl Pts',(50.8400381542954,-6.28315629679635,-7.16818851180851E-5));
#65314=CARTESIAN_POINT('Origin',(37.,0.,0.));
#65315=CARTESIAN_POINT('',(52.2962984310704,-6.28217298973102,3.97775880020546E-5));
#65316=CARTESIAN_POINT('',(52.1100381542954,-6.28218861558386,-5.63730895511787E-5));
#65317=CARTESIAN_POINT('',(37.,-6.28269,-7.69407619853508E-16));
#65318=CARTESIAN_POINT('Ctrl Pts',(52.2962984310704,-6.28217298973102,3.97775880020546E-5));
#65319=CARTESIAN_POINT('Ctrl Pts',(52.2809365211356,-6.28227906390278,0.477636057591627));
#65320=CARTESIAN_POINT('Ctrl Pts',(52.2655746112008,-6.22851193741266,0.955208832619816));
#65321=CARTESIAN_POINT('Ctrl Pts',(52.250212701266,-6.12061110101499,1.42022047576571));
#65322=CARTESIAN_POINT('Ctrl Pts',(52.2166893979467,-5.88514607861162,2.43498533419222));
#65323=CARTESIAN_POINT('Ctrl Pts',(52.1831660946274,-5.39188814239352,3.38993218283741));
#65324=CARTESIAN_POINT('Ctrl Pts',(52.1496427913082,-4.70064460482311,4.16927412732642));
#65325=CARTESIAN_POINT('Ctrl Pts',(52.1161194879889,-4.00940106725278,4.94861607181534));
#65326=CARTESIAN_POINT('Ctrl Pts',(52.0825961846696,-3.12017192833018,5.55235311214812));
#65327=CARTESIAN_POINT('Ctrl Pts',(52.0490728813504,-2.14077583841207,5.90728239204119));
#65328=CARTESIAN_POINT('Ctrl Pts',(52.0155495780311,-1.16137974849396,6.26221167193427));
#65329=CARTESIAN_POINT('Ctrl Pts',(51.9820262747118,-0.0918167075805276,
6.36833319138765));
#65330=CARTESIAN_POINT('Ctrl Pts',(51.9485029713926,0.938229225972791,6.21277976184401));
#65331=CARTESIAN_POINT('Ctrl Pts',(51.9149796680733,1.96827515952611,6.05722633230036));
#65332=CARTESIAN_POINT('Ctrl Pts',(51.881456364754,2.95880398571927,5.63999795375958));
#65333=CARTESIAN_POINT('Ctrl Pts',(51.8479330614348,3.78971451071403,5.01168338753872));
#65334=CARTESIAN_POINT('Ctrl Pts',(51.8144097581155,4.62062503570879,4.38336882131786));
#65335=CARTESIAN_POINT('Ctrl Pts',(51.7808864547962,5.29191725950531,3.54396806741685));
#65336=CARTESIAN_POINT('Ctrl Pts',(51.747363151477,5.72219728890199,2.59525810595611));
#65337=CARTESIAN_POINT('Ctrl Pts',(51.7138398481577,6.15247731829869,1.64654814449533));
#65338=CARTESIAN_POINT('Ctrl Pts',(51.6803165448384,6.34174515329552,0.588528975474791));
#65339=CARTESIAN_POINT('Ctrl Pts',(51.6467932415192,6.26705215036274,-0.450515032248377));
#65340=CARTESIAN_POINT('Ctrl Pts',(51.6132699381999,6.19235914742996,-1.48955903997155));
#65341=CARTESIAN_POINT('Ctrl Pts',(51.5797466348806,5.85370530656757,-2.50962788639735));
#65342=CARTESIAN_POINT('Ctrl Pts',(51.5462233315613,5.29215226021866,-3.3870386629489));
#65343=CARTESIAN_POINT('Ctrl Pts',(51.5127000282421,4.73059921386977,-4.2644494395004));
#65344=CARTESIAN_POINT('Ctrl Pts',(51.4791767249228,3.94614696203438,-4.99920214617766));
#65345=CARTESIAN_POINT('Ctrl Pts',(51.4456534216036,3.03391000260804,-5.50220833354418));
#65346=CARTESIAN_POINT('Ctrl Pts',(51.4121301182843,2.12167304318169,-6.00521452091069));
#65347=CARTESIAN_POINT('Ctrl Pts',(51.378606814965,1.08165137616439,-6.27647418896646));
#65348=CARTESIAN_POINT('Ctrl Pts',(51.3450835116457,0.0399471810417346,
-6.28309721971377));
#65349=CARTESIAN_POINT('Ctrl Pts',(51.3115602083265,-1.00175701408092,-6.28972025046108));
#65350=CARTESIAN_POINT('Ctrl Pts',(51.2780369050072,-2.04514373730893,-6.03170664389993));
#65351=CARTESIAN_POINT('Ctrl Pts',(51.244513601688,-2.96370279753951,-5.54034043877311));
#65352=CARTESIAN_POINT('Ctrl Pts',(51.2109902983687,-3.88226185777009,-5.04897423364628));
#65353=CARTESIAN_POINT('Ctrl Pts',(51.1774669950494,-4.67599325500323,-4.32425542995378));
#65354=CARTESIAN_POINT('Ctrl Pts',(51.1439436917301,-5.24865739895781,-3.45405587071395));
#65355=CARTESIAN_POINT('Ctrl Pts',(51.1104203884109,-5.82132154291242,-2.58385631147407));
#65356=CARTESIAN_POINT('Ctrl Pts',(51.0768970850916,-6.17291843358843,-1.56817599668685));
#65357=CARTESIAN_POINT('Ctrl Pts',(51.0433737817723,-6.26081709932372,-0.530165727356866));
#65358=CARTESIAN_POINT('Ctrl Pts',(51.037681998205,-6.27574105166978,-0.353926239935505));
#65359=CARTESIAN_POINT('Ctrl Pts',(51.0319902146377,-6.28306331063293,-0.177043041439763));
#65360=CARTESIAN_POINT('Ctrl Pts',(51.0262984310705,-6.28288820464993,-0.000145391911651194));
#65361=CARTESIAN_POINT('Ctrl Pts',(50.8400381542954,-6.28315629679635,-7.16818851180851E-5));
#65362=CARTESIAN_POINT('Ctrl Pts',(50.8423253226182,-6.28319755604677,-0.0711468952931936));
#65363=CARTESIAN_POINT('Ctrl Pts',(50.844612490941,-6.28201648803129,-0.142220735300779));
#65364=CARTESIAN_POINT('Ctrl Pts',(50.8468996592638,-6.27960426962443,-0.213252765949846));
#65365=CARTESIAN_POINT('Ctrl Pts',(50.8804229625831,-6.2442480920669,-1.25437784847344));
#65366=CARTESIAN_POINT('Ctrl Pts',(50.9139462659024,-5.94440239613498,-2.28652097625335));
#65367=CARTESIAN_POINT('Ctrl Pts',(50.9474695692217,-5.41642334340257,-3.18453523929544));
#65368=CARTESIAN_POINT('Ctrl Pts',(50.9809928725409,-4.88844429067018,-4.08254950233747));
#65369=CARTESIAN_POINT('Ctrl Pts',(51.0145161758602,-4.1323318811373,-4.84643490064171));
#65370=CARTESIAN_POINT('Ctrl Pts',(51.0480394791794,-3.23976441901818,-5.38357065845099));
#65371=CARTESIAN_POINT('Ctrl Pts',(51.0815627824987,-2.34719695689906,-5.92070641626027));
#65372=CARTESIAN_POINT('Ctrl Pts',(51.115086085818,-1.31817444219368,-6.2310925335746));
#65373=CARTESIAN_POINT('Ctrl Pts',(51.1486093891372,-0.277465411904037,
-6.27709482726425));
#65374=CARTESIAN_POINT('Ctrl Pts',(51.1821326924565,0.763243618385662,-6.3230971209539));
#65375=CARTESIAN_POINT('Ctrl Pts',(51.2156559957758,1.81563916425966,-6.10471559101883));
#65376=CARTESIAN_POINT('Ctrl Pts',(51.249179299095,2.75211871874681,-5.64842890396915));
#65377=CARTESIAN_POINT('Ctrl Pts',(51.2827026024143,3.68859827323391,-5.19214221691949));
#65378=CARTESIAN_POINT('Ctrl Pts',(51.3162259057336,4.50916183633422,-4.49795037275522));
#65379=CARTESIAN_POINT('Ctrl Pts',(51.3497492090529,5.11431642920412,-3.65002383379116));
#65380=CARTESIAN_POINT('Ctrl Pts',(51.3832725123721,5.71947102207406,-2.80209729482705));
#65381=CARTESIAN_POINT('Ctrl Pts',(51.4167958156914,6.10921664471359,-1.80043606106309));
#65382=CARTESIAN_POINT('Ctrl Pts',(51.4503191190106,6.23629680812975,-0.76649112596386));
#65383=CARTESIAN_POINT('Ctrl Pts',(51.4838424223299,6.36337697154592,0.26745380913537));
#65384=CARTESIAN_POINT('Ctrl Pts',(51.5173657256492,6.22779167573876,1.33368244556975));
#65385=CARTESIAN_POINT('Ctrl Pts',(51.5508890289685,5.84598057946701,2.30291502009198));
#65386=CARTESIAN_POINT('Ctrl Pts',(51.5844123322877,5.46416948319528,3.27214759461415));
#65387=CARTESIAN_POINT('Ctrl Pts',(51.617935635607,4.83613258645898,4.14438410722406));
#65388=CARTESIAN_POINT('Ctrl Pts',(51.6514589389262,4.03801909267131,4.81386625619082));
#65389=CARTESIAN_POINT('Ctrl Pts',(51.6849822422455,3.23990559888364,5.48334840515759));
#65390=CARTESIAN_POINT('Ctrl Pts',(51.7185055455648,2.27171550804457,5.95007619048123));
#65391=CARTESIAN_POINT('Ctrl Pts',(51.7520288488841,1.25084145194549,6.15745906907757));
#65392=CARTESIAN_POINT('Ctrl Pts',(51.7855521522033,0.229967395846398,6.36484194767391));
#65393=CARTESIAN_POINT('Ctrl Pts',(51.8190754555226,-0.843590625512924,
6.31287991954294));
#65394=CARTESIAN_POINT('Ctrl Pts',(51.8525987588419,-1.83966416411708,6.00787335823035));
#65395=CARTESIAN_POINT('Ctrl Pts',(51.8861220621611,-2.83573770272123,5.70286679691777));
#65396=CARTESIAN_POINT('Ctrl Pts',(51.9196453654804,-3.75432675857026,5.14481570242368));
#65397=CARTESIAN_POINT('Ctrl Pts',(51.9531686687997,-4.48405280401665,4.40138352976211));
#65398=CARTESIAN_POINT('Ctrl Pts',(51.9866919721189,-5.21377884946307,3.65795135710051));
#65399=CARTESIAN_POINT('Ctrl Pts',(52.0202152754382,-5.75464188450669,2.72913810627147));
#65400=CARTESIAN_POINT('Ctrl Pts',(52.0537385787575,-6.04106249894367,1.72756198416353));
#65401=CARTESIAN_POINT('Ctrl Pts',(52.0725051039368,-6.20140229665138,1.16687429370754));
#65402=CARTESIAN_POINT('Ctrl Pts',(52.0912716291161,-6.2820044067331,0.583384025414971));
#65403=CARTESIAN_POINT('Ctrl Pts',(52.1100381542954,-6.28218861558386,-5.63730895511787E-5));
#65404=CARTESIAN_POINT('Origin',(37.,0.,0.));
#65405=CARTESIAN_POINT('',(53.5662984310705,-6.28311963543023,8.84621771294822E-5));
#65406=CARTESIAN_POINT('',(53.3800381542954,-6.28283028954965,0.000152413998317728));
#65407=CARTESIAN_POINT('',(37.,-6.28269,-7.69407619853508E-16));
#65408=CARTESIAN_POINT('Ctrl Pts',(53.5662984310705,-6.28311963543023,8.84621771294822E-5));
#65409=CARTESIAN_POINT('Ctrl Pts',(53.5634061309528,-6.28318170133873,0.0899700538258294));
#65410=CARTESIAN_POINT('Ctrl Pts',(53.5605138308351,-6.28129275480609,0.179849034806085));
#65411=CARTESIAN_POINT('Ctrl Pts',(53.5576215307174,-6.27743568838293,0.269643476396016));
#65412=CARTESIAN_POINT('Ctrl Pts',(53.5240982273981,-6.23273022824222,1.31040901915495));
#65413=CARTESIAN_POINT('Ctrl Pts',(53.4905749240788,-5.92362659308418,2.33981749945716));
#65414=CARTESIAN_POINT('Ctrl Pts',(53.4570516207596,-5.38760345798027,3.23305357860289));
#65415=CARTESIAN_POINT('Ctrl Pts',(53.4235283174403,-4.85158032287627,4.12628965774877));
#65416=CARTESIAN_POINT('Ctrl Pts',(53.3900050141211,-4.08863768782632,4.88335333573811));
#65417=CARTESIAN_POINT('Ctrl Pts',(53.3564817108018,-3.19128202285747,5.41245096927237));
#65418=CARTESIAN_POINT('Ctrl Pts',(53.3229584074825,-2.29392635788873,5.94154860280657));
#65419=CARTESIAN_POINT('Ctrl Pts',(53.2894351041632,-1.26215766300112,6.24268019188573));
#65420=CARTESIAN_POINT('Ctrl Pts',(53.255911800844,-0.221077446364313,6.27933366002215));
#65421=CARTESIAN_POINT('Ctrl Pts',(53.2223884975247,0.820002770272492,6.31598712815857));
#65422=CARTESIAN_POINT('Ctrl Pts',(53.1888651942055,1.87039450865849,6.08816247535226));
#65423=CARTESIAN_POINT('Ctrl Pts',(53.1553418908862,2.80273822159734,5.62348334316875));
#65424=CARTESIAN_POINT('Ctrl Pts',(53.1218185875669,3.73508193453619,5.15880421098525));
#65425=CARTESIAN_POINT('Ctrl Pts',(53.0882952842476,4.54937762202789,4.45727059942454));
#65426=CARTESIAN_POINT('Ctrl Pts',(53.0547719809284,5.14689228297022,3.60394315669717));
#65427=CARTESIAN_POINT('Ctrl Pts',(53.0212486776091,5.74440694391255,2.75061571396979));
#65428=CARTESIAN_POINT('Ctrl Pts',(52.9877253742898,6.12514057830551,1.74549444007574));
#65429=CARTESIAN_POINT('Ctrl Pts',(52.9542020709706,6.24292939658562,0.710449856979257));
#65430=CARTESIAN_POINT('Ctrl Pts',(52.9206787676513,6.36071821486574,-0.324594726117287));
#65431=CARTESIAN_POINT('Ctrl Pts',(52.8871554643321,6.21556221703297,-1.38956261841627));
#65432=CARTESIAN_POINT('Ctrl Pts',(52.8536321610128,5.82506150548354,-2.35532692141684));
#65433=CARTESIAN_POINT('Ctrl Pts',(52.8201088576935,5.43456079393411,-3.3210912244174));
#65434=CARTESIAN_POINT('Ctrl Pts',(52.7865855543742,4.79871536866802,-4.18765193811955));
#65435=CARTESIAN_POINT('Ctrl Pts',(52.753062251055,3.99462121375218,-4.84993894893488));
#65436=CARTESIAN_POINT('Ctrl Pts',(52.7195389477357,3.19052705883639,-5.51222595975018));
#65437=CARTESIAN_POINT('Ctrl Pts',(52.6860156444164,2.21818417427087,-5.97023926767867));
#65438=CARTESIAN_POINT('Ctrl Pts',(52.6524923410972,1.19548871633445,-6.16844495628597));
#65439=CARTESIAN_POINT('Ctrl Pts',(52.6189690377779,0.172793258398022,-6.36665064489327));
#65440=CARTESIAN_POINT('Ctrl Pts',(52.5854457344586,-0.90025477290931,-6.30504871417938));
#65441=CARTESIAN_POINT('Ctrl Pts',(52.5519224311394,-1.89354876566498,-5.9911083717206));
#65442=CARTESIAN_POINT('Ctrl Pts',(52.5183991278201,-2.8868427584207,-5.6771680292618));
#65443=CARTESIAN_POINT('Ctrl Pts',(52.4848758245008,-3.80038271262475,-5.11088927505809));
#65444=CARTESIAN_POINT('Ctrl Pts',(52.4513525211815,-4.52340230202128,-4.36093316432646));
#65445=CARTESIAN_POINT('Ctrl Pts',(52.4178292178623,-5.24642189141773,-3.61097705359491));
#65446=CARTESIAN_POINT('Ctrl Pts',(52.384305914543,-5.77892111600671,-2.6773435863355));
#65447=CARTESIAN_POINT('Ctrl Pts',(52.3507826112238,-6.05633467400686,-1.67323541860197));
#65448=CARTESIAN_POINT('Ctrl Pts',(52.3326212178393,-6.20662465912666,-1.12925551122031));
#65449=CARTESIAN_POINT('Ctrl Pts',(52.3144598244549,-6.28204758509257,-0.564591440593399));
#65450=CARTESIAN_POINT('Ctrl Pts',(52.2962984310704,-6.28217298973102,3.97775880020546E-5));
#65451=CARTESIAN_POINT('Ctrl Pts',(52.1100381542954,-6.28218861558386,-5.63730895511787E-5));
#65452=CARTESIAN_POINT('Ctrl Pts',(52.1247949324354,-6.28233346547568,-0.45883605853235));
#65453=CARTESIAN_POINT('Ctrl Pts',(52.1395517105753,-6.23275408168553,-0.917584908340834));
#65454=CARTESIAN_POINT('Ctrl Pts',(52.1543084887153,-6.13311973819662,-1.36519185545982));
#65455=CARTESIAN_POINT('Ctrl Pts',(52.1878317920346,-5.90677816918225,-2.38203057958831));
#65456=CARTESIAN_POINT('Ctrl Pts',(52.2213550953538,-5.42211683732318,-3.34136903445849));
#65457=CARTESIAN_POINT('Ctrl Pts',(52.2548783986731,-4.73790072050221,-4.12688784533034));
#65458=CARTESIAN_POINT('Ctrl Pts',(52.2884017019923,-4.05368460368123,-4.91240665620218));
#65459=CARTESIAN_POINT('Ctrl Pts',(52.3219250053116,-3.16991370189837,-5.52410582307568));
#65460=CARTESIAN_POINT('Ctrl Pts',(52.3554483086309,-2.19374485660695,-5.88781708525163));
#65461=CARTESIAN_POINT('Ctrl Pts',(52.3889716119501,-1.21757601131547,-6.25152834742761));
#65462=CARTESIAN_POINT('Ctrl Pts',(52.4224949152694,-0.149009222515451,
-6.36725170490601));
#65463=CARTESIAN_POINT('Ctrl Pts',(52.4560182185886,0.882392246577315,-6.22095575040135));
#65464=CARTESIAN_POINT('Ctrl Pts',(52.4895415219079,1.91379371566996,-6.07465979589671));
#65465=CARTESIAN_POINT('Ctrl Pts',(52.5230648252272,2.90802986505533,-5.66634452940909));
#65466=CARTESIAN_POINT('Ctrl Pts',(52.5565881285465,3.74454998955454,-5.04551800125575));
#65467=CARTESIAN_POINT('Ctrl Pts',(52.5901114318657,4.58107011405381,-4.42469147310237));
#65468=CARTESIAN_POINT('Ctrl Pts',(52.623634735185,5.25987421366686,-3.59135368328327));
#65469=CARTESIAN_POINT('Ctrl Pts',(52.6571580385042,5.69865758348159,-2.64654648013265));
#65470=CARTESIAN_POINT('Ctrl Pts',(52.6906813418235,6.13744095329634,-1.70173927698197));
#65471=CARTESIAN_POINT('Ctrl Pts',(52.7242046451428,6.33620359331273,-0.645462660499612));
#65472=CARTESIAN_POINT('Ctrl Pts',(52.7577279484621,6.27084561898115,0.394210284200658));
#65473=CARTESIAN_POINT('Ctrl Pts',(52.7912512517814,6.20548764464956,1.43388322890093));
#65474=CARTESIAN_POINT('Ctrl Pts',(52.8247745551006,5.87600905597011,2.45695250181907));
#65475=CARTESIAN_POINT('Ctrl Pts',(52.8582978584199,5.32235899000359,3.3393713939609));
#65476=CARTESIAN_POINT('Ctrl Pts',(52.8918211617391,4.76870892403713,4.22179028610262));
#65477=CARTESIAN_POINT('Ctrl Pts',(52.9253444650584,3.99088738078357,4.96355879746799));
#65478=CARTESIAN_POINT('Ctrl Pts',(52.9588677683777,3.08320488758523,5.47473781531546));
#65479=CARTESIAN_POINT('Ctrl Pts',(52.9923910716969,2.17552239438675,5.98591683316301));
#65480=CARTESIAN_POINT('Ctrl Pts',(53.0259143750162,1.13797895124335,6.26650635749272));
#65481=CARTESIAN_POINT('Ctrl Pts',(53.0594376783355,0.0963762540466073,
6.28248502926124));
#65482=CARTESIAN_POINT('Ctrl Pts',(53.0929609816548,-0.94522644315002,6.29846370102975));
#65483=CARTESIAN_POINT('Ctrl Pts',(53.126484284974,-1.99088839439997,6.04983152023715));
#65484=CARTESIAN_POINT('Ctrl Pts',(53.1600075882933,-2.91382353815079,5.56673503176638));
#65485=CARTESIAN_POINT('Ctrl Pts',(53.1935308916126,-3.83675868190156,5.08363854329565));
#65486=CARTESIAN_POINT('Ctrl Pts',(53.2270541949318,-4.6369670181532,4.36607774714679));
#65487=CARTESIAN_POINT('Ctrl Pts',(53.2605774982511,-5.21742363061766,3.50105658104994));
#65488=CARTESIAN_POINT('Ctrl Pts',(53.2941008015703,-5.79788024308219,2.63603541495299));
#65489=CARTESIAN_POINT('Ctrl Pts',(53.3276241048896,-6.15858513175947,1.62355387890804));
#65490=CARTESIAN_POINT('Ctrl Pts',(53.3611474082089,-6.25580298403,0.586374923284767));
#65491=CARTESIAN_POINT('Ctrl Pts',(53.3674443235711,-6.27406408979303,0.391554381980045));
#65492=CARTESIAN_POINT('Ctrl Pts',(53.3737412389332,-6.28302865535999,0.195862448454363));
#65493=CARTESIAN_POINT('Ctrl Pts',(53.3800381542954,-6.28283028954965,0.000152413998317728));
#65494=CARTESIAN_POINT('Origin',(37.,0.,0.));
#65495=CARTESIAN_POINT('',(54.8362984310704,-6.28252994889952,-0.000148679754663761));
#65496=CARTESIAN_POINT('',(54.6500381542954,-6.28284206479216,-0.000151303447314885));
#65497=CARTESIAN_POINT('',(37.,-6.28269,-7.69407619853508E-16));
#65498=CARTESIAN_POINT('Ctrl Pts',(54.8362984310704,-6.28252994889952,-0.000148679754663761));
#65499=CARTESIAN_POINT('Ctrl Pts',(54.8123524374506,-6.28183164615208,0.744205706882085));
#65500=CARTESIAN_POINT('Ctrl Pts',(54.7884064438308,-6.1494773107617,1.48879635703162));
#65501=CARTESIAN_POINT('Ctrl Pts',(54.764460450211,-5.8905402896867,2.18640382765216));
#65502=CARTESIAN_POINT('Ctrl Pts',(54.7309371468918,-5.52804022241435,3.16302259765179));
#65503=CARTESIAN_POINT('Ctrl Pts',(54.6974138435725,-4.91745419101602,4.04756031147763));
#65504=CARTESIAN_POINT('Ctrl Pts',(54.6638905402532,-4.13279136549942,4.73275600063913));
#65505=CARTESIAN_POINT('Ctrl Pts',(54.6303672369339,-3.34812853998279,5.41795168980066));
#65506=CARTESIAN_POINT('Ctrl Pts',(54.5968439336147,-2.38938892034787,5.90380535429783));
#65507=CARTESIAN_POINT('Ctrl Pts',(54.5633206302954,-1.37283159840298,6.13141314347905));
#65508=CARTESIAN_POINT('Ctrl Pts',(54.5297973269761,-0.356274276458217,
6.35902093266023));
#65509=CARTESIAN_POINT('Ctrl Pts',(54.4962740236568,0.718100747796503,6.32838284652552));
#65510=CARTESIAN_POINT('Ctrl Pts',(54.4627507203376,1.72003226351471,6.04321082867509));
#65511=CARTESIAN_POINT('Ctrl Pts',(54.4292274170183,2.72196377923304,5.75803881082463));
#65512=CARTESIAN_POINT('Ctrl Pts',(54.3957041136991,3.65145178641483,5.21833286125838));
#65513=CARTESIAN_POINT('Ctrl Pts',(54.3621808103798,4.39579304566329,4.48953358170574));
#65514=CARTESIAN_POINT('Ctrl Pts',(54.3286575070606,5.14013430491179,3.76073430215307));
#65515=CARTESIAN_POINT('Ctrl Pts',(54.2951342037413,5.69932881622692,2.842841692614));
#65516=CARTESIAN_POINT('Ctrl Pts',(54.261610900422,6.00557613055491,1.84714907670987));
#65517=CARTESIAN_POINT('Ctrl Pts',(54.2280875971027,6.31182344488285,0.851456460805907));
#65518=CARTESIAN_POINT('Ctrl Pts',(54.1945642937835,6.36512356222373,-0.222036161463082));
#65519=CARTESIAN_POINT('Ctrl Pts',(54.1610409904642,6.15901302578961,-1.2431678832118));
#65520=CARTESIAN_POINT('Ctrl Pts',(54.1275176871449,5.95290248935549,-2.26429960496059));
#65521=CARTESIAN_POINT('Ctrl Pts',(54.0939943838257,5.48738129914634,-3.23307042618909));
#65522=CARTESIAN_POINT('Ctrl Pts',(54.0604710805064,4.8188941286198,-4.0320175003176));
#65523=CARTESIAN_POINT('Ctrl Pts',(54.0269477771871,4.15040695809322,-4.83096457444614));
#65524=CARTESIAN_POINT('Ctrl Pts',(53.9934244738678,3.27895380724923,-5.46008790147467));
#65525=CARTESIAN_POINT('Ctrl Pts',(53.9599011705486,2.31019777605328,-5.84310644733658));
#65526=CARTESIAN_POINT('Ctrl Pts',(53.9263778672293,1.34144174485745,-6.22612499319844));
#65527=CARTESIAN_POINT('Ctrl Pts',(53.8928545639101,0.27538283330969,-6.36303875789375));
#65528=CARTESIAN_POINT('Ctrl Pts',(53.8593312605908,-0.758719662249247,
-6.23724705822467));
#65529=CARTESIAN_POINT('Ctrl Pts',(53.8258079572716,-1.7928221578083,-6.11145535855559));
#65530=CARTESIAN_POINT('Ctrl Pts',(53.7922846539523,-2.79496823737853,-5.72295819452207));
#65531=CARTESIAN_POINT('Ctrl Pts',(53.758761350633,-3.64364817746724,-5.11886065355629));
#65532=CARTESIAN_POINT('Ctrl Pts',(53.7252380473137,-4.49232811755596,-4.51476311259051));
#65533=CARTESIAN_POINT('Ctrl Pts',(53.6917147439944,-5.18754191816317,-3.69506519469248));
#65534=CARTESIAN_POINT('Ctrl Pts',(53.6581914406752,-5.64499517590509,-2.75915493313556));
#65535=CARTESIAN_POINT('Ctrl Pts',(53.6275604374736,-6.06298060141694,-1.90399248255254));
#65536=CARTESIAN_POINT('Ctrl Pts',(53.5969294342721,-6.28246232430602,-0.951805604666501));
#65537=CARTESIAN_POINT('Ctrl Pts',(53.5662984310705,-6.28311963543023,8.84621771294822E-5));
#65538=CARTESIAN_POINT('Ctrl Pts',(53.3800381542954,-6.28283028954965,0.000152413998317728));
#65539=CARTESIAN_POINT('Ctrl Pts',(53.4072645422525,-6.28197260222196,-0.846051960481647));
#65540=CARTESIAN_POINT('Ctrl Pts',(53.4344909302096,-6.1098143561761,-1.69259473097886));
#65541=CARTESIAN_POINT('Ctrl Pts',(53.4617173181667,-5.77715549886801,-2.47050214869888));
#65542=CARTESIAN_POINT('Ctrl Pts',(53.4952406214859,-5.36755934557172,-3.42832388985779));
#65543=CARTESIAN_POINT('Ctrl Pts',(53.5287639248052,-4.71463622311535,-4.28209099697412));
#65544=CARTESIAN_POINT('Ctrl Pts',(53.5622872281245,-3.89755277860976,-4.9282845761252));
#65545=CARTESIAN_POINT('Ctrl Pts',(53.5958105314438,-3.08046933410412,-5.57447815527632));
#65546=CARTESIAN_POINT('Ctrl Pts',(53.629333834763,-2.09922556754923,-6.01309820646219));
#65547=CARTESIAN_POINT('Ctrl Pts',(53.6628571380823,-1.07279686419783,-6.19096223659628));
#65548=CARTESIAN_POINT('Ctrl Pts',(53.6963804414015,-0.0463681608464844,
-6.36882626673037));
#65549=CARTESIAN_POINT('Ctrl Pts',(53.7299037447208,1.0252454793014,-6.2859342758127));
#65550=CARTESIAN_POINT('Ctrl Pts',(53.7634270480401,2.01211136537584,-5.9523368833727));
#65551=CARTESIAN_POINT('Ctrl Pts',(53.7969503513594,2.99897725145034,-5.61873949093267));
#65552=CARTESIAN_POINT('Ctrl Pts',(53.8304736546786,3.90109538345142,-5.03443669697027));
#65553=CARTESIAN_POINT('Ctrl Pts',(53.8639969579979,4.60908432271368,-4.27027496120012));
#65554=CARTESIAN_POINT('Ctrl Pts',(53.8975202613172,5.31707326197589,-3.50611322543002));
#65555=CARTESIAN_POINT('Ctrl Pts',(53.9310435646364,5.83093300849932,-2.56209254785216));
#65556=CARTESIAN_POINT('Ctrl Pts',(53.9645668679557,6.08835829593271,-1.55267503431523));
#65557=CARTESIAN_POINT('Ctrl Pts',(53.998090171275,6.3457835833661,-0.543257520778245));
#65558=CARTESIAN_POINT('Ctrl Pts',(54.0316134745942,6.34677441170943,0.531556828717691));
#65559=CARTESIAN_POINT('Ctrl Pts',(54.0651367779135,6.0912106302571,1.54144724672204));
#65560=CARTESIAN_POINT('Ctrl Pts',(54.0986600812328,5.8356468488048,2.55133766472626));
#65561=CARTESIAN_POINT('Ctrl Pts',(54.1321833845521,5.32352845755678,3.49630415123893));
#65562=CARTESIAN_POINT('Ctrl Pts',(54.1657066878713,4.61694961685463,4.26176990729727));
#65563=CARTESIAN_POINT('Ctrl Pts',(54.1992299911906,3.9103707761524,5.0272356633557));
#65564=CARTESIAN_POINT('Ctrl Pts',(54.2327532945098,3.00933148599608,5.61320068895984));
#65565=CARTESIAN_POINT('Ctrl Pts',(54.2662765978291,2.02308232195134,5.94861701454061));
#65566=CARTESIAN_POINT('Ctrl Pts',(54.2997999011483,1.0368331579066,6.28403334012138));
#65567=CARTESIAN_POINT('Ctrl Pts',(54.3333232044676,-0.0346258800264526,
6.36890096567867));
#65568=CARTESIAN_POINT('Ctrl Pts',(54.3668465077869,-1.06138074574406,6.19292965459644));
#65569=CARTESIAN_POINT('Ctrl Pts',(54.4003698111062,-2.0881356114616,6.01695834351422));
#65570=CARTESIAN_POINT('Ctrl Pts',(54.4338931144254,-3.07018630496374,5.5801480957925));
#65571=CARTESIAN_POINT('Ctrl Pts',(54.4674164177447,-3.88845979596622,4.93546210989902));
#65572=CARTESIAN_POINT('Ctrl Pts',(54.500939721064,-4.70673328696874,4.2907761240055));
#65573=CARTESIAN_POINT('Ctrl Pts',(54.5344630243832,-5.36122957547162,3.43821439994017));
#65574=CARTESIAN_POINT('Ctrl Pts',(54.5679863277025,-5.77259088926278,2.48114939807468));
#65575=CARTESIAN_POINT('Ctrl Pts',(54.5953369365668,-6.10820764779796,1.70031016291839));
#65576=CARTESIAN_POINT('Ctrl Pts',(54.6226875454311,-6.28198367935227,0.84990921015598));
#65577=CARTESIAN_POINT('Ctrl Pts',(54.6500381542954,-6.28284206479216,-0.000151303447314885));
#65578=CARTESIAN_POINT('Origin',(16.5082437683087,0.,0.));
#65579=CARTESIAN_POINT('',(55.2432437683087,-5.57769790490533,-0.000131999491044005));
#65580=CARTESIAN_POINT('',(55.26731,-5.57784,5.11151866531329E-13));
#65581=CARTESIAN_POINT('',(16.5082437683087,-5.57784,5.11151866531329E-13));
#65582=CARTESIAN_POINT('',(55.26731,-5.53834961081692,-0.66255766085986));
#65583=CARTESIAN_POINT('Ctrl Pts',(55.2432437683087,-5.57769790490533,-0.000131999491043942));
#65584=CARTESIAN_POINT('Ctrl Pts',(55.2512658455391,-5.57790559613044,-0.221520036468065));
#65585=CARTESIAN_POINT('Ctrl Pts',(55.2592879227696,-5.56499524171959,-0.442884532438414));
#65586=CARTESIAN_POINT('Ctrl Pts',(55.26731,-5.53879749490423,-0.662649316846852));
#65587=CARTESIAN_POINT('Origin',(55.26731,0.,0.));
#65588=CARTESIAN_POINT('Origin',(16.5082437683087,0.,0.));
#65589=CARTESIAN_POINT('',(53.9732437683087,-5.57822143497263,7.85376758110207E-5));
#65590=CARTESIAN_POINT('',(54.2430928170571,-5.57797500476393,-0.000134328833226449));
#65591=CARTESIAN_POINT('',(16.5082437683087,-5.57784,5.11151866531329E-13));
#65592=CARTESIAN_POINT('Ctrl Pts',(53.9732437683087,-5.57822143497263,7.85376758111623E-5));
#65593=CARTESIAN_POINT('Ctrl Pts',(54.0038747715103,-5.57763786706127,-0.845023290013137));
#65594=CARTESIAN_POINT('Ctrl Pts',(54.0680290780311,-5.16952209782556,-2.61556926080919));
#65595=CARTESIAN_POINT('Ctrl Pts',(54.1657066878714,-3.37111907823718,-4.73599208528508));
#65596=CARTESIAN_POINT('Ctrl Pts',(54.2662765978291,-0.701970757150338,
-5.77072801277767));
#65597=CARTESIAN_POINT('Ctrl Pts',(54.3668465077869,2.13740507033186,-5.40606745817384));
#65598=CARTESIAN_POINT('Ctrl Pts',(54.4674164177447,4.45846161278591,-3.73044001590026));
#65599=CARTESIAN_POINT('Ctrl Pts',(54.5679863277025,5.69834582588392,-1.15018443868033));
#65600=CARTESIAN_POINT('Ctrl Pts',(54.6685562376603,5.55638456732653,1.70899057466459));
#65601=CARTESIAN_POINT('Ctrl Pts',(54.7691261476182,4.06700779734722,4.15373547526812));
#65602=CARTESIAN_POINT('Ctrl Pts',(54.8696960575759,1.59137933916517,5.59120577878235));
#65603=CARTESIAN_POINT('Ctrl Pts',(54.9702659675337,-1.27014589220361,5.67280824955481));
#65604=CARTESIAN_POINT('Ctrl Pts',(55.0708358774915,-3.82368404225601,4.37876986600632));
#65605=CARTESIAN_POINT('Ctrl Pts',(55.1618284777499,-5.29506982353384,2.24721731124727));
#65606=CARTESIAN_POINT('Ctrl Pts',(55.2192977746889,-5.57707794418837,0.660713859839581));
#65607=CARTESIAN_POINT('Ctrl Pts',(55.2432437683087,-5.57769790490533,-0.000131999491043942));
#65608=CARTESIAN_POINT('',(55.26731,-1.93782473268743,5.23040479991605));
#65609=CARTESIAN_POINT('Origin',(55.26731,0.,0.));
#65610=CARTESIAN_POINT('Ctrl Pts',(54.2430928170571,-5.57797500476393,-0.000134328833225669));
#65611=CARTESIAN_POINT('Ctrl Pts',(54.249265511512,-5.57814699767408,-0.170459190757225));
#65612=CARTESIAN_POINT('Ctrl Pts',(54.2889615092863,-5.52896704997114,-1.26570281170263));
#65613=CARTESIAN_POINT('Ctrl Pts',(54.3621808103798,-4.83314809906796,-3.23028641703264));
#65614=CARTESIAN_POINT('Ctrl Pts',(54.4627507203376,-2.70537098973005,-5.14538998627536));
#65615=CARTESIAN_POINT('Ctrl Pts',(54.5633206302954,0.078446240209487,-5.81273346716538));
#65616=CARTESIAN_POINT('Ctrl Pts',(54.6638905402532,2.84325992667244,-5.0705086592284));
#65617=CARTESIAN_POINT('Ctrl Pts',(54.764460450211,4.91854716216131,-3.09866134240672));
#65618=CARTESIAN_POINT('Ctrl Pts',(54.8650303601689,5.8011660495001,-0.375447161461482));
#65619=CARTESIAN_POINT('Ctrl Pts',(54.9656002701266,5.27686000591952,2.43892212337069));
#65620=CARTESIAN_POINT('Ctrl Pts',(55.0661701800844,3.47320975124282,4.66163850225691));
#65621=CARTESIAN_POINT('Ctrl Pts',(55.1667400900422,0.826722671906332,5.75435770195244));
#65622=CARTESIAN_POINT('Ctrl Pts',(55.2337866966808,-1.07034715964058,5.55179856586871));
#65623=CARTESIAN_POINT('Ctrl Pts',(55.26731,-1.93782473268743,5.23040479991605));
#65624=CARTESIAN_POINT('Origin',(16.5082437683087,0.,0.));
#65625=CARTESIAN_POINT('',(52.7032437683088,-5.57738099270237,3.53149720619964E-5));
#65626=CARTESIAN_POINT('',(52.9730928170571,-5.57796455057653,0.000135314793302463));
#65627=CARTESIAN_POINT('',(16.5082437683087,-5.57784,5.11151866531329E-13));
#65628=CARTESIAN_POINT('Ctrl Pts',(52.7032437683088,-5.57738099270237,3.53149720621823E-5));
#65629=CARTESIAN_POINT('Ctrl Pts',(52.7214051616932,-5.57726965711069,-0.501250375396387));
#65630=CARTESIAN_POINT('Ctrl Pts',(52.7730898583969,-5.38670752464807,-1.92791989326071));
#65631=CARTESIAN_POINT('Ctrl Pts',(52.8582978584198,-4.18507142767569,-4.03475427685318));
#65632=CARTESIAN_POINT('Ctrl Pts',(52.9588677683777,-1.75191953024455,-5.54299944875284));
#65633=CARTESIAN_POINT('Ctrl Pts',(53.0594376783355,1.10607134513556,-5.70707202588776));
#65634=CARTESIAN_POINT('Ctrl Pts',(53.1600075882933,3.69584087152237,-4.48718454958579));
#65635=CARTESIAN_POINT('Ctrl Pts',(53.2605774982511,5.38937216792545,-2.1791586826484));
#65636=CARTESIAN_POINT('Ctrl Pts',(53.3611474082089,5.77598535317805,0.657311288835543));
#65637=CARTESIAN_POINT('Ctrl Pts',(53.4617173181667,4.76192706193859,3.33438383883116));
#65638=CARTESIAN_POINT('Ctrl Pts',(53.5622872281245,2.59310555832215,5.2028711778091));
#65639=CARTESIAN_POINT('Ctrl Pts',(53.6628571380823,-0.204541812806597,
5.80966673579904));
#65640=CARTESIAN_POINT('Ctrl Pts',(53.7634270480401,-2.95258796680689,5.00762310982228));
#65641=CARTESIAN_POINT('Ctrl Pts',(53.8639969579978,-4.98463408757047,2.99123519367383));
#65642=CARTESIAN_POINT('Ctrl Pts',(53.9339358647541,-5.55716187048982,1.08454472513754));
#65643=CARTESIAN_POINT('Ctrl Pts',(53.9703514681911,-5.57827653775616,0.0798763849612549));
#65644=CARTESIAN_POINT('Ctrl Pts',(53.9732437683087,-5.57822143497263,7.85376758111623E-5));
#65645=CARTESIAN_POINT('Ctrl Pts',(52.9730928170571,-5.57796455057653,0.000135314793302289));
#65646=CARTESIAN_POINT('Ctrl Pts',(53.0003192050142,-5.57720308650882,-0.751134063156271));
#65647=CARTESIAN_POINT('Ctrl Pts',(53.0610688962905,-5.23616546002432,-2.42809664728444));
#65648=CARTESIAN_POINT('Ctrl Pts',(53.1553418908863,-3.60603273460568,-4.55967026342535));
#65649=CARTESIAN_POINT('Ctrl Pts',(53.2559118008439,-0.99255631088897,-5.72790511170206));
#65650=CARTESIAN_POINT('Ctrl Pts',(53.3564817108019,1.86161416062682,-5.50712789877888));
#65651=CARTESIAN_POINT('Ctrl Pts',(53.4570516207595,4.26434480692677,-3.95087691570875));
#65652=CARTESIAN_POINT('Ctrl Pts',(53.5576215307175,5.63297549627246,-1.43654167257841));
#65653=CARTESIAN_POINT('Ctrl Pts',(53.6581914406752,5.63561450056838,1.42615367186469));
#65654=CARTESIAN_POINT('Ctrl Pts',(53.758761350633,4.2716217932542,3.94300801314016));
#65655=CARTESIAN_POINT('Ctrl Pts',(53.8593312605908,1.87176456925964,5.50368623779372));
#65656=CARTESIAN_POINT('Ctrl Pts',(53.9599011705486,-0.981994129710483,
5.72972541999358));
#65657=CARTESIAN_POINT('Ctrl Pts',(54.0604710805064,-3.59761974878958,4.56631086087063));
#65658=CARTESIAN_POINT('Ctrl Pts',(54.1548682960093,-5.23383330465535,2.43494193696294));
#65659=CARTESIAN_POINT('Ctrl Pts',(54.2157422081928,-5.57721292090455,0.754558571054565));
#65660=CARTESIAN_POINT('Ctrl Pts',(54.2430928170571,-5.57797500476393,-0.000134328833225669));
#65661=CARTESIAN_POINT('Origin',(16.5082437683087,0.,0.));
#65662=CARTESIAN_POINT('',(51.4332437683088,-5.57801596822771,-0.00012908050836989));
#65663=CARTESIAN_POINT('',(51.7030928170571,-5.57739486550319,-5.00486370436093E-5));
#65664=CARTESIAN_POINT('',(16.5082437683087,-5.57784,5.11151866531329E-13));
#65665=CARTESIAN_POINT('Ctrl Pts',(51.4332437683088,-5.57801596822771,-0.000129080508369864));
#65666=CARTESIAN_POINT('Ctrl Pts',(51.4389355518761,-5.57817142920959,-0.157180723267159));
#65667=CARTESIAN_POINT('Ctrl Pts',(51.4781506387626,-5.53338253817611,-1.23914222489699));
#65668=CARTESIAN_POINT('Ctrl Pts',(51.5508890289684,-4.85608058876542,-3.19570747170793));
#65669=CARTESIAN_POINT('Ctrl Pts',(51.6514589389262,-2.74203068176238,-5.12594700222191));
#65670=CARTESIAN_POINT('Ctrl Pts',(51.7520288488841,0.036959305149328,-5.81314879725927));
#65671=CARTESIAN_POINT('Ctrl Pts',(51.8525987588419,2.80698669237795,-5.09066701308651));
#65672=CARTESIAN_POINT('Ctrl Pts',(51.9531686687997,4.89632222303964,-3.13370286043244));
#65673=CARTESIAN_POINT('Ctrl Pts',(52.0537385787575,5.79830382950879,-0.41681846170471));
#65674=CARTESIAN_POINT('Ctrl Pts',(52.1543084887152,5.29420174866827,2.4011440551771));
#65675=CARTESIAN_POINT('Ctrl Pts',(52.2548783986731,3.50626030117625,4.63683120565213));
#65676=CARTESIAN_POINT('Ctrl Pts',(52.3554483086308,0.868053748938764,5.74809078027364));
#65677=CARTESIAN_POINT('Ctrl Pts',(52.4560182185887,-1.98065509017138,5.46544328880053));
#65678=CARTESIAN_POINT('Ctrl Pts',(52.5565881285464,-4.34905677491859,3.85743050460308));
#65679=CARTESIAN_POINT('Ctrl Pts',(52.6389966451198,-5.4255710484936,1.77329999683277));
#65680=CARTESIAN_POINT('Ctrl Pts',(52.6878818583739,-5.57747516649707,0.424050447734582));
#65681=CARTESIAN_POINT('Ctrl Pts',(52.7032437683088,-5.57738099270237,3.53149720621823E-5));
#65682=CARTESIAN_POINT('Ctrl Pts',(51.7030928170571,-5.57739486550319,-5.00486370434358E-5));
#65683=CARTESIAN_POINT('Ctrl Pts',(51.717849595197,-5.57752346480075,-0.407359605634272));
#65684=CARTESIAN_POINT('Ctrl Pts',(51.7661296766563,-5.43351169352543,-1.73987383596617));
#65685=CARTESIAN_POINT('Ctrl Pts',(51.8479330614348,-4.38352629472378,-3.81821453267259));
#65686=CARTESIAN_POINT('Ctrl Pts',(51.9485029713925,-2.02966225553008,-5.44743390253828));
#65687=CARTESIAN_POINT('Ctrl Pts',(52.0490728813504,0.816393133438721,-5.75565524034613));
#65688=CARTESIAN_POINT('Ctrl Pts',(52.1496427913082,3.46447389032224,-4.66813513700239));
#65689=CARTESIAN_POINT('Ctrl Pts',(52.250212701266,5.27242271112307,-2.44859628140164));
#65690=CARTESIAN_POINT('Ctrl Pts',(52.3507826112238,5.80181356312538,0.364725064619975));
#65691=CARTESIAN_POINT('Ctrl Pts',(52.4513525211815,4.9242696204448,3.08960089643144));
#65692=CARTESIAN_POINT('Ctrl Pts',(52.5519224311394,2.85259453374416,5.06525117048629));
#65693=CARTESIAN_POINT('Ctrl Pts',(52.6524923410972,0.0891677282345522,
5.81258239599026));
#65694=CARTESIAN_POINT('Ctrl Pts',(52.753062251055,-2.6958821746702,5.15036739414614));
#65695=CARTESIAN_POINT('Ctrl Pts',(52.8536321610128,-4.82718297079972,3.23919273272347));
#65696=CARTESIAN_POINT('Ctrl Pts',(52.9269756830135,-5.52781083299589,1.27256351205078));
#65697=CARTESIAN_POINT('Ctrl Pts',(52.9667959016949,-5.57814066188418,0.173888795959752));
#65698=CARTESIAN_POINT('Ctrl Pts',(52.9730928170571,-5.57796455057653,0.000135314793302289));
#65699=CARTESIAN_POINT('Origin',(16.5082437683087,0.,0.));
#65700=CARTESIAN_POINT('',(50.1632437683087,-5.5779229988856,0.000138978711251798));
#65701=CARTESIAN_POINT('',(50.4330928170571,-5.5782539833292,-6.36399508394114E-5));
#65702=CARTESIAN_POINT('',(16.5082437683087,-5.57784,5.11151866531329E-13));
#65703=CARTESIAN_POINT('Ctrl Pts',(50.1632437683087,-5.5779229988856,0.000138978711251916));
#65704=CARTESIAN_POINT('Ctrl Pts',(50.1899892453782,-5.57716794349296,-0.737876265870143));
#65705=CARTESIAN_POINT('Ctrl Pts',(50.2502580257669,-5.24512519452518,-2.40159339675091));
#65706=CARTESIAN_POINT('Ctrl Pts',(50.3440501094749,-3.63848643265499,-4.53381532582656));
#65707=CARTESIAN_POINT('Ctrl Pts',(50.4446200194326,-1.0334150980172,-5.72067462494628));
#65708=CARTESIAN_POINT('Ctrl Pts',(50.5451899293905,1.82225850829634,-5.52027525203731));
#65709=CARTESIAN_POINT('Ctrl Pts',(50.6457598393482,4.23603599500043,-3.98121388252061));
#65710=CARTESIAN_POINT('Ctrl Pts',(50.7463297493061,5.62257839941823,-1.47671157363573));
#65711=CARTESIAN_POINT('Ctrl Pts',(50.8468996592638,5.64565038205386,1.38589202066021));
#65712=CARTESIAN_POINT('Ctrl Pts',(50.9474695692217,4.29965700697908,3.91241799296163));
#65713=CARTESIAN_POINT('Ctrl Pts',(51.0480394791794,1.91100050897997,5.4901859698914));
#65714=CARTESIAN_POINT('Ctrl Pts',(51.1486093891373,-0.941071967402673,
5.73658857523205));
#65715=CARTESIAN_POINT('Ctrl Pts',(51.249179299095,-3.56493530179192,4.59187338929895));
#65716=CARTESIAN_POINT('Ctrl Pts',(51.3440574254855,-5.22473285590304,2.46143864477682));
#65717=CARTESIAN_POINT('Ctrl Pts',(51.4054122485568,-5.57725579958518,0.76781752987093));
#65718=CARTESIAN_POINT('Ctrl Pts',(51.4332437683088,-5.57801596822771,-0.000129080508369864));
#65719=CARTESIAN_POINT('Ctrl Pts',(50.4330928170571,-5.5782539833292,-6.36399508389517E-5));
#65720=CARTESIAN_POINT('Ctrl Pts',(50.4353799853799,-5.5782906137371,-0.0631649816304534));
#65721=CARTESIAN_POINT('Ctrl Pts',(50.471190457022,-5.5618731054905,-1.05113124534463));
#65722=CARTESIAN_POINT('Ctrl Pts',(50.5405242319834,-5.01129836816094,-2.94634581461765));
#65723=CARTESIAN_POINT('Ctrl Pts',(50.6410941419411,-2.99744409122436,-4.98090292156266));
#65724=CARTESIAN_POINT('Ctrl Pts',(50.7416640518989,-0.256712202451727,
-5.80759535773281));
#65725=CARTESIAN_POINT('Ctrl Pts',(50.8422339618567,2.54627217443023,-5.2259509189974));
#65726=CARTESIAN_POINT('Ctrl Pts',(50.9428038718146,4.73178774091697,-3.37701788105352));
#65727=CARTESIAN_POINT('Ctrl Pts',(51.0433737817723,5.76984885348993,-0.709160913988021));
#65728=CARTESIAN_POINT('Ctrl Pts',(51.1439436917302,5.40872658594295,2.13066696425354));
#65729=CARTESIAN_POINT('Ctrl Pts',(51.2445136016879,3.73599277729174,4.45380993780282));
#65730=CARTESIAN_POINT('Ctrl Pts',(51.3450835116458,1.15728393619704,5.69690783540226));
#65731=CARTESIAN_POINT('Ctrl Pts',(51.4456534216035,-1.70206526320226,5.55851048697829));
#65732=CARTESIAN_POINT('Ctrl Pts',(51.5462233315614,-4.14866510146161,4.07217913038731));
#65733=CARTESIAN_POINT('Ctrl Pts',(51.6320364633792,-5.37784278716992,1.96133692425061));
#65734=CARTESIAN_POINT('Ctrl Pts',(51.6843262918778,-5.57723132289702,0.517934635056378));
#65735=CARTESIAN_POINT('Ctrl Pts',(51.7030928170571,-5.57739486550319,-5.00486370434358E-5));
#65736=CARTESIAN_POINT('Origin',(16.5082437683087,0.,0.));
#65737=CARTESIAN_POINT('',(48.8932437683088,-5.57740928288687,-6.1363554564314E-5));
#65738=CARTESIAN_POINT('',(49.1630928170571,-5.57763899819707,0.000132369982857178));
#65739=CARTESIAN_POINT('',(16.5082437683087,-5.57784,5.11151866531329E-13));
#65740=CARTESIAN_POINT('Ctrl Pts',(48.8932437683088,-5.57740928288687,-6.13635545640076E-5));
#65741=CARTESIAN_POINT('Ctrl Pts',(48.9075196355611,-5.57756230890984,-0.394094130874663));
#65742=CARTESIAN_POINT('Ctrl Pts',(48.9553188061326,-5.43970662246569,-1.71330876178174));
#65743=CARTESIAN_POINT('Ctrl Pts',(49.0366412800234,-4.41066789779351,-3.78682896691783));
#65744=CARTESIAN_POINT('Ctrl Pts',(49.1372111899812,-2.06849270248174,-5.43280800959264));
#65745=CARTESIAN_POINT('Ctrl Pts',(49.2377810999391,0.775290192564016,-5.76133578665817));
#65746=CARTESIAN_POINT('Ctrl Pts',(49.3383510098967,3.43106588330503,-4.69274459498218));
#65747=CARTESIAN_POINT('Ctrl Pts',(49.4389209198547,5.25481105090448,-2.48616687867213));
#65748=CARTESIAN_POINT('Ctrl Pts',(49.5394908298124,5.80426906215165,0.323304165552166));
#65749=CARTESIAN_POINT('Ctrl Pts',(49.6400607397703,4.94619682230831,3.05437422793956));
#65750=CARTESIAN_POINT('Ctrl Pts',(49.740630649728,2.88867611088328,5.04476116934454));
#65751=CARTESIAN_POINT('Ctrl Pts',(49.8412005596858,0.130653929224284,5.81179786985854));
#65752=CARTESIAN_POINT('Ctrl Pts',(49.9417704696436,-2.65905171780094,5.16947858989416));
#65753=CARTESIAN_POINT('Ctrl Pts',(50.0423403796015,-4.80393961224742,3.27356520191584));
#65754=CARTESIAN_POINT('Ctrl Pts',(50.1161648124898,-5.52327275317913,1.29912495283839));
#65755=CARTESIAN_POINT('Ctrl Pts',(50.1564659420589,-5.57811434466893,0.187166455713234));
#65756=CARTESIAN_POINT('Ctrl Pts',(50.1632437683087,-5.5779229988856,0.000138978711251916));
#65757=CARTESIAN_POINT('Ctrl Pts',(49.1630928170571,-5.57763899819707,0.000132369982857247));
#65758=CARTESIAN_POINT('Ctrl Pts',(49.186433678882,-5.57706759919496,-0.644030166077704));
#65759=CARTESIAN_POINT('Ctrl Pts',(49.2432978440262,-5.30539891262772,-2.21384039930619));
#65760=CARTESIAN_POINT('Ctrl Pts',(49.3336853124898,-3.86284675623355,-4.3442467623172));
#65761=CARTESIAN_POINT('Ctrl Pts',(49.4342552224475,-1.3210494073637,-5.66117421188848));
#65762=CARTESIAN_POINT('Ctrl Pts',(49.5348251324054,1.54110128559463,-5.60527178837798));
#65763=CARTESIAN_POINT('Ctrl Pts',(49.6353950423631,4.02953624342044,-4.19009578136448));
#65764=CARTESIAN_POINT('Ctrl Pts',(49.735964952321,5.54081213095715,-1.75882515432473));
#65765=CARTESIAN_POINT('Ctrl Pts',(49.8365348622786,5.70844584642674,1.09895905859165));
#65766=CARTESIAN_POINT('Ctrl Pts',(49.9371047722366,4.49178635813174,3.69024664581502));
#65767=CARTESIAN_POINT('Ctrl Pts',(50.0376746821943,2.18587254464829,5.38665259809838));
#65768=CARTESIAN_POINT('Ctrl Pts',(50.1382445921522,-0.650113479250571,
5.77679993232794));
#65769=CARTESIAN_POINT('Ctrl Pts',(50.2388145021098,-3.32844754406752,4.76607825580302));
#65770=CARTESIAN_POINT('Ctrl Pts',(50.337097243745,-5.15708123981284,2.64885721594067));
#65771=CARTESIAN_POINT('Ctrl Pts',(50.4018566820606,-5.57775371740881,0.861719031441649));
#65772=CARTESIAN_POINT('Ctrl Pts',(50.4330928170571,-5.5782539833292,-6.36399508389517E-5));
#65773=CARTESIAN_POINT('Origin',(16.5082437683087,0.,0.));
#65774=CARTESIAN_POINT('',(47.6232437683088,-5.57827554158207,-5.10498665022794E-5));
#65775=CARTESIAN_POINT('',(47.8930928170571,-5.577588863943,-0.000124534612764571));
#65776=CARTESIAN_POINT('',(16.5082437683087,-5.57784,5.11151866531329E-13));
#65777=CARTESIAN_POINT('Ctrl Pts',(47.6232437683088,-5.57827554158207,-5.10498665022129E-5));
#65778=CARTESIAN_POINT('Ctrl Pts',(47.6250500257439,-5.57829948763171,-0.0498838434567743));
#65779=CARTESIAN_POINT('Ctrl Pts',(47.6603795864984,-5.56550912456252,-1.0245779380622));
#65780=CARTESIAN_POINT('Ctrl Pts',(47.729232450572,-5.03220084112436,-2.91050161035883));
#65781=CARTESIAN_POINT('Ctrl Pts',(47.8298023605298,-3.03291992582039,-4.95938117640456));
#65782=CARTESIAN_POINT('Ctrl Pts',(47.9303722704876,-0.298158539329414,
-5.80561507634972));
#65783=CARTESIAN_POINT('Ctrl Pts',(48.0309421804455,2.50890603628552,-5.24399231792002));
#65784=CARTESIAN_POINT('Ctrl Pts',(48.1315120904031,4.70756305783949,-3.41070593657371));
#65785=CARTESIAN_POINT('Ctrl Pts',(48.2320820003611,5.76464009027266,-0.750326301641742));
#65786=CARTESIAN_POINT('Ctrl Pts',(48.3326519103187,5.42379686318222,2.09200681553594));
#65787=CARTESIAN_POINT('Ctrl Pts',(48.4332218202766,3.76768756572999,4.42703008080563));
#65788=CARTESIAN_POINT('Ctrl Pts',(48.5337917302344,1.19791727692173,5.6885023623944));
#65789=CARTESIAN_POINT('Ctrl Pts',(48.6343616401922,-1.6623469203385,5.57051771792849));
#65790=CARTESIAN_POINT('Ctrl Pts',(48.73493155015,-4.11949342041254,4.10168732212634));
#65791=CARTESIAN_POINT('Ctrl Pts',(48.8212255928555,-5.37067912645522,1.98789235424378));
#65792=CARTESIAN_POINT('Ctrl Pts',(48.8739963322418,-5.57720296557236,0.531193260999239));
#65793=CARTESIAN_POINT('Ctrl Pts',(48.8932437683088,-5.57740928288687,-6.13635545640076E-5));
#65794=CARTESIAN_POINT('Ctrl Pts',(47.8930928170571,-5.577588863943,-0.000124534612764085));
#65795=CARTESIAN_POINT('Ctrl Pts',(47.9039640690649,-5.57783588456841,-0.300157751719058));
#65796=CARTESIAN_POINT('Ctrl Pts',(47.948358624392,-5.48066132849218,-1.52523460204365));
#65797=CARTESIAN_POINT('Ctrl Pts',(48.0262764830383,-4.59631199877497,-3.55921072767047));
#65798=CARTESIAN_POINT('Ctrl Pts',(48.1268463929962,-2.34026552289286,-5.32139288874693));
#65799=CARTESIAN_POINT('Ctrl Pts',(48.2274163029538,0.483293327723093,-5.79314185510984));
#65800=CARTESIAN_POINT('Ctrl Pts',(48.3279862129118,3.18965396239895,-4.8600589085113));
#65801=CARTESIAN_POINT('Ctrl Pts',(48.4285561228695,5.12252625693867,-2.74841586027683));
#65802=CARTESIAN_POINT('Ctrl Pts',(48.5291260328273,5.81319034378827,0.0297156681595752));
#65803=CARTESIAN_POINT('Ctrl Pts',(48.629695942785,5.09416077643017,2.80064117264737));
#65804=CARTESIAN_POINT('Ctrl Pts',(48.730265852743,3.13980160598745,4.89241360364045));
#65805=CARTESIAN_POINT('Ctrl Pts',(48.8308357627007,0.424043248924028,5.79777994728061));
#65806=CARTESIAN_POINT('Ctrl Pts',(48.9314056726585,-2.39454523097487,5.29718964460052));
#65807=CARTESIAN_POINT('Ctrl Pts',(49.0319755826163,-4.63245855365558,3.51203541307753));
#65808=CARTESIAN_POINT('Ctrl Pts',(49.1092046307492,-5.48833418586149,1.48718441118965));
#65809=CARTESIAN_POINT('Ctrl Pts',(49.1529103755628,-5.57788827077974,0.281148014797861));
#65810=CARTESIAN_POINT('Ctrl Pts',(49.1630928170571,-5.57763899819707,0.000132369982857247));
#65811=CARTESIAN_POINT('Origin',(16.5082437683087,0.,0.));
#65812=CARTESIAN_POINT('',(46.3532437683088,-5.57760359476194,0.000127107498088562));
#65813=CARTESIAN_POINT('',(46.6230928170571,-5.57828356523297,4.54320993283769E-5));
#65814=CARTESIAN_POINT('',(16.5082437683087,-5.57784,5.11151866531329E-13));
#65815=CARTESIAN_POINT('Ctrl Pts',(46.3532437683088,-5.57760359476194,0.000127107498088495));
#65816=CARTESIAN_POINT('Ctrl Pts',(46.376103719246,-5.57707135817663,-0.63077470871854));
#65817=CARTESIAN_POINT('Ctrl Pts',(46.4324869735025,-5.3134714216754,-2.18730507792145));
#65818=CARTESIAN_POINT('Ctrl Pts',(46.5223935310784,-3.89375628397183,-4.31656425069105));
#65819=CARTESIAN_POINT('Ctrl Pts',(46.6229634410361,-1.36142352031365,-5.65160074029039));
#65820=CARTESIAN_POINT('Ctrl Pts',(46.723533350994,1.50105327506819,-5.61612891542932));
#65821=CARTESIAN_POINT('Ctrl Pts',(46.8241032609517,3.99952594339569,-4.21875066310145));
#65822=CARTESIAN_POINT('Ctrl Pts',(46.9246731709096,5.52811701335638,-1.79832900659305));
#65823=CARTESIAN_POINT('Ctrl Pts',(47.0252430808674,5.71614446633981,1.05818588596099));
#65824=CARTESIAN_POINT('Ctrl Pts',(47.1258129908252,4.5180118068569,3.65809161208624));
#65825=CARTESIAN_POINT('Ctrl Pts',(47.226382900783,2.22426517344535,5.37091327127076));
#65826=CARTESIAN_POINT('Ctrl Pts',(47.3269528107408,-0.608863849815457,
5.78129308560828));
#65827=CARTESIAN_POINT('Ctrl Pts',(47.4275227206986,-3.29434391362348,4.78971430338867));
#65828=CARTESIAN_POINT('Ctrl Pts',(47.5262863732212,-5.14706458748218,2.675303717135));
#65829=CARTESIAN_POINT('Ctrl Pts',(47.5915267224247,-5.57785506001607,0.874989777696537));
#65830=CARTESIAN_POINT('Ctrl Pts',(47.6232437683088,-5.57827554158207,-5.10498665022129E-5));
#65831=CARTESIAN_POINT('Ctrl Pts',(46.6230928170571,-5.57828356523297,4.54320993282641E-5));
#65832=CARTESIAN_POINT('Ctrl Pts',(46.655017762567,-5.57790150280944,-0.880727451819953));
#65833=CARTESIAN_POINT('Ctrl Pts',(46.7204660113962,-5.14269869890383,-2.68673433595031));
#65834=CARTESIAN_POINT('Ctrl Pts',(46.8194375635447,-3.27954872353672,-4.79985678577976));
#65835=CARTESIAN_POINT('Ctrl Pts',(46.9200074735025,-0.591021750409563,
-5.78314432507005));
#65836=CARTESIAN_POINT('Ctrl Pts',(47.0205773834603,2.24082748842343,-5.36402434382742));
#65837=CARTESIAN_POINT('Ctrl Pts',(47.1211472934181,4.52927799028237,-3.64413307671263));
#65838=CARTESIAN_POINT('Ctrl Pts',(47.2217172033759,5.71938247843022,-1.04054267546927));
#65839=CARTESIAN_POINT('Ctrl Pts',(47.3222871133337,5.52254163896719,1.8153784288464));
#65840=CARTESIAN_POINT('Ctrl Pts',(47.4228570232915,3.98648920601686,4.23107182689664));
#65841=CARTESIAN_POINT('Ctrl Pts',(47.5234269332493,1.48371657229165,5.62073394915242));
#65842=CARTESIAN_POINT('Ctrl Pts',(47.6239968432071,-1.37885605298849,5.64737292722768));
#65843=CARTESIAN_POINT('Ctrl Pts',(47.7245667531649,-3.90705727237777,4.30452883187085));
#65844=CARTESIAN_POINT('Ctrl Pts',(47.8142654111149,-5.31692771113889,2.17583281045649));
#65845=CARTESIAN_POINT('Ctrl Pts',(47.8704407657456,-5.57707415562073,0.62504428901131));
#65846=CARTESIAN_POINT('Ctrl Pts',(47.8930928170571,-5.577588863943,-0.000124534612764085));
#65847=CARTESIAN_POINT('Origin',(16.5082437683087,0.,0.));
#65848=CARTESIAN_POINT('',(45.0832437683088,-5.57762347393826,-0.000130215119483779));
#65849=CARTESIAN_POINT('',(45.3530928170571,-5.57741643618798,6.6124065845885E-5));
#65850=CARTESIAN_POINT('',(16.5082437683087,-5.57784,5.11151866531329E-13));
#65851=CARTESIAN_POINT('Ctrl Pts',(45.0832437683088,-5.57762347393826,-0.000130215119483572));
#65852=CARTESIAN_POINT('Ctrl Pts',(45.0936341094289,-5.57787263228915,-0.286885775923387));
#65853=CARTESIAN_POINT('Ctrl Pts',(45.1375477538683,-5.48603989704716,-1.49866881654569));
#65854=CARTESIAN_POINT('Ctrl Pts',(45.2149847016269,-4.62159948960023,-3.52631295931618));
#65855=CARTESIAN_POINT('Ctrl Pts',(45.3155546115848,-2.3781884143173,-5.30455321354411));
#65856=CARTESIAN_POINT('Ctrl Pts',(45.4161245215426,0.441931304224746,-5.79644387979909));
#65857=CARTESIAN_POINT('Ctrl Pts',(45.5166944315003,3.15488306191939,-4.88270189494794));
#65858=CARTESIAN_POINT('Ctrl Pts',(45.6172643414582,5.1027783929124,-2.78490890374179));
#65859=CARTESIAN_POINT('Ctrl Pts',(45.717834251416,5.81325435624223,-0.0117779007076735));
#65860=CARTESIAN_POINT('Ctrl Pts',(45.8184041613737,5.11402114239932,2.76420923310936));
#65861=CARTESIAN_POINT('Ctrl Pts',(45.9189740713316,3.1746422038206,4.86987800740792));
#65862=CARTESIAN_POINT('Ctrl Pts',(46.0195439812894,0.465415263638452,5.79460555704065));
#65863=CARTESIAN_POINT('Ctrl Pts',(46.1201138912472,-2.35667447733314,5.3141462472537));
#65864=CARTESIAN_POINT('Ctrl Pts',(46.220683801205,-4.60727268624445,3.54501104707727));
#65865=CARTESIAN_POINT('Ctrl Pts',(46.2983937602255,-5.4829987578168,1.51375007970848));
#65866=CARTESIAN_POINT('Ctrl Pts',(46.3425804159268,-5.57785186416004,0.294420319378661));
#65867=CARTESIAN_POINT('Ctrl Pts',(46.3532437683088,-5.57760359476194,0.000127107498088495));
#65868=CARTESIAN_POINT('Ctrl Pts',(45.3530928170571,-5.57741643618798,6.61240658456769E-5));
#65869=CARTESIAN_POINT('Ctrl Pts',(45.3725481527499,-5.57719134984669,-0.536924835055485));
#65870=CARTESIAN_POINT('Ctrl Pts',(45.4255267917619,-5.36754962672399,-1.99937184209296));
#65871=CARTESIAN_POINT('Ctrl Pts',(45.5120287340932,-4.1068173316415,-4.11437922396275));
#65872=CARTESIAN_POINT('Ctrl Pts',(45.6125986440511,-1.64515019125313,-5.57562066879259));
#65873=CARTESIAN_POINT('Ctrl Pts',(45.7131685540088,1.21546445432158,-5.68477890109438));
#65874=CARTESIAN_POINT('Ctrl Pts',(45.8137384639667,3.78133001603,-4.41538314350158));
#65875=CARTESIAN_POINT('Ctrl Pts',(45.9143083739244,5.43022630392851,-2.07526077449805));
#65876=CARTESIAN_POINT('Ctrl Pts',(46.0148782838823,5.76229738761891,0.768110545877321));
#65877=CARTESIAN_POINT('Ctrl Pts',(46.11544819384,4.69701631516247,3.42521572008903));
#65878=CARTESIAN_POINT('Ctrl Pts',(46.2160181037979,2.4927128296055,5.25170903070299));
#65879=CARTESIAN_POINT('Ctrl Pts',(46.3165880137556,-0.316071371332041,
5.80466742219323));
#65880=CARTESIAN_POINT('Ctrl Pts',(46.4171579237135,-3.04820853680487,4.94999896062587));
#65881=CARTESIAN_POINT('Ctrl Pts',(46.5177278336712,-5.04115775608791,2.89496001220778));
#65882=CARTESIAN_POINT('Ctrl Pts',(46.5863727981191,-5.56705141744763,1.01309914407614));
#65883=CARTESIAN_POINT('Ctrl Pts',(46.6214944592478,-5.57830269361201,0.0441423035201426));
#65884=CARTESIAN_POINT('Ctrl Pts',(46.6230928170571,-5.57828356523297,4.54320993282641E-5));
#65885=CARTESIAN_POINT('Origin',(16.5082437683087,0.,0.));
#65886=CARTESIAN_POINT('',(43.8132437683088,-5.57826379807651,5.82713151345457E-5));
#65887=CARTESIAN_POINT('',(44.0830928170571,-5.57790494923753,-0.000140205289279327));
#65888=CARTESIAN_POINT('',(16.5082437683087,-5.57784,5.11151866531329E-13));
#65889=CARTESIAN_POINT('Ctrl Pts',(43.8132437683088,-5.57826379807651,5.82713151345022E-5));
#65890=CARTESIAN_POINT('Ctrl Pts',(43.844687802931,-5.5777964967119,-0.867455764163641));
#65891=CARTESIAN_POINT('Ctrl Pts',(43.9096551408726,-5.15276511634523,-2.66029104170784));
#65892=CARTESIAN_POINT('Ctrl Pts',(44.0081457821333,-3.31372511850974,-4.77632607432447));
#65893=CARTESIAN_POINT('Ctrl Pts',(44.1087156920912,-0.632285046713879,
-5.77877846512705));
#65894=CARTESIAN_POINT('Ctrl Pts',(44.2092856020489,2.202483604621,-5.37988205267457));
#65895=CARTESIAN_POINT('Ctrl Pts',(44.3098555120068,4.50315187779634,-3.67636887360525));
#65896=CARTESIAN_POINT('Ctrl Pts',(44.4104254219645,5.71180969704834,-1.08133940741041));
#65897=CARTESIAN_POINT('Ctrl Pts',(44.5109953319224,5.53535858165572,1.77591393423347));
#65898=CARTESIAN_POINT('Ctrl Pts',(44.6115652418801,4.01658777520697,4.20250967558343));
#65899=CARTESIAN_POINT('Ctrl Pts',(44.712135151838,1.52379789086441,5.61000043824521));
#65900=CARTESIAN_POINT('Ctrl Pts',(44.8127050617957,-1.33851167028378,5.65707092388173));
#65901=CARTESIAN_POINT('Ctrl Pts',(44.9132749717536,-3.87623330361735,4.33230658024589));
#65902=CARTESIAN_POINT('Ctrl Pts',(45.0034545405912,-5.30890197702976,2.20236946067521));
#65903=CARTESIAN_POINT('Ctrl Pts',(45.0601108061096,-5.57706875002244,0.638299791343409));
#65904=CARTESIAN_POINT('Ctrl Pts',(45.0832437683088,-5.57762347393826,-0.000130215119483572));
#65905=CARTESIAN_POINT('Ctrl Pts',(44.0830928170571,-5.57790494923753,-0.000140205289278963));
#65906=CARTESIAN_POINT('Ctrl Pts',(44.0900785429327,-5.5781024864199,-0.192906266953961));
#65907=CARTESIAN_POINT('Ctrl Pts',(44.1305875721276,-5.52128067157015,-1.31060778880162));
#65908=CARTESIAN_POINT('Ctrl Pts',(44.2046199046419,-4.79381558281113,-3.28837302507556));
#65909=CARTESIAN_POINT('Ctrl Pts',(44.3051898145996,-2.64308772173875,-5.17765895837504));
#65910=CARTESIAN_POINT('Ctrl Pts',(44.4057597245574,0.148586636609559,-5.81136705134586));
#65911=CARTESIAN_POINT('Ctrl Pts',(44.5063296345153,2.90422886348763,-5.03582363695677));
#65912=CARTESIAN_POINT('Ctrl Pts',(44.606899544473,4.95559809101348,-3.03909732558712));
#65913=CARTESIAN_POINT('Ctrl Pts',(44.7074694544309,5.80523904738957,-0.305392528904701));
#65914=CARTESIAN_POINT('Ctrl Pts',(44.8080393643886,5.24711453208993,2.50236969314653));
#65915=CARTESIAN_POINT('Ctrl Pts',(44.9086092743465,3.41656925962507,4.70330941872129));
#65916=CARTESIAN_POINT('Ctrl Pts',(45.0091791843043,0.757508882781974,5.76370065899971));
#65917=CARTESIAN_POINT('Ctrl Pts',(45.109749094262,-2.08524674605032,5.42639945102955));
#65918=CARTESIAN_POINT('Ctrl Pts',(45.2103190042198,-4.42233183400564,3.77320104738504));
#65919=CARTESIAN_POINT('Ctrl Pts',(45.2914335784849,-5.44235309585835,1.701824445005));
#65920=CARTESIAN_POINT('Ctrl Pts',(45.3390248494306,-5.57757919397393,0.388359163462492));
#65921=CARTESIAN_POINT('Ctrl Pts',(45.3530928170571,-5.57741643618798,6.61240658456769E-5));
#65922=CARTESIAN_POINT('Origin',(16.5082437683087,0.,0.));
#65923=CARTESIAN_POINT('',(42.5432437683088,-5.57740073011504,5.4988692936847E-5));
#65924=CARTESIAN_POINT('',(42.8130928170571,-5.57803330847514,0.000126527485840092));
#65925=CARTESIAN_POINT('',(16.5082437683087,-5.57784,5.11151866531329E-13));
#65926=CARTESIAN_POINT('Ctrl Pts',(42.5432437683088,-5.57740073011504,5.49886929369914E-5));
#65927=CARTESIAN_POINT('Ctrl Pts',(42.5622181931139,-5.57721881714937,-0.523666463456379));
#65928=CARTESIAN_POINT('Ctrl Pts',(42.6147159212383,-5.37475882476217,-1.97281714130688));
#65929=CARTESIAN_POINT('Ctrl Pts',(42.7007369526818,-4.13607991865755,-4.08496117922704));
#65930=CARTESIAN_POINT('Ctrl Pts',(42.8013068626397,-1.68490539227271,-5.56373604230149));
#65931=CARTESIAN_POINT('Ctrl Pts',(42.9018767725975,1.1748572413234,-5.69330970454131));
#65932=CARTESIAN_POINT('Ctrl Pts',(43.0024466825553,3.74971800524932,-4.4422606643941));
#65933=CARTESIAN_POINT('Ctrl Pts',(43.1030165925131,5.41527538076706,-2.11396723715677));
#65934=CARTESIAN_POINT('Ctrl Pts',(43.2035865024709,5.76763313807318,0.726961425327436));
#65935=CARTESIAN_POINT('Ctrl Pts',(43.3041564124287,4.72134482434061,3.39160256795904));
#65936=CARTESIAN_POINT('Ctrl Pts',(43.4047263223865,2.5301344549744,5.23378300744937));
#65937=CARTESIAN_POINT('Ctrl Pts',(43.5052962323444,-0.274631341710833,
5.80677557302366));
#65938=CARTESIAN_POINT('Ctrl Pts',(43.6058661423021,-3.01279927444167,4.97163006077864));
#65939=CARTESIAN_POINT('Ctrl Pts',(43.7064360522599,-5.02036597662438,2.93086853851659));
#65940=CARTESIAN_POINT('Ctrl Pts',(43.7755619275955,-5.56345669958936,1.03965202892801));
#65941=CARTESIAN_POINT('Ctrl Pts',(43.8111644996118,-5.57829469885344,0.0574235172151608));
#65942=CARTESIAN_POINT('Ctrl Pts',(43.8132437683088,-5.57826379807651,5.82713151345022E-5));
#65943=CARTESIAN_POINT('Ctrl Pts',(42.8130928170571,-5.57803330847514,0.000126527485840109));
#65944=CARTESIAN_POINT('Ctrl Pts',(42.8411322364349,-5.57727619059748,-0.77354965244955));
#65945=CARTESIAN_POINT('Ctrl Pts',(42.9026949591319,-5.22076416624656,-2.47289174149367));
#65946=CARTESIAN_POINT('Ctrl Pts',(42.9977809851481,-3.55074929685554,-4.60285177090544));
#65947=CARTESIAN_POINT('Ctrl Pts',(43.0983508951061,-0.923366230433899,
-5.73946511432395));
#65948=CARTESIAN_POINT('Ctrl Pts',(43.1989208050638,1.92793235200782,-5.48426310821507));
#65949=CARTESIAN_POINT('Ctrl Pts',(43.2994907150216,4.31170899870712,-3.89913201937502));
#65950=CARTESIAN_POINT('Ctrl Pts',(43.4000606249794,5.64989992486267,-1.36846477232117));
#65951=CARTESIAN_POINT('Ctrl Pts',(43.5006305349373,5.61799498283493,1.49405400400684));
#65952=CARTESIAN_POINT('Ctrl Pts',(43.601200444895,4.22373109360091,3.99426597048771));
#65953=CARTESIAN_POINT('Ctrl Pts',(43.7017703548528,1.80521605007753,5.52587187750403));
#65954=CARTESIAN_POINT('Ctrl Pts',(43.8023402648106,-1.05106233160792,5.71745861105458));
#65955=CARTESIAN_POINT('Ctrl Pts',(43.9029101747684,-3.65245900266303,4.52256655317676));
#65956=CARTESIAN_POINT('Ctrl Pts',(43.9964943588506,-5.24896409347016,2.39013445685884));
#65957=CARTESIAN_POINT('Ctrl Pts',(44.0565552396135,-5.57715453927749,0.732145083454281));
#65958=CARTESIAN_POINT('Ctrl Pts',(44.0830928170571,-5.57790494923753,-0.000140205289278963));
#65959=CARTESIAN_POINT('Origin',(16.5082437683087,0.,0.));
#65960=CARTESIAN_POINT('',(41.2732437683088,-5.57794663527581,-0.000137039997376016));
#65961=CARTESIAN_POINT('',(41.5430928170571,-5.57737735400439,-3.01529304447268E-5));
#65962=CARTESIAN_POINT('',(16.5082437683087,-5.57784,5.11151866531329E-13));
#65963=CARTESIAN_POINT('Ctrl Pts',(41.2732437683088,-5.57794663527581,-0.000137039997375726));
#65964=CARTESIAN_POINT('Ctrl Pts',(41.2797485832967,-5.57812947862225,-0.179628846193896));
#65965=CARTESIAN_POINT('Ctrl Pts',(41.319776701604,-5.52586098423105,-1.28404603494069));
#65966=CARTESIAN_POINT('Ctrl Pts',(41.3933281232305,-4.81716488388169,-3.25407243478249));
#65967=CARTESIAN_POINT('Ctrl Pts',(41.4938980331883,-2.6799769691159,-5.15866149057317));
#65968=CARTESIAN_POINT('Ctrl Pts',(41.5944679431461,0.107103053659489,-5.81227957562358));
#65969=CARTESIAN_POINT('Ctrl Pts',(41.6950378531039,2.8682106781198,-5.0564248669622));
#65970=CARTESIAN_POINT('Ctrl Pts',(41.7956077630617,4.93377968217404,-3.07439148077804));
#65971=CARTESIAN_POINT('Ctrl Pts',(41.8961776730195,5.80291136044017,-0.346820807029599));
#65972=CARTESIAN_POINT('Ctrl Pts',(41.9967475829773,5.26484202911207,2.46485361387027));
#65973=CARTESIAN_POINT('Ctrl Pts',(42.0973174929351,3.4500530378513,4.67880315522326));
#65974=CARTESIAN_POINT('Ctrl Pts',(42.1978874028929,0.798629154816186,5.75814695908256));
#65975=CARTESIAN_POINT('Ctrl Pts',(42.2984573128507,-2.04646161077897,5.44114508214238));
#65976=CARTESIAN_POINT('Ctrl Pts',(42.3990272228085,-4.39528719741307,3.80467020667639));
#65977=CARTESIAN_POINT('Ctrl Pts',(42.4806227079612,-5.43620232966336,1.72838970928726));
#65978=CARTESIAN_POINT('Ctrl Pts',(42.5286948897946,-5.57754021416608,0.401624989409368));
#65979=CARTESIAN_POINT('Ctrl Pts',(42.5432437683088,-5.57740073011504,5.49886929369914E-5));
#65980=CARTESIAN_POINT('Ctrl Pts',(41.5430928170571,-5.57737735400439,-3.0152930444588E-5));
#65981=CARTESIAN_POINT('Ctrl Pts',(41.5586626266178,-5.57745878542451,-0.429784476705716));
#65982=CARTESIAN_POINT('Ctrl Pts',(41.6077557394976,-5.42280542730085,-1.7847836899185));
#65983=CARTESIAN_POINT('Ctrl Pts',(41.6903721556968,-4.33713329105347,-3.87083192733591));
#65984=CARTESIAN_POINT('Ctrl Pts',(41.7909420656546,-1.96378107173494,-5.4715289358956));
#65985=CARTESIAN_POINT('Ctrl Pts',(41.8915119756124,0.88578636700025,-5.74538488754965));
#65986=CARTESIAN_POINT('Ctrl Pts',(41.9920818855702,3.52055137424819,-4.62598994976497));
#65987=CARTESIAN_POINT('Ctrl Pts',(42.0926517955281,5.30158570383253,-2.38479643134711));
#65988=CARTESIAN_POINT('Ctrl Pts',(42.1932217054858,5.7969900639945,0.434708168771271));
#65989=CARTESIAN_POINT('Ctrl Pts',(42.2937916154436,4.88662932385308,3.14879641217187));
#65990=CARTESIAN_POINT('Ctrl Pts',(42.3943615254014,2.79126517922797,5.09930423619505));
#65991=CARTESIAN_POINT('Ctrl Pts',(42.4949314353592,0.0190216314411856,
5.81323517256825));
#65992=CARTESIAN_POINT('Ctrl Pts',(42.595501345317,-2.75783464559572,5.11746158379321));
#65993=CARTESIAN_POINT('Ctrl Pts',(42.6960712552748,-4.86591839509884,3.18070796620598));
#65994=CARTESIAN_POINT('Ctrl Pts',(42.7686017458548,-5.53526120505294,1.22766026552409));
#65995=CARTESIAN_POINT('Ctrl Pts',(42.8076089331156,-5.57818138381562,0.151440301922733));
#65996=CARTESIAN_POINT('Ctrl Pts',(42.8130928170571,-5.57803330847514,0.000126527485840109));
#65997=CARTESIAN_POINT('Origin',(16.5082437683087,0.,0.));
#65998=CARTESIAN_POINT('',(40.0032437683088,-5.57799292358802,0.000132115289384061));
#65999=CARTESIAN_POINT('',(40.2730928170571,-5.57820901493156,-8.33809270067709E-5));
#66000=CARTESIAN_POINT('',(16.5082437683087,-5.57784,5.11151866531329E-13));
#66001=CARTESIAN_POINT('Ctrl Pts',(40.0032437683088,-5.57799292358802,0.00013211528938413));
#66002=CARTESIAN_POINT('Ctrl Pts',(40.0308022767989,-5.57723081277639,-0.760290445687694));
#66003=CARTESIAN_POINT('Ctrl Pts',(40.0918840886083,-5.22991270231027,-2.44639707817582));
#66004=CARTESIAN_POINT('Ctrl Pts',(40.1864892037368,-3.58351262028272,-4.57739032960799));
#66005=CARTESIAN_POINT('Ctrl Pts',(40.2870591136947,-0.964309291247043,
-5.73272819171892));
#66006=CARTESIAN_POINT('Ctrl Pts',(40.3876290236525,1.88873821081094,-5.49788440223482));
#66007=CARTESIAN_POINT('Ctrl Pts',(40.4881989336103,4.28376832262728,-3.92980837794532));
#66008=CARTESIAN_POINT('Ctrl Pts',(40.5887688435681,5.63998830379708,-1.40875720489588));
#66009=CARTESIAN_POINT('Ctrl Pts',(40.6893387535259,5.62851597635984,1.45391637764221));
#66010=CARTESIAN_POINT('Ctrl Pts',(40.7899086634837,4.25213336984329,3.964016490175));
#66011=CARTESIAN_POINT('Ctrl Pts',(40.8904785734415,1.84461208149807,5.51284601617945));
#66012=CARTESIAN_POINT('Ctrl Pts',(40.9910484833993,-1.01022604871547,5.7248151288763));
#66013=CARTESIAN_POINT('Ctrl Pts',(41.0916183933571,-3.62008523174703,4.54852150090567));
#66014=CARTESIAN_POINT('Ctrl Pts',(41.1856834883269,-5.24005244945936,2.41663978755469));
#66015=CARTESIAN_POINT('Ctrl Pts',(41.2462252799775,-5.57718717465606,0.745402576464613));
#66016=CARTESIAN_POINT('Ctrl Pts',(41.2732437683088,-5.57794663527581,-0.000137039997375726));
#66017=CARTESIAN_POINT('Ctrl Pts',(40.2730928170571,-5.57820901493156,-8.33809270062505E-5));
#66018=CARTESIAN_POINT('Ctrl Pts',(40.2761930168006,-5.57827097512514,-0.0856176805388213));
#66019=CARTESIAN_POINT('Ctrl Pts',(40.3128165198633,-5.55550823955623,-1.09602464080041));
#66020=CARTESIAN_POINT('Ctrl Pts',(40.3829633262454,-4.9753803739444,-3.00660192386958));
#66021=CARTESIAN_POINT('Ctrl Pts',(40.4835332362031,-2.93712200893205,-5.01671000743458));
#66022=CARTESIAN_POINT('Ctrl Pts',(40.584103146161,-0.186614085112543,-5.81027023272455));
#66023=CARTESIAN_POINT('Ctrl Pts',(40.6846730561188,2.609147593704,-5.19484492822605));
#66024=CARTESIAN_POINT('Ctrl Pts',(40.7852429660765,4.7721932270764,-3.31967420050424));
#66025=CARTESIAN_POINT('Ctrl Pts',(40.8858128760344,5.77798611092356,-0.639485336830895));
#66026=CARTESIAN_POINT('Ctrl Pts',(40.9863827859921,5.38262233672791,2.19577817053662));
#66027=CARTESIAN_POINT('Ctrl Pts',(41.08695269595,3.6819772793914,4.49856736173782));
#66028=CARTESIAN_POINT('Ctrl Pts',(41.1875226059078,1.08845590135412,5.7104578402134));
#66029=CARTESIAN_POINT('Ctrl Pts',(41.2880925158656,-1.76901509578748,5.53756720816311));
#66030=CARTESIAN_POINT('Ctrl Pts',(41.3886624258233,-4.19750145501954,4.02182129502992));
#66031=CARTESIAN_POINT('Ctrl Pts',(41.4736625262206,-5.38971481780673,1.91643858201631));
#66032=CARTESIAN_POINT('Ctrl Pts',(41.5251393232985,-5.57728345571441,0.495518077098019));
#66033=CARTESIAN_POINT('Ctrl Pts',(41.5430928170571,-5.57737735400439,-3.0152930444588E-5));
#66034=CARTESIAN_POINT('Origin',(16.5082437683087,0.,0.));
#66035=CARTESIAN_POINT('',(38.7332437683088,-5.57738665159885,-4.20214438878431E-5));
#66036=CARTESIAN_POINT('',(39.0030928170571,-5.57770250057755,0.000138966530263268));
#66037=CARTESIAN_POINT('',(16.5082437683087,-5.57784,5.11151866531329E-13));
#66038=CARTESIAN_POINT('Ctrl Pts',(38.7332437683088,-5.57738665159885,-4.20214438870761E-5));
#66039=CARTESIAN_POINT('Ctrl Pts',(38.7483326669818,-5.57749685500109,-0.416520364740088));
#66040=CARTESIAN_POINT('Ctrl Pts',(38.796944868974,-5.42917366098025,-1.75821956594524));
#66041=CARTESIAN_POINT('Ctrl Pts',(38.8790803742854,-4.36465164317584,-3.8397761605381));
#66042=CARTESIAN_POINT('Ctrl Pts',(38.9796502842433,-2.00278518012054,-5.45737266929827));
#66043=CARTESIAN_POINT('Ctrl Pts',(39.080220194201,0.844754965059067,-5.75156100361652));
#66044=CARTESIAN_POINT('Ctrl Pts',(39.1807901041589,3.48744275840115,-4.65100074566642));
#66045=CARTESIAN_POINT('Ctrl Pts',(39.2813600141166,5.28442868492169,-2.42257681060703));
#66046=CARTESIAN_POINT('Ctrl Pts',(39.3819299240745,5.79994520433648,0.39331991560096));
#66047=CARTESIAN_POINT('Ctrl Pts',(39.4824998340322,4.90898000445885,3.11383690085679));
#66048=CARTESIAN_POINT('Ctrl Pts',(39.5830697439901,2.8275913792907,5.07925111813494));
#66049=CARTESIAN_POINT('Ctrl Pts',(39.6836396539479,0.0605142787163216,
5.8129513116304));
#66050=CARTESIAN_POINT('Ctrl Pts',(39.7842095639056,-2.72123748235436,5.13701581601069));
#66051=CARTESIAN_POINT('Ctrl Pts',(39.8847794738635,-4.84309149647335,3.21535840709891));
#66052=CARTESIAN_POINT('Ctrl Pts',(39.9577908753311,-5.530887896341,1.25422042093262));
#66053=CARTESIAN_POINT('Ctrl Pts',(39.9972789734796,-5.57815787571633,0.164718836712659));
#66054=CARTESIAN_POINT('Ctrl Pts',(40.0032437683088,-5.57799292358802,0.00013211528938413));
#66055=CARTESIAN_POINT('Ctrl Pts',(39.0030928170571,-5.57770250057755,0.00013896653026358));
#66056=CARTESIAN_POINT('Ctrl Pts',(39.0272467103027,-5.57707034665817,-0.666439870181227));
#66057=CARTESIAN_POINT('Ctrl Pts',(39.0849239068676,-5.29150453091099,-2.25869376639851));
#66058=CARTESIAN_POINT('Ctrl Pts',(39.1761244067517,-3.81014410570237,-4.39054289215228));
#66059=CARTESIAN_POINT('Ctrl Pts',(39.2766943167096,-1.25264064176956,-5.67670295300313));
#66060=CARTESIAN_POINT('Ctrl Pts',(39.3772642266673,1.60862709948338,-5.58626743441943));
#66061=CARTESIAN_POINT('Ctrl Pts',(39.4778341366252,4.07980415386393,-4.14116687180823));
#66062=CARTESIAN_POINT('Ctrl Pts',(39.578404046583,5.5616322129449,-1.69183690761873));
#66063=CARTESIAN_POINT('Ctrl Pts',(39.6789739565408,5.69476924799924,1.16776205028657));
#66064=CARTESIAN_POINT('Ctrl Pts',(39.7795438664986,4.44692964263445,3.74417971624045));
#66065=CARTESIAN_POINT('Ctrl Pts',(39.8801137764563,2.12071342697536,5.41263702410329));
#66066=CARTESIAN_POINT('Ctrl Pts',(39.9806836864142,-0.719773969154297,
5.76853451297425));
#66067=CARTESIAN_POINT('Ctrl Pts',(40.081253596372,-3.38571679736614,4.72556734816892));
#66068=CARTESIAN_POINT('Ctrl Pts',(40.1787233065863,-5.17375445747103,2.6041302969216));
#66069=CARTESIAN_POINT('Ctrl Pts',(40.2426697134813,-5.57760098269404,0.839287973076047));
#66070=CARTESIAN_POINT('Ctrl Pts',(40.2730928170571,-5.57820901493156,-8.33809270062505E-5));
#66071=CARTESIAN_POINT('Origin',(16.5082437683087,0.,0.));
#66072=CARTESIAN_POINT('',(37.4632437683088,-5.57823681479003,-7.19583867586569E-5));
#66073=CARTESIAN_POINT('',(37.7330928170571,-5.5775348825402,-0.000112846948039924));
#66074=CARTESIAN_POINT('',(16.5082437683087,-5.57784,5.11151866531329E-13));
#66075=CARTESIAN_POINT('Ctrl Pts',(37.4632437683088,-5.57823681479003,-7.19583867583775E-5));
#66076=CARTESIAN_POINT('Ctrl Pts',(37.4658630571646,-5.57828328322656,-0.0723369141437499));
#66077=CARTESIAN_POINT('Ctrl Pts',(37.5020056493397,-5.55930617745199,-1.06946971283999));
#66078=CARTESIAN_POINT('Ctrl Pts',(37.5716715448341,-4.99671385197042,-2.97101255649336));
#66079=CARTESIAN_POINT('Ctrl Pts',(37.6722414547918,-2.97285496046918,-4.99561791106246));
#66080=CARTESIAN_POINT('Ctrl Pts',(37.7728113647497,-0.228081300173006,
-5.80879022257005));
#66081=CARTESIAN_POINT('Ctrl Pts',(37.8733812747074,2.57200187907619,-5.21333590547767));
#66082=CARTESIAN_POINT('Ctrl Pts',(37.9739511846653,4.74837681670243,-3.35365211909601));
#66083=CARTESIAN_POINT('Ctrl Pts',(38.074521094623,5.77327446381726,-0.680710580753474));
#66084=CARTESIAN_POINT('Ctrl Pts',(38.1750910045808,5.39815802325663,2.15730268744658));
#66085=CARTESIAN_POINT('Ctrl Pts',(38.2756609145386,3.71399290894551,4.47217191100887));
#66086=CARTESIAN_POINT('Ctrl Pts',(38.3762308244964,1.1291877113267,5.70254329592533));
#66087=CARTESIAN_POINT('Ctrl Pts',(38.4768007344543,-1.72944453425166,5.55005284049271));
#66088=CARTESIAN_POINT('Ctrl Pts',(38.5773706444121,-4.16868796902945,4.05167934888527));
#66089=CARTESIAN_POINT('Ctrl Pts',(38.6628516556969,-5.38272866987952,1.94299661298295));
#66090=CARTESIAN_POINT('Ctrl Pts',(38.7148093636625,-5.57725201393216,0.508777772045055));
#66091=CARTESIAN_POINT('Ctrl Pts',(38.7332437683088,-5.57738665159885,-4.20214438870761E-5));
#66092=CARTESIAN_POINT('Ctrl Pts',(37.7330928170571,-5.5775348825402,-0.000112846948039542));
#66093=CARTESIAN_POINT('Ctrl Pts',(37.7447771004856,-5.5777721557373,-0.32259368260295));
#66094=CARTESIAN_POINT('Ctrl Pts',(37.7899846872333,-5.47134065168775,-1.57014734993002));
#66095=CARTESIAN_POINT('Ctrl Pts',(37.8687155773003,-4.55302886484057,-3.61441463448453));
#66096=CARTESIAN_POINT('Ctrl Pts',(37.9692854872581,-2.27588264393015,-5.34924510422778));
#66097=CARTESIAN_POINT('Ctrl Pts',(38.0698553972159,0.553163158988311,-5.78688824097939));
#66098=CARTESIAN_POINT('Ctrl Pts',(38.1704253071738,3.24806737203082,-4.82121596081281));
#66099=CARTESIAN_POINT('Ctrl Pts',(38.2709952171315,5.15531804338536,-2.6864029603901));
#66100=CARTESIAN_POINT('Ctrl Pts',(38.3715651270894,5.81240852706456,0.0998604453944716));
#66101=CARTESIAN_POINT('Ctrl Pts',(38.4721350370471,5.0599949464186,2.86190777913362));
#66102=CARTESIAN_POINT('Ctrl Pts',(38.572704947005,3.08053694705489,4.92994494004518));
#66103=CARTESIAN_POINT('Ctrl Pts',(38.6732748569627,0.354051389844875,5.80247469683378));
#66104=CARTESIAN_POINT('Ctrl Pts',(38.7738447669205,-2.45829132462492,5.26790933457678));
#66105=CARTESIAN_POINT('Ctrl Pts',(38.8744146768784,-4.67450050904083,3.45588049345234));
#66106=CARTESIAN_POINT('Ctrl Pts',(38.9508306935905,-5.49712786015583,1.44227304681289));
#66107=CARTESIAN_POINT('Ctrl Pts',(38.9937234069834,-5.5779477160896,0.258708067753872));
#66108=CARTESIAN_POINT('Ctrl Pts',(39.0030928170571,-5.57770250057755,0.00013896653026358));
#66109=CARTESIAN_POINT('Origin',(16.5082437683087,0.,0.));
#66110=CARTESIAN_POINT('',(36.1932437683088,-5.57766442098412,0.000135422462255629));
#66111=CARTESIAN_POINT('',(36.4630928170571,-5.57830649769973,2.26809192473663E-5));
#66112=CARTESIAN_POINT('',(16.5082437683087,-5.57784,5.11151866531329E-13));
#66113=CARTESIAN_POINT('Ctrl Pts',(36.1932437683088,-5.57766442098412,0.00013542246225573));
#66114=CARTESIAN_POINT('Ctrl Pts',(36.2169167506667,-5.57706728688419,-0.653184446091782));
#66115=CARTESIAN_POINT('Ctrl Pts',(36.2741130363439,-5.29976066215789,-2.2321640105613));
#66116=CARTESIAN_POINT('Ctrl Pts',(36.3648326253404,-3.84138542393408,-4.36323537688503));
#66117=CARTESIAN_POINT('Ctrl Pts',(36.4654025352982,-1.29312733691379,-5.66761736709884));
#66118=CARTESIAN_POINT('Ctrl Pts',(36.565972445256,1.56871301614697,-5.59760702463875));
#66119=CARTESIAN_POINT('Ctrl Pts',(36.6665423552138,4.05014181318524,-4.17018179728447));
#66120=CARTESIAN_POINT('Ctrl Pts',(36.7671122651716,5.54941470700435,-1.73149107390076));
#66121=CARTESIAN_POINT('Ctrl Pts',(36.8676821751295,5.70295931147022,1.12708474438672));
#66122=CARTESIAN_POINT('Ctrl Pts',(36.9682520850872,4.47354119217547,3.71234348238731));
#66123=CARTESIAN_POINT('Ctrl Pts',(37.068821995045,2.15929318473071,5.39736212160066));
#66124=CARTESIAN_POINT('Ctrl Pts',(37.1693919050028,-0.678581561229704,
5.77352509252997));
#66125=CARTESIAN_POINT('Ctrl Pts',(37.2699618149606,-3.35190086273439,4.74961319853676));
#66126=CARTESIAN_POINT('Ctrl Pts',(37.3679124360626,-5.16393173391408,2.63058883473529));
#66127=CARTESIAN_POINT('Ctrl Pts',(37.4323397538453,-5.57768855100025,0.852555361794227));
#66128=CARTESIAN_POINT('Ctrl Pts',(37.4632437683088,-5.57823681479003,-7.19583867583775E-5));
#66129=CARTESIAN_POINT('Ctrl Pts',(36.4630928170571,-5.57830649769973,2.26809192474704E-5));
#66130=CARTESIAN_POINT('Ctrl Pts',(36.4958307939877,-5.57809885394134,-0.903170003029449));
#66131=CARTESIAN_POINT('Ctrl Pts',(36.5620920742375,-5.12541758812386,-2.73142201137822));
#66132=CARTESIAN_POINT('Ctrl Pts',(36.6618766578068,-3.22139075996267,-4.83908116956871));
#66133=CARTESIAN_POINT('Ctrl Pts',(36.7624465677644,-0.5211943400678,-5.78985504602047));
#66134=CARTESIAN_POINT('Ctrl Pts',(36.8630164777224,2.30539125863451,-5.33659405788552));
#66135=CARTESIAN_POINT('Ctrl Pts',(36.9635863876801,4.57292146166484,-3.58921360460651));
#66136=CARTESIAN_POINT('Ctrl Pts',(37.064156297638,5.73152214674337,-0.97145194190844));
#66137=CARTESIAN_POINT('Ctrl Pts',(37.1647262075957,5.50023364509525,1.88188598044871));
#66138=CARTESIAN_POINT('Ctrl Pts',(37.2652961175536,3.93514321927045,4.27886817252847));
#66139=CARTESIAN_POINT('Ctrl Pts',(37.3658660275113,1.41578395025668,5.63822851614255));
#66140=CARTESIAN_POINT('Ctrl Pts',(37.4664359374691,-1.44690170794694,5.63032329814084));
#66141=CARTESIAN_POINT('Ctrl Pts',(37.5670058474269,-3.9587149475079,4.25706952708373));
#66142=CARTESIAN_POINT('Ctrl Pts',(37.6558914739562,-5.33025071134417,2.13096314978175));
#66143=CARTESIAN_POINT('Ctrl Pts',(37.7112537971663,-5.57709139671561,0.602634033284536));
#66144=CARTESIAN_POINT('Ctrl Pts',(37.7330928170571,-5.5775348825402,-0.000112846948039542));
#66145=CARTESIAN_POINT('Origin',(16.5082437683087,0.,0.));
#66146=CARTESIAN_POINT('',(34.9232437683088,-5.57756608151389,-0.000120065769840256));
#66147=CARTESIAN_POINT('',(35.1930928170571,-5.57744951564134,8.38323760708748E-5));
#66148=CARTESIAN_POINT('',(16.5082437683087,-5.57784,5.11151866531329E-13));
#66149=CARTESIAN_POINT('Ctrl Pts',(34.9232437683088,-5.57756608151389,-0.000120065769840146));
#66150=CARTESIAN_POINT('Ctrl Pts',(34.9344471408496,-5.57781006450218,-0.309323022954409));
#66151=CARTESIAN_POINT('Ctrl Pts',(34.9791738167096,-5.47688847173027,-1.54358125097877));
#66152=CARTESIAN_POINT('Ctrl Pts',(35.057423795889,-4.57871148724481,-3.58182440187771));
#66153=CARTESIAN_POINT('Ctrl Pts',(35.1579937058468,-2.31400597626052,-5.33286426520916));
#66154=CARTESIAN_POINT('Ctrl Pts',(35.2585636158045,0.511843992004246,-5.79068913490987));
#66155=CARTESIAN_POINT('Ctrl Pts',(35.3591335257624,3.21357223281796,-4.84427687418623));
#66156=CARTESIAN_POINT('Ctrl Pts',(35.4597034357202,5.13601197350847,-2.72313164156489));
#66157=CARTESIAN_POINT('Ctrl Pts',(35.560273345678,5.81297323184956,0.0583706699861391));
#66158=CARTESIAN_POINT('Ctrl Pts',(35.6608432556358,5.08029348544121,2.82571814431267));
#66159=CARTESIAN_POINT('Ctrl Pts',(35.7614131655936,3.11564694207568,4.9078314011026));
#66160=CARTESIAN_POINT('Ctrl Pts',(35.8619830755514,0.395458697295045,5.79979976792715));
#66161=CARTESIAN_POINT('Ctrl Pts',(35.9625529855092,-2.42062794115745,5.28532168366335));
#66162=CARTESIAN_POINT('Ctrl Pts',(36.063122895467,-4.64971438762522,3.48915764086767));
#66163=CARTESIAN_POINT('Ctrl Pts',(36.1400198230669,-5.4919606905701,1.46883814539051));
#66164=CARTESIAN_POINT('Ctrl Pts',(36.1833934473475,-5.57791288830659,0.271981626644002));
#66165=CARTESIAN_POINT('Ctrl Pts',(36.1932437683088,-5.57766442098412,0.00013542246225573));
#66166=CARTESIAN_POINT('Ctrl Pts',(35.1930928170571,-5.57744951564134,8.38323760707013E-5));
#66167=CARTESIAN_POINT('Ctrl Pts',(35.2133611841706,-5.57714996681278,-0.559338285009587));
#66168=CARTESIAN_POINT('Ctrl Pts',(35.2671528546033,-5.35512132667755,-2.04426121989497));
#66169=CARTESIAN_POINT('Ctrl Pts',(35.3544678283553,-4.05687069717986,-4.16363604802468));
#66170=CARTESIAN_POINT('Ctrl Pts',(35.4550377383131,-1.57775019122715,-5.59506651686378));
#66171=CARTESIAN_POINT('Ctrl Pts',(35.5556076482709,1.28397337792556,-5.66969817175709));
#66172=CARTESIAN_POINT('Ctrl Pts',(35.6561775582287,3.83433450821241,-4.36943290063812));
#66173=CARTESIAN_POINT('Ctrl Pts',(35.7567474681865,5.45487282096287,-2.00958391244754));
#66174=CARTESIAN_POINT('Ctrl Pts',(35.8573173781443,5.75260917034078,0.837587444604104));
#66175=CARTESIAN_POINT('Ctrl Pts',(35.9578872881021,4.65534274792201,3.48164456735854));
#66176=CARTESIAN_POINT('Ctrl Pts',(36.05845719806,2.4291597165847,5.28140587962803));
#66177=CARTESIAN_POINT('Ctrl Pts',(36.1590271080177,-0.386092454934063,
5.80043081247336));
#66178=CARTESIAN_POINT('Ctrl Pts',(36.2595970179756,-3.10771753849076,4.91285626647109));
#66179=CARTESIAN_POINT('Ctrl Pts',(36.3601669279333,-5.07572379417585,2.83391830497715));
#66180=CARTESIAN_POINT('Ctrl Pts',(36.4279988609605,-5.57291174024723,0.968210876530677));
#66181=CARTESIAN_POINT('Ctrl Pts',(36.4623074906685,-5.57831147870766,0.0216886821586606));
#66182=CARTESIAN_POINT('Ctrl Pts',(36.4630928170571,-5.57830649769973,2.26809192474704E-5));
#66183=CARTESIAN_POINT('Origin',(16.5082437683087,0.,0.));
#66184=CARTESIAN_POINT('',(33.6532437683088,-5.57829460971474,3.62717574107884E-5));
#66185=CARTESIAN_POINT('',(33.9230928170571,-5.57783438402505,-0.000142925532344573));
#66186=CARTESIAN_POINT('',(16.5082437683087,-5.57784,5.11151866531329E-13));
#66187=CARTESIAN_POINT('Ctrl Pts',(33.6532437683088,-5.57829460971474,3.62717574106273E-5));
#66188=CARTESIAN_POINT('Ctrl Pts',(33.6855008343517,-5.57797904703139,-0.889894308257694));
#66189=CARTESIAN_POINT('Ctrl Pts',(33.7512812037139,-5.13567938972669,-2.70499181735756));
#66190=CARTESIAN_POINT('Ctrl Pts',(33.8505848763954,-3.2558486083957,-4.81596457301359));
#66191=CARTESIAN_POINT('Ctrl Pts',(33.9511547863532,-0.562507314318525,
-5.78598742226877));
#66192=CARTESIAN_POINT('Ctrl Pts',(34.051724696311,2.26724151925849,-5.35291330236766));
#66193=CARTESIAN_POINT('Ctrl Pts',(34.1522946062688,4.54718623612184,-3.62176231458366));
#66194=CARTESIAN_POINT('Ctrl Pts',(34.2528645162266,5.72444220507391,-1.01233708322999));
#66195=CARTESIAN_POINT('Ctrl Pts',(34.3534344261844,5.5135258670596,1.84257901935812));
#66196=CARTESIAN_POINT('Ctrl Pts',(34.4540043361422,3.96558425248456,4.25067129589676));
#66197=CARTESIAN_POINT('Ctrl Pts',(34.5545742461,1.45599187037064,5.62797944228023));
#66198=CARTESIAN_POINT('Ctrl Pts',(34.6551441560578,-1.40667728694861,5.64050741863682));
#66199=CARTESIAN_POINT('Ctrl Pts',(34.7557140660156,-3.92822841309095,4.28521720148455));
#66200=CARTESIAN_POINT('Ctrl Pts',(34.8450806034326,-5.3224072856642,2.15750467293659));
#66201=CARTESIAN_POINT('Ctrl Pts',(34.9009238375303,-5.57708000614775,0.615889852290342));
#66202=CARTESIAN_POINT('Ctrl Pts',(34.9232437683088,-5.57756608151389,-0.000120065769840146));
#66203=CARTESIAN_POINT('Ctrl Pts',(33.9230928170571,-5.57783438402505,-0.000142925532344608));
#66204=CARTESIAN_POINT('Ctrl Pts',(33.9308915743534,-5.57805340367234,-0.215351841616216));
#66205=CARTESIAN_POINT('Ctrl Pts',(33.972213634969,-5.51331437958064,-1.35551481940617));
#66206=CARTESIAN_POINT('Ctrl Pts',(34.0470589989039,-4.75378622921922,-3.34597989846517));
#66207=CARTESIAN_POINT('Ctrl Pts',(34.1476289088617,-2.58041721203297,-5.20917575110413));
#66208=CARTESIAN_POINT('Ctrl Pts',(34.2481988188195,0.218700757774141,-5.80915096830823));
#66209=CARTESIAN_POINT('Ctrl Pts',(34.3487687287773,2.96478398208491,-5.00041207638131));
#66210=CARTESIAN_POINT('Ctrl Pts',(34.4493386387351,4.99190964291116,-2.97907756043006));
#66211=CARTESIAN_POINT('Ctrl Pts',(34.5499085486929,5.80850151251044,-0.235319300549913));
#66212=CARTESIAN_POINT('Ctrl Pts',(34.6504784586507,5.21653676545061,2.56550368714399));
#66213=CARTESIAN_POINT('Ctrl Pts',(34.7510483686085,3.35956634331347,4.74419423916461));
#66214=CARTESIAN_POINT('Ctrl Pts',(34.8516182785663,0.687903974933855,5.7724217721263));
#66215=CARTESIAN_POINT('Ctrl Pts',(34.952188188524,-2.15057451519974,5.40084199441352));
#66216=CARTESIAN_POINT('Ctrl Pts',(35.0527580984819,-4.46754053667362,3.71956268225518));
#66217=CARTESIAN_POINT('Ctrl Pts',(35.1330596413262,-5.45251987727794,1.65691221806805));
#66218=CARTESIAN_POINT('Ctrl Pts',(35.1798378808513,-5.57764541206412,0.365930002250153));
#66219=CARTESIAN_POINT('Ctrl Pts',(35.1930928170571,-5.57744951564134,8.38323760707013E-5));
#66220=CARTESIAN_POINT('Origin',(16.5082437683087,0.,0.));
#66221=CARTESIAN_POINT('',(32.3832437683088,-5.57742896989317,7.35428515294205E-5));
#66222=CARTESIAN_POINT('',(32.6530928170571,-5.57809874629883,0.00011458596757101));
#66223=CARTESIAN_POINT('',(16.5082437683087,-5.57784,5.11151866531329E-13));
#66224=CARTESIAN_POINT('Ctrl Pts',(32.3832437683088,-5.57742896989317,7.35428515291625E-5));
#66225=CARTESIAN_POINT('Ctrl Pts',(32.4030312245346,-5.57717363126457,-0.546080832034013));
#66226=CARTESIAN_POINT('Ctrl Pts',(32.4563419840797,-5.36250926464525,-2.01770966254631));
#66227=CARTESIAN_POINT('Ctrl Pts',(32.5431760469439,-4.08648613702948,-4.13457325260782));
#66228=CARTESIAN_POINT('Ctrl Pts',(32.6437459569018,-1.61764590787947,-5.58366247601294));
#66229=CARTESIAN_POINT('Ctrl Pts',(32.7443158668595,1.24347206141533,-5.67871835556173));
#66230=CARTESIAN_POINT('Ctrl Pts',(32.8448857768174,3.80304912623336,-4.39668992229039));
#66231=CARTESIAN_POINT('Ctrl Pts',(32.9454556867751,5.44039005171353,-2.04846796766039));
#66232=CARTESIAN_POINT('Ctrl Pts',(33.046025596733,5.75844107289692,0.796505705747263));
#66233=CARTESIAN_POINT('Ctrl Pts',(33.1465955066908,4.68007509093404,3.44832743116613));
#66234=CARTESIAN_POINT('Ctrl Pts',(33.2471654166486,2.46679492816254,5.26393272294638));
#66235=CARTESIAN_POINT('Ctrl Pts',(33.3477353266064,-0.344680881200578,
5.80303886075641));
#66236=CARTESIAN_POINT('Ctrl Pts',(33.4483052365642,-3.07257187358376,4.93491307025526));
#66237=CARTESIAN_POINT('Ctrl Pts',(33.548875146522,-5.05536683158087,2.87007510833188));
#66238=CARTESIAN_POINT('Ctrl Pts',(33.6171879904368,-5.56947823032715,0.99476209986866));
#66239=CARTESIAN_POINT('Ctrl Pts',(33.6519775310325,-5.57830699699238,0.034970114539885));
#66240=CARTESIAN_POINT('Ctrl Pts',(33.6532437683088,-5.57829460971474,3.62717574106273E-5));
#66241=CARTESIAN_POINT('Ctrl Pts',(32.6530928170571,-5.57809874629883,0.000114585967571079));
#66242=CARTESIAN_POINT('Ctrl Pts',(32.6819452678556,-5.57736761763102,-0.795968132793007));
#66243=CARTESIAN_POINT('Ctrl Pts',(32.7443210219733,-5.20504218182127,-2.51767136306138));
#66244=CARTESIAN_POINT('Ctrl Pts',(32.8402200794103,-3.49494881941665,-4.64536303680407));
#66245=CARTESIAN_POINT('Ctrl Pts',(32.940789989368,-0.854041693849599,-5.75018936898723));
#66246=CARTESIAN_POINT('Ctrl Pts',(33.0413598993259,1.99396980729241,-5.46059972911893));
#66247=CARTESIAN_POINT('Ctrl Pts',(33.1419298092837,4.35844534663238,-3.8468193555801));
#66248=CARTESIAN_POINT('Ctrl Pts',(33.2424997192414,5.66600164128877,-1.30018859976555));
#66249=CARTESIAN_POINT('Ctrl Pts',(33.3430696291993,5.59955741538933,1.56173677225253));
#66250=CARTESIAN_POINT('Ctrl Pts',(33.443639539157,4.17522533651758,4.04494232138717));
#66251=CARTESIAN_POINT('Ctrl Pts',(33.5442094491149,1.73840470769403,5.54725283958776));
#66252=CARTESIAN_POINT('Ctrl Pts',(33.6447793590727,-1.1199775662767,5.70435931942268));
#66253=CARTESIAN_POINT('Ctrl Pts',(33.7453492690304,-3.70676624453413,4.47816357477366));
#66254=CARTESIAN_POINT('Ctrl Pts',(33.838120421692,-5.263777944182,2.34531388575583));
#66255=CARTESIAN_POINT('Ctrl Pts',(33.8973682710342,-5.57711193802725,0.709733206778817));
#66256=CARTESIAN_POINT('Ctrl Pts',(33.9230928170571,-5.57783438402505,-0.000142925532344608));
#66257=CARTESIAN_POINT('Origin',(16.5082437683087,0.,0.));
#66258=CARTESIAN_POINT('',(31.1132437683088,-5.57787607033853,-0.000141715837242922));
#66259=CARTESIAN_POINT('',(31.3830928170571,-5.57736868831649,-9.6464866874979E-6));
#66260=CARTESIAN_POINT('',(16.5082437683087,-5.57784,5.11151866531329E-13));
#66261=CARTESIAN_POINT('Ctrl Pts',(31.1132437683088,-5.57787607033853,-0.000141715837243019));
#66262=CARTESIAN_POINT('Ctrl Pts',(31.1205616147174,-5.57808293770935,-0.202075414452116));
#66263=CARTESIAN_POINT('Ctrl Pts',(31.1614027644454,-5.51806033372383,-1.3289519298113));
#66264=CARTESIAN_POINT('Ctrl Pts',(31.2357672174925,-4.7775477306356,-3.31196355819516));
#66265=CARTESIAN_POINT('Ctrl Pts',(31.3363371274504,-2.61753301334895,-5.19062480375363));
#66266=CARTESIAN_POINT('Ctrl Pts',(31.4369070374081,0.177231206427325,-5.81056400264058));
#66267=CARTESIAN_POINT('Ctrl Pts',(31.537476947366,2.92901701121071,-5.02144643278732));
#66268=CARTESIAN_POINT('Ctrl Pts',(31.6380468573237,4.97051871215735,-3.01463242558821));
#66269=CARTESIAN_POINT('Ctrl Pts',(31.7386167672815,5.80667390417087,-0.276772650265986));
#66270=CARTESIAN_POINT('Ctrl Pts',(31.8391866772394,5.23471567297435,2.52820425449188));
#66271=CARTESIAN_POINT('Ctrl Pts',(31.9397565871971,3.39334339727493,4.72009380388618));
#66272=CARTESIAN_POINT('Ctrl Pts',(32.040326497155,0.729088268823663,5.76736466903021));
#66273=CARTESIAN_POINT('Ctrl Pts',(32.1408964071127,-2.11197013719727,5.4160545666473));
#66274=CARTESIAN_POINT('Ctrl Pts',(32.2414663170706,-4.44087760299231,3.75135589414753));
#66275=CARTESIAN_POINT('Ctrl Pts',(32.3222487708025,-5.44654131005962,1.68347805483491));
#66276=CARTESIAN_POINT('Ctrl Pts',(32.3695079212153,-5.57760621816194,0.379197210758078));
#66277=CARTESIAN_POINT('Ctrl Pts',(32.3832437683088,-5.57742896989317,7.35428515291625E-5));
#66278=CARTESIAN_POINT('Ctrl Pts',(31.3830928170571,-5.57736868831649,-9.64648668739382E-6));
#66279=CARTESIAN_POINT('Ctrl Pts',(31.3994756580384,-5.57739604835976,-0.452207087798499));
#66280=CARTESIAN_POINT('Ctrl Pts',(31.449381802339,-5.4118049609828,-1.82969150179622));
#66281=CARTESIAN_POINT('Ctrl Pts',(31.5328112499588,-4.29010873851205,-3.92288567330096));
#66282=CARTESIAN_POINT('Ctrl Pts',(31.6333811599166,-1.89761393322384,-5.49482723609051));
#66283=CARTESIAN_POINT('Ctrl Pts',(31.7339510698744,0.955050617350668,-5.73427792423296));
#66284=CARTESIAN_POINT('Ctrl Pts',(31.8345209798323,3.57611621535257,-4.58317115197979));
#66285=CARTESIAN_POINT('Ctrl Pts',(31.93509088979,5.32997670955485,-2.32064932069671));
#66286=CARTESIAN_POINT('Ctrl Pts',(32.0356607997479,5.79132243988692,0.504627973173819));
#66287=CARTESIAN_POINT('Ctrl Pts',(32.1362307097056,4.84827746388286,3.20753341794796));
#66288=CARTESIAN_POINT('Ctrl Pts',(32.2368006196635,2.72952937642347,5.13261477000649));
#66289=CARTESIAN_POINT('Ctrl Pts',(32.3373705296212,-0.051127235161469,
5.8130414586404));
#66290=CARTESIAN_POINT('Ctrl Pts',(32.4379404395791,-2.81938553623152,5.0838105975868));
#66291=CARTESIAN_POINT('Ctrl Pts',(32.5385103495368,-4.90394527177332,3.12176004290838));
#66292=CARTESIAN_POINT('Ctrl Pts',(32.6102278086962,-5.54243391615643,1.18275932950451));
#66293=CARTESIAN_POINT('Ctrl Pts',(32.6484219645363,-5.57821710692632,0.128990465513416));
#66294=CARTESIAN_POINT('Ctrl Pts',(32.6530928170571,-5.57809874629883,0.000114585967571079));
#66295=CARTESIAN_POINT('Origin',(16.5082437683087,0.,0.));
#66296=CARTESIAN_POINT('',(29.8432437683088,-5.5780605344387,0.000122021361445272));
#66297=CARTESIAN_POINT('',(30.1130928170571,-5.57815516189836,-0.00010078891834242));
#66298=CARTESIAN_POINT('',(16.5082437683087,-5.57784,5.11151866531329E-13));
#66299=CARTESIAN_POINT('Ctrl Pts',(29.8432437683088,-5.5780605344387,0.000122021361445238));
#66300=CARTESIAN_POINT('Ctrl Pts',(29.8716153082195,-5.57731124588235,-0.782707136893296));
#66301=CARTESIAN_POINT('Ctrl Pts',(29.9335101514496,-5.21438063601642,-2.491185998848));
#66302=CARTESIAN_POINT('Ctrl Pts',(30.0289282979989,-3.52801699702796,-4.62029879964445));
#66303=CARTESIAN_POINT('Ctrl Pts',(30.1294982079567,-0.895063067200426,
-5.74394699096779));
#66304=CARTESIAN_POINT('Ctrl Pts',(30.2300681179145,1.95494288592725,-5.47469298153573));
#66305=CARTESIAN_POINT('Ctrl Pts',(30.3306380278723,4.33087687208847,-3.87783063685398));
#66306=CARTESIAN_POINT('Ctrl Pts',(30.4312079378301,5.65657694491125,-1.34059770088297));
#66307=CARTESIAN_POINT('Ctrl Pts',(30.5317778477879,5.61056197793671,1.52172902352723));
#66308=CARTESIAN_POINT('Ctrl Pts',(30.6323477577457,4.20399056104516,4.01503776968005));
#66309=CARTESIAN_POINT('Ctrl Pts',(30.7329176677035,1.77795505201581,5.53470331294511));
#66310=CARTESIAN_POINT('Ctrl Pts',(30.8334875776613,-1.07923302661269,5.71220806725234));
#66311=CARTESIAN_POINT('Ctrl Pts',(30.9340574876192,-3.67470802532234,4.50450728248337));
#66312=CARTESIAN_POINT('Ctrl Pts',(31.0273095511682,-5.25505371512234,2.37182694926743));
#66313=CARTESIAN_POINT('Ctrl Pts',(31.0870383113982,-5.57713527124692,0.722989727807046));
#66314=CARTESIAN_POINT('Ctrl Pts',(31.1132437683088,-5.57787607033853,-0.000141715837243019));
#66315=CARTESIAN_POINT('Ctrl Pts',(30.1130928170571,-5.57815516189836,-0.000100788918342126));
#66316=CARTESIAN_POINT('Ctrl Pts',(30.1170060482213,-5.57824565243898,-0.108069590543255));
#66317=CARTESIAN_POINT('Ctrl Pts',(30.1544425827047,-5.54886883866117,-1.1409207127355));
#66318=CARTESIAN_POINT('Ctrl Pts',(30.2254024205074,-4.93873789291885,-3.06642022871864));
#66319=CARTESIAN_POINT('Ctrl Pts',(30.3259723304652,-2.87637223950989,-5.05178658830954));
#66320=CARTESIAN_POINT('Ctrl Pts',(30.426542240423,-0.116488794083507,-5.81209904895815));
#66321=CARTESIAN_POINT('Ctrl Pts',(30.5271121503808,2.67164308363124,-5.16298249345597));
#66322=CARTESIAN_POINT('Ctrl Pts',(30.6276820603386,4.81190381339239,-3.26184712773408));
#66323=CARTESIAN_POINT('Ctrl Pts',(30.7282519702964,5.78528201063068,-0.569716641428254));
#66324=CARTESIAN_POINT('Ctrl Pts',(30.8288218802542,5.35573430042772,2.26056963999551));
#66325=CARTESIAN_POINT('Ctrl Pts',(30.929391790212,3.62742563274069,4.54266972968354));
#66326=CARTESIAN_POINT('Ctrl Pts',(31.0299617001698,1.01946937170607,5.72317632038368));
#66327=CARTESIAN_POINT('Ctrl Pts',(31.1305316101276,-1.8357073343788,5.51581758006511));
#66328=CARTESIAN_POINT('Ctrl Pts',(31.2311015200854,-4.24572659210633,3.97087782475468));
#66329=CARTESIAN_POINT('Ctrl Pts',(31.3152885890619,-5.40128803627012,1.87153638998712));
#66330=CARTESIAN_POINT('Ctrl Pts',(31.3659523547191,-5.57734006301324,0.473099579255527));
#66331=CARTESIAN_POINT('Ctrl Pts',(31.3830928170571,-5.57736868831649,-9.64648668739382E-6));
#66332=CARTESIAN_POINT('Origin',(16.5082437683087,0.,0.));
#66333=CARTESIAN_POINT('',(28.5732437683088,-5.5773727299529,-2.18264568977285E-5));
#66334=CARTESIAN_POINT('',(28.8430928170571,-5.57776963474036,0.000142506048256413));
#66335=CARTESIAN_POINT('',(16.5082437683087,-5.57784,5.11151866531329E-13));
#66336=CARTESIAN_POINT('Ctrl Pts',(28.5732437683088,-5.5773727299529,-2.18264568977583E-5));
#66337=CARTESIAN_POINT('Ctrl Pts',(28.5891456984024,-5.57743287143306,-0.438944304786934));
#66338=CARTESIAN_POINT('Ctrl Pts',(28.6385709318153,-5.41834739991601,-1.80312865329392));
#66339=CARTESIAN_POINT('Ctrl Pts',(28.7215194685475,-4.31799983261996,-3.89216422762556));
#66340=CARTESIAN_POINT('Ctrl Pts',(28.8220893785053,-1.93678602348512,-5.48114265719722));
#66341=CARTESIAN_POINT('Ctrl Pts',(28.9226592884631,0.91409672910392,-5.74094871072331));
#66342=CARTESIAN_POINT('Ctrl Pts',(29.0232291984209,3.54331181176593,-4.60857964387231));
#66343=CARTESIAN_POINT('Ctrl Pts',(29.1237991083787,5.31327683025914,-2.35863398057979));
#66344=CARTESIAN_POINT('Ctrl Pts',(29.2243690183365,5.79477679123556,0.463278392623556));
#66345=CARTESIAN_POINT('Ctrl Pts',(29.3249389282943,4.87104836864741,3.17284615441902));
#66346=CARTESIAN_POINT('Ctrl Pts',(29.4255088382521,2.76609490980042,5.11300145504481));
#66347=CARTESIAN_POINT('Ctrl Pts',(29.5260787482099,-0.00963418353934693,
5.81325830424054));
#66348=CARTESIAN_POINT('Ctrl Pts',(29.6266486581677,-2.78302699566422,5.10380501887743));
#66349=CARTESIAN_POINT('Ctrl Pts',(29.7272185681255,-4.88153815704996,3.15668340993825));
#66350=CARTESIAN_POINT('Ctrl Pts',(29.7994169381725,-5.53822470938508,1.20931809855868));
#66351=CARTESIAN_POINT('Ctrl Pts',(29.8380920049003,-5.57819659181801,0.142269773132362));
#66352=CARTESIAN_POINT('Ctrl Pts',(29.8432437683088,-5.5780605344387,0.000122021361445238));
#66353=CARTESIAN_POINT('Ctrl Pts',(28.8430928170571,-5.57776963474036,0.000142506048256483));
#66354=CARTESIAN_POINT('Ctrl Pts',(28.8680597417234,-5.57708554036205,-0.688849856278956));
#66355=CARTESIAN_POINT('Ctrl Pts',(28.926549969709,-5.27729829006175,-2.30353694477276));
#66356=CARTESIAN_POINT('Ctrl Pts',(29.0185635010138,-3.75688664349095,-4.43619969591165));
#66357=CARTESIAN_POINT('Ctrl Pts',(29.1191334109716,-1.18404947371506,-5.69140508467306));
#66358=CARTESIAN_POINT('Ctrl Pts',(29.2197033209294,1.67591867417301,-5.56644963972599));
#66359=CARTESIAN_POINT('Ctrl Pts',(29.3202732308872,4.12947798625297,-4.09163494890484));
#66360=CARTESIAN_POINT('Ctrl Pts',(29.420843140845,5.58164244143966,-1.62460230517097));
#66361=CARTESIAN_POINT('Ctrl Pts',(29.5214130508028,5.68026340941513,1.2363949990626));
#66362=CARTESIAN_POINT('Ctrl Pts',(29.6219829607606,4.40142539034105,3.79756758034778));
#66363=CARTESIAN_POINT('Ctrl Pts',(29.7225528707184,2.05524550298248,5.43783329245368));
#66364=CARTESIAN_POINT('Ctrl Pts',(29.8231227806762,-0.789329649635071,
5.75942911218241));
#66365=CARTESIAN_POINT('Ctrl Pts',(29.923692690634,-3.44249304169372,4.68436833008867));
#66366=CARTESIAN_POINT('Ctrl Pts',(30.0203493694276,-5.19010136525037,2.5593841261018));
#66367=CARTESIAN_POINT('Ctrl Pts',(30.083482744902,-5.57747045115051,0.816861938937919));
#66368=CARTESIAN_POINT('Ctrl Pts',(30.1130928170571,-5.57815516189836,-0.000100788918342126));
#66369=CARTESIAN_POINT('Origin',(16.5082437683087,0.,0.));
#66370=CARTESIAN_POINT('',(27.3032437683088,-5.57818796811726,-9.07968746462347E-5));
#66371=CARTESIAN_POINT('',(27.5730928170571,-5.57748734871596,-9.87876261981935E-5));
#66372=CARTESIAN_POINT('',(16.5082437683087,-5.57784,5.11151866531329E-13));
#66373=CARTESIAN_POINT('Ctrl Pts',(27.3032437683088,-5.57818796811726,-9.07968746462033E-5));
#66374=CARTESIAN_POINT('Ctrl Pts',(27.3066760885853,-5.57826130241348,-0.0947893148921463));
#66375=CARTESIAN_POINT('Ctrl Pts',(27.343631712181,-5.55282928699094,-1.11436421216366));
#66376=CARTESIAN_POINT('Ctrl Pts',(27.4141106390961,-4.96049926954682,-3.03109088054774));
#66377=CARTESIAN_POINT('Ctrl Pts',(27.5146805490538,-2.91235710475748,-5.03112721203537));
#66378=CARTESIAN_POINT('Ctrl Pts',(27.6152504590117,-0.157970849104978,
-5.81111952554301));
#66379=CARTESIAN_POINT('Ctrl Pts',(27.7158203689695,2.63472320146966,-5.18192035648482));
#66380=CARTESIAN_POINT('Ctrl Pts',(27.8163902789273,4.78849914373318,-3.2961099617247));
#66381=CARTESIAN_POINT('Ctrl Pts',(27.9169601888851,5.7810681657188,-0.610995738632328));
#66382=CARTESIAN_POINT('Ctrl Pts',(28.0175300988429,5.37173313402688,2.22228442511572));
#66383=CARTESIAN_POINT('Ctrl Pts',(28.1181000088007,3.65975744147539,4.51666252877937));
#66384=CARTESIAN_POINT('Ctrl Pts',(28.2186699187585,1.06029371979028,5.71575385728667));
#66385=CARTESIAN_POINT('Ctrl Pts',(28.3192398287163,-1.79629031621274,5.52877979568679));
#66386=CARTESIAN_POINT('Ctrl Pts',(28.4198097386741,-4.21727549683238,4.00108139296507));
#66387=CARTESIAN_POINT('Ctrl Pts',(28.5044777185383,-5.39447844165815,1.89809661666281));
#66388=CARTESIAN_POINT('Ctrl Pts',(28.5556223950832,-5.57730608549767,0.486360440489903));
#66389=CARTESIAN_POINT('Ctrl Pts',(28.5732437683088,-5.5773727299529,-2.18264568977583E-5));
#66390=CARTESIAN_POINT('Ctrl Pts',(27.5730928170571,-5.57748734871596,-9.87876261983323E-5));
#66391=CARTESIAN_POINT('Ctrl Pts',(27.5855901319063,-5.57770694637395,-0.345027339152668));
#66392=CARTESIAN_POINT('Ctrl Pts',(27.6316107500747,-5.46173274549469,-1.61506032531023));
#66393=CARTESIAN_POINT('Ctrl Pts',(27.7111546715624,-4.50908274454013,-3.66909223063931));
#66394=CARTESIAN_POINT('Ctrl Pts',(27.8117245815202,-2.21116836378188,-5.3763183928277));
#66395=CARTESIAN_POINT('Ctrl Pts',(27.912294491478,0.622952441756332,-5.77979197284445));
#66396=CARTESIAN_POINT('Ctrl Pts',(28.0128644014358,3.30600781642397,-4.78167097485711));
#66397=CARTESIAN_POINT('Ctrl Pts',(28.1134343113936,5.18735914151516,-2.62399888166641));
#66398=CARTESIAN_POINT('Ctrl Pts',(28.2140042213514,5.8107803402164,0.169990681514914));
#66399=CARTESIAN_POINT('Ctrl Pts',(28.3145741313092,5.02509230850153,2.92275765076171));
#66400=CARTESIAN_POINT('Ctrl Pts',(28.415144041267,3.02082371771862,4.96675840569238));
#66401=CARTESIAN_POINT('Ctrl Pts',(28.5157139512248,0.284007975800641,5.80632452277075));
#66402=CARTESIAN_POINT('Ctrl Pts',(28.6162838611826,-2.5216794557668,5.23786194132788));
#66403=CARTESIAN_POINT('Ctrl Pts',(28.7168537711404,-4.71586179004478,3.39922234801476));
#66404=CARTESIAN_POINT('Ctrl Pts',(28.7924567564319,-5.50563811108249,1.39736289418203));
#66405=CARTESIAN_POINT('Ctrl Pts',(28.8345364384041,-5.57800407973563,0.236266082334538));
#66406=CARTESIAN_POINT('Ctrl Pts',(28.8430928170571,-5.57776963474036,0.000142506048256483));
#66407=CARTESIAN_POINT('Origin',(16.5082437683087,0.,0.));
#66408=CARTESIAN_POINT('',(26.0332437683088,-5.57772954743397,0.00014079117121212));
#66409=CARTESIAN_POINT('',(26.3030928170571,-5.57831427568592,-8.04374804677406E-7));
#66410=CARTESIAN_POINT('',(16.5082437683087,-5.57784,5.11151866531329E-13));
#66411=CARTESIAN_POINT('Ctrl Pts',(26.0332437683088,-5.57772954743397,0.000140791171212053));
#66412=CARTESIAN_POINT('Ctrl Pts',(26.0577297820874,-5.57707497798415,-0.675594212321096));
#66413=CARTESIAN_POINT('Ctrl Pts',(26.1157390991853,-5.28573910446548,-2.27701333570043));
#66414=CARTESIAN_POINT('Ctrl Pts',(26.2072717196025,-3.78845520303171,-4.40927115336947));
#66415=CARTESIAN_POINT('Ctrl Pts',(26.3078416295602,-1.22464285560959,-5.68280870745432));
#66416=CARTESIAN_POINT('Ctrl Pts',(26.408411539518,1.63614433009017,-5.57827004190617));
#66417=CARTESIAN_POINT('Ctrl Pts',(26.5089814494759,4.100167924183,-4.12100569313063));
#66418=CARTESIAN_POINT('Ctrl Pts',(26.6095513594336,5.56990432620359,-1.66440101125078));
#66419=CARTESIAN_POINT('Ctrl Pts',(26.7101212693915,5.6889437238532,1.19581948309323));
#66420=CARTESIAN_POINT('Ctrl Pts',(26.8106911793493,4.42841916567433,3.76605478218288));
#66421=CARTESIAN_POINT('Ctrl Pts',(26.911261089307,2.09400677192963,5.42302503852111));
#66422=CARTESIAN_POINT('Ctrl Pts',(27.0118309992649,-0.748200461426902,
5.76491639131348));
#66423=CARTESIAN_POINT('Ctrl Pts',(27.1124009092227,-3.40896972695984,4.70882048181766));
#66424=CARTESIAN_POINT('Ctrl Pts',(27.209538498904,-5.18047142072391,2.58585388687039));
#66425=CARTESIAN_POINT('Ctrl Pts',(27.273152785266,-5.57754504994926,0.830126452765981));
#66426=CARTESIAN_POINT('Ctrl Pts',(27.3032437683088,-5.57818796811726,-9.07968746462033E-5));
#66427=CARTESIAN_POINT('Ctrl Pts',(26.3030928170571,-5.57831427096578,-8.04366799073348E-7));
#66428=CARTESIAN_POINT('Ctrl Pts',(26.3031205220891,-5.57831427759844,-0.000765142388995596));
#66429=CARTESIAN_POINT('Ctrl Pts',(26.3366715304404,-5.57812799481241,-0.926384403945683));
#66430=CARTESIAN_POINT('Ctrl Pts',(26.403745842111,-5.10726891650053,-2.77666512359608));
#66431=CARTESIAN_POINT('Ctrl Pts',(26.5043157520687,-3.16276371564756,-4.87760091366961));
#66432=CARTESIAN_POINT('Ctrl Pts',(26.6048856620266,-0.451291036347756,
-5.79572268095701));
#66433=CARTESIAN_POINT('Ctrl Pts',(26.7054555719843,2.36961933078211,-5.30838668723663));
#66434=CARTESIAN_POINT('Ctrl Pts',(26.8060254819422,4.61589905003359,-3.53377149147286));
#66435=CARTESIAN_POINT('Ctrl Pts',(26.9065953918999,5.74282722315021,-0.902219750998773));
#66436=CARTESIAN_POINT('Ctrl Pts',(27.0071653018578,5.47712473824325,1.94811950243589));
#66437=CARTESIAN_POINT('Ctrl Pts',(27.1077352118156,3.88322421917838,4.32604145352698));
#66438=CARTESIAN_POINT('Ctrl Pts',(27.2083051217733,1.34764516975351,5.65490207611833));
#66439=CARTESIAN_POINT('Ctrl Pts',(27.3088750317312,-1.51473667324498,5.61245381315286));
#66440=CARTESIAN_POINT('Ctrl Pts',(27.409444941689,-4.00979617691032,4.20899033185902));
#66441=CARTESIAN_POINT('Ctrl Pts',(27.4975175367976,-5.3432668877154,2.08608595628941));
#66442=CARTESIAN_POINT('Ctrl Pts',(27.552066828587,-5.57711788872549,0.580222972283408));
#66443=CARTESIAN_POINT('Ctrl Pts',(27.5730928170571,-5.57748734871596,-9.87876261983323E-5));
#66444=CARTESIAN_POINT('Origin',(16.5082437683087,0.,0.));
#66445=CARTESIAN_POINT('',(24.7632437683088,-5.57751463566409,-0.000107372944178986));
#66446=CARTESIAN_POINT('',(25.0330928170571,-5.57749036758178,9.98147628876456E-5));
#66447=CARTESIAN_POINT('',(16.5082437683087,-5.57784,5.11151866531329E-13));
#66448=CARTESIAN_POINT('Ctrl Pts',(24.7632437683088,-5.57751463566409,-0.000107372944178757));
#66449=CARTESIAN_POINT('Ctrl Pts',(24.7752601722703,-5.57774565600241,-0.331758031377505));
#66450=CARTESIAN_POINT('Ctrl Pts',(24.820799879551,-5.46745062976281,-1.58849413899114));
#66451=CARTESIAN_POINT('Ctrl Pts',(24.899862890151,-4.53515675876486,-3.63681427938567));
#66452=CARTESIAN_POINT('Ctrl Pts',(25.0004328001089,-2.24948658571366,-5.36039877527861));
#66453=CARTESIAN_POINT('Ctrl Pts',(25.1010027100666,0.581682147950543,-5.78409118255149));
#66454=CARTESIAN_POINT('Ctrl Pts',(25.2015726200244,3.27179346146541,-4.80514645716718));
#66455=CARTESIAN_POINT('Ctrl Pts',(25.3021425299822,5.16849767702856,-2.66095785232772));
#66456=CARTESIAN_POINT('Ctrl Pts',(25.40271243994,5.81184565510331,0.128510741072388));
#66457=CARTESIAN_POINT('Ctrl Pts',(25.5032823498978,5.04582606481892,2.88681559038817));
#66458=CARTESIAN_POINT('Ctrl Pts',(25.6038522598556,3.05619799740772,4.94507014408847));
#66459=CARTESIAN_POINT('Ctrl Pts',(25.7044221698135,0.325444546488037,5.80414944470552));
#66460=CARTESIAN_POINT('Ctrl Pts',(25.8049920797712,-2.484228926803,5.25572750135977));
#66461=CARTESIAN_POINT('Ctrl Pts',(25.9055619897291,-4.69147902383981,3.43279616321523));
#66462=CARTESIAN_POINT('Ctrl Pts',(25.9816458859082,-5.50063843152049,1.42392723963565));
#66463=CARTESIAN_POINT('Ctrl Pts',(26.0242064787681,-5.57797113570129,0.249540833763626));
#66464=CARTESIAN_POINT('Ctrl Pts',(26.0332437683088,-5.57772954743397,0.000140791171212053));
#66465=CARTESIAN_POINT('Ctrl Pts',(25.0330928170571,-5.57749036758178,9.9814762887715E-5));
#66466=CARTESIAN_POINT('Ctrl Pts',(25.0541742155912,-5.57711581138055,-0.58175037250084));
#66467=CARTESIAN_POINT('Ctrl Pts',(25.1087789174447,-5.34238951116529,-2.08914466751173));
#66468=CARTESIAN_POINT('Ctrl Pts',(25.1969069226173,-4.00633332410426,-4.21228658690491));
#66469=CARTESIAN_POINT('Ctrl Pts',(25.2974768325751,-1.51012044812308,-5.61369764292733));
#66470=CARTESIAN_POINT('Ctrl Pts',(25.3980467425329,1.35229533657296,-5.65379185297181));
#66471=CARTESIAN_POINT('Ctrl Pts',(25.4986166524907,3.88678066624468,-4.32284640561678));
#66472=CARTESIAN_POINT('Ctrl Pts',(25.5991865624485,5.47872503020431,-1.94361442612985));
#66473=CARTESIAN_POINT('Ctrl Pts',(25.6997564724064,5.74208329058304,0.906942378574534));
#66474=CARTESIAN_POINT('Ctrl Pts',(25.8003263823641,4.61299129594534,3.53756643719661));
#66475=CARTESIAN_POINT('Ctrl Pts',(25.900896292322,2.3652528830361,5.31033368003713));
#66476=CARTESIAN_POINT('Ctrl Pts',(26.0014662022797,-0.456057317931881,
5.79534957675619));
#66477=CARTESIAN_POINT('Ctrl Pts',(26.1020361122375,-3.1667740118886,4.87499818991498));
#66478=CARTESIAN_POINT('Ctrl Pts',(26.2025783171634,-5.10901553723906,2.77304314538772));
#66479=CARTESIAN_POINT('Ctrl Pts',(26.2695972187698,-5.5783062520285,0.924089784394088));
#66480=CARTESIAN_POINT('Ctrl Pts',(26.3030928170571,-5.57831427096578,-8.04366799073348E-7));
#66481=CARTESIAN_POINT('Origin',(16.5082437683087,0.,0.));
#66482=CARTESIAN_POINT('',(23.4932437683088,-5.57831163277732,1.31347539625247E-5));
#66483=CARTESIAN_POINT('',(23.7630928170571,-5.57776496850477,-0.000142365144290002));
#66484=CARTESIAN_POINT('',(16.5082437683087,-5.57784,5.11151866531329E-13));
#66485=CARTESIAN_POINT('Ctrl Pts',(23.4932437683088,-5.57831163277732,1.31347539627179E-5));
#66486=CARTESIAN_POINT('Ctrl Pts',(23.5263138657724,-5.57818690513318,-0.912339814690282));
#66487=CARTESIAN_POINT('Ctrl Pts',(23.5929072665553,-5.11826294276396,-2.74967014419475));
#66488=CARTESIAN_POINT('Ctrl Pts',(23.6930239706574,-3.19749799998333,-4.85490179812288));
#66489=CARTESIAN_POINT('Ctrl Pts',(23.7935938806152,-0.492647672782865,
-5.79235385657815));
#66490=CARTESIAN_POINT('Ctrl Pts',(23.894163790573,2.33166929098219,-5.32516509103753));
#66491=CARTESIAN_POINT('Ctrl Pts',(23.9947337005308,4.59055845885185,-3.56662837497514));
#66492=CARTESIAN_POINT('Ctrl Pts',(24.0953036104886,5.73624115213431,-0.94318734823729));
#66493=CARTESIAN_POINT('Ctrl Pts',(24.1958735204464,5.49089030394512,1.90897579852541));
#66494=CARTESIAN_POINT('Ctrl Pts',(24.2964434304042,3.91400328376506,4.2982139574468));
#66495=CARTESIAN_POINT('Ctrl Pts',(24.397013340362,1.38797383655825,5.64513893171319));
#66496=CARTESIAN_POINT('Ctrl Pts',(24.4975832503198,-1.47463807120625,5.62312257453662));
#66497=CARTESIAN_POINT('Ctrl Pts',(24.5981531602776,-3.97965151611398,4.23750383358008));
#66498=CARTESIAN_POINT('Ctrl Pts',(24.6867066662739,-5.33560473957068,2.11263182982895));
#66499=CARTESIAN_POINT('Ctrl Pts',(24.741736868951,-5.57710115662481,0.593479307041815));
#66500=CARTESIAN_POINT('Ctrl Pts',(24.7632437683088,-5.57751463566409,-0.000107372944178757));
#66501=CARTESIAN_POINT('Ctrl Pts',(23.7630928170571,-5.57776496850477,-0.000142365144289967));
#66502=CARTESIAN_POINT('Ctrl Pts',(23.7717046057741,-5.57800034635737,-0.237795620494548));
#66503=CARTESIAN_POINT('Ctrl Pts',(23.8138396978104,-5.50506709041506,-1.40042358557772));
#66504=CARTESIAN_POINT('Ctrl Pts',(23.8894980931659,-4.71306465610696,-3.40309954914673));
#66505=CARTESIAN_POINT('Ctrl Pts',(23.9900680031237,-2.51737095653659,-5.23993401306099));
#66506=CARTESIAN_POINT('Ctrl Pts',(24.0906379130815,0.288783032968795,-5.80608898949342));
#66507=CARTESIAN_POINT('Ctrl Pts',(24.1912078230393,3.02490738557195,-4.9642723840216));
#66508=CARTESIAN_POINT('Ctrl Pts',(24.2917777329971,5.02749430110096,-2.91862399881259));
#66509=CARTESIAN_POINT('Ctrl Pts',(24.3923476429549,5.81091817642424,-0.165211806326761));
#66510=CARTESIAN_POINT('Ctrl Pts',(24.4929175529127,5.18519939616966,2.62826410697425));
#66511=CARTESIAN_POINT('Ctrl Pts',(24.5934874628705,3.30207422591229,4.78438823681912));
#66512=CARTESIAN_POINT('Ctrl Pts',(24.6940573728283,0.618198898391366,5.78030233777395));
#66513=CARTESIAN_POINT('Ctrl Pts',(24.7946272827861,-2.21558912982611,5.37449809766863));
#66514=CARTESIAN_POINT('Ctrl Pts',(24.895197192744,-4.51209870130343,3.66538269540076));
#66515=CARTESIAN_POINT('Ctrl Pts',(24.9746857041676,-5.46239669669542,1.61199939801417));
#66516=CARTESIAN_POINT('Ctrl Pts',(25.020650912272,-5.57771142467081,0.343498504248142));
#66517=CARTESIAN_POINT('Ctrl Pts',(25.0330928170571,-5.57749036758178,9.9814762887715E-5));
#66518=CARTESIAN_POINT('Origin',(16.5082437683087,0.,0.));
#66519=CARTESIAN_POINT('',(22.2232437683088,-5.57746529176104,9.05900862117445E-5));
#66520=CARTESIAN_POINT('',(22.4930928170571,-5.57815907267454,9.96846322134232E-5));
#66521=CARTESIAN_POINT('',(16.5082437683087,-5.57784,5.11151866531329E-13));
#66522=CARTESIAN_POINT('Ctrl Pts',(22.2232437683088,-5.57746529176104,9.05900862117892E-5));
#66523=CARTESIAN_POINT('Ctrl Pts',(22.2438442559552,-5.57713507809895,-0.568493695023154));
#66524=CARTESIAN_POINT('Ctrl Pts',(22.297968046921,-5.34995718351836,-2.06259671300443));
#66525=CARTESIAN_POINT('Ctrl Pts',(22.385615141206,-4.03629730435431,-4.18358327276709));
#66526=CARTESIAN_POINT('Ctrl Pts',(22.4861850511638,-1.5501508710191,-5.60277584830882));
#66527=CARTESIAN_POINT('Ctrl Pts',(22.5867549611216,1.31190581412394,-5.66330010366589));
#66528=CARTESIAN_POINT('Ctrl Pts',(22.6873248710794,3.85582646866807,-4.35047895901507));
#66529=CARTESIAN_POINT('Ctrl Pts',(22.7878947810372,5.46471252376619,-1.98267041182017));
#66530=CARTESIAN_POINT('Ctrl Pts',(22.888464690995,5.74841049603226,0.865934003501583));
#66531=CARTESIAN_POINT('Ctrl Pts',(22.9890346009528,4.63812387140712,3.50455016839501));
#66532=CARTESIAN_POINT('Ctrl Pts',(23.0896045109106,2.40309620059581,5.29331593426996));
#66533=CARTESIAN_POINT('Ctrl Pts',(23.1901744208684,-0.414680230205875,
5.79845714272258));
#66534=CARTESIAN_POINT('Ctrl Pts',(23.2907443308262,-3.13189706215126,4.89747748554319));
#66535=CARTESIAN_POINT('Ctrl Pts',(23.391314240784,-5.08963155255177,2.80886375400866));
#66536=CARTESIAN_POINT('Ctrl Pts',(23.4588140532782,-5.57522741043254,0.949874987164157));
#66537=CARTESIAN_POINT('Ctrl Pts',(23.4927905624531,-5.57831334209489,0.0125163848447095));
#66538=CARTESIAN_POINT('Ctrl Pts',(23.4932437683088,-5.57831163277732,1.31347539627179E-5));
#66539=CARTESIAN_POINT('Ctrl Pts',(22.4930928170571,-5.57815907267454,9.96846322134405E-5));
#66540=CARTESIAN_POINT('Ctrl Pts',(22.5227582992762,-5.57747866976091,-0.818390184172317));
#66541=CARTESIAN_POINT('Ctrl Pts',(22.5859470848146,-5.18899760582401,-2.56243426994159));
#66542=CARTESIAN_POINT('Ctrl Pts',(22.6826591736723,-3.43863942725612,-4.68719787115575));
#66543=CARTESIAN_POINT('Ctrl Pts',(22.7832290836301,-0.78459279653397,-5.7600763135287));
#66544=CARTESIAN_POINT('Ctrl Pts',(22.8837989935879,2.05971691194769,-5.4361412083098));
#66545=CARTESIAN_POINT('Ctrl Pts',(22.9843689035457,4.40454704234543,-3.79394653966204));
#66546=CARTESIAN_POINT('Ctrl Pts',(23.0849388135035,5.68127830653479,-1.2317231010842));
#66547=CARTESIAN_POINT('Ctrl Pts',(23.1855087234613,5.58030447199677,1.62919212920396));
#66548=CARTESIAN_POINT('Ctrl Pts',(23.2860786334191,4.12611160668567,4.09502967061549));
#66549=CARTESIAN_POINT('Ctrl Pts',(23.3866485433769,1.67134022862849,5.56782604202173));
#66550=CARTESIAN_POINT('Ctrl Pts',(23.4872184533347,-1.1887297161335,5.69042939118205));
#66551=CARTESIAN_POINT('Ctrl Pts',(23.5877883632925,-3.76053372802574,4.43310851146552));
#66552=CARTESIAN_POINT('Ctrl Pts',(23.6797464845333,-5.27827641947763,2.30048111746861));
#66553=CARTESIAN_POINT('Ctrl Pts',(23.7381813024548,-5.57708408570509,0.687322543190415));
#66554=CARTESIAN_POINT('Ctrl Pts',(23.7630928170571,-5.57776496850477,-0.000142365144289967));
#66555=CARTESIAN_POINT('Origin',(16.5082437683087,0.,0.));
#66556=CARTESIAN_POINT('',(20.9532437683088,-5.5778058049599,-0.000143089372731608));
#66557=CARTESIAN_POINT('',(21.2230928170571,-5.57736899471967,1.10549737200594E-5));
#66558=CARTESIAN_POINT('',(16.5082437683087,-5.57784,5.11151866531329E-13));
#66559=CARTESIAN_POINT('Ctrl Pts',(20.9532437683088,-5.5778058049599,-0.000143089372731907));
#66560=CARTESIAN_POINT('Ctrl Pts',(20.9613746461381,-5.57803218064351,-0.224520272604914));
#66561=CARTESIAN_POINT('Ctrl Pts',(21.0030288272867,-5.50997940288581,-1.37385969881095));
#66562=CARTESIAN_POINT('Ctrl Pts',(21.0782063117546,-4.7372348978758,-3.36937241192321));
#66563=CARTESIAN_POINT('Ctrl Pts',(21.1787762217124,-2.5547079071865,-5.22183228757078));
#66564=CARTESIAN_POINT('Ctrl Pts',(21.2793461316702,0.247333551781491,-5.80800232805862));
#66565=CARTESIAN_POINT('Ctrl Pts',(21.379916041628,2.98939683737892,-4.98573680395642));
#66566=CARTESIAN_POINT('Ctrl Pts',(21.4804859515858,5.0065339632579,-2.95443439662243));
#66567=CARTESIAN_POINT('Ctrl Pts',(21.5810558615436,5.80959091282129,-0.206684191439672));
#66568=CARTESIAN_POINT('Ctrl Pts',(21.6816257715014,5.20382706708468,2.59118675228346));
#66569=CARTESIAN_POINT('Ctrl Pts',(21.7821956814592,3.33613963718532,4.76069713912736));
#66570=CARTESIAN_POINT('Ctrl Pts',(21.882765591417,0.659441217112314,5.77574256788688));
#66571=CARTESIAN_POINT('Ctrl Pts',(21.9833355013748,-2.17717113044407,5.39017539585389));
#66572=CARTESIAN_POINT('Ctrl Pts',(22.0839054113326,-4.48582135303932,3.69749533034633));
#66573=CARTESIAN_POINT('Ctrl Pts',(22.1638748336439,-5.45658946829869,1.63856553019077));
#66574=CARTESIAN_POINT('Ctrl Pts',(22.210320952636,-5.57767243687145,0.356767093915296));
#66575=CARTESIAN_POINT('Ctrl Pts',(22.2232437683088,-5.57746529176104,9.05900862117892E-5));
#66576=CARTESIAN_POINT('Ctrl Pts',(21.2230928170571,-5.57736899471967,1.10549737201288E-5));
#66577=CARTESIAN_POINT('Ctrl Pts',(21.2402886894591,-5.57733608158979,-0.47462751888798));
#66578=CARTESIAN_POINT('Ctrl Pts',(21.2910078651803,-5.40050874890991,-1.87459669199057));
#66579=CARTESIAN_POINT('Ctrl Pts',(21.3752503442208,-4.24245948454918,-3.97436819079288));
#66580=CARTESIAN_POINT('Ctrl Pts',(21.4758202541787,-1.83117047488202,-5.51732541055725));
#66581=CARTESIAN_POINT('Ctrl Pts',(21.5763901641365,1.02417579862052,-5.72233596772863));
#66582=CARTESIAN_POINT('Ctrl Pts',(21.6769600740943,3.6311603225972,-4.53968497867921));
#66583=CARTESIAN_POINT('Ctrl Pts',(21.7775299840521,5.35759159415115,-2.25616429018983));
#66584=CARTESIAN_POINT('Ctrl Pts',(21.8780998940099,5.78481151609187,0.574474296499018));
#66585=CARTESIAN_POINT('Ctrl Pts',(21.9786698039677,4.809219625112,3.26580336081112));
#66586=CARTESIAN_POINT('Ctrl Pts',(22.0792397139255,2.66739611495663,5.16517792142356));
#66587=CARTESIAN_POINT('Ctrl Pts',(22.1798096238833,-0.121268656904642,
5.81200128242416));
#66588=CARTESIAN_POINT('Ctrl Pts',(22.2803795338411,-2.88052588385809,5.04941933557423));
#66589=CARTESIAN_POINT('Ctrl Pts',(22.3809494437989,-4.94125806361523,3.06235754653254));
#66590=CARTESIAN_POINT('Ctrl Pts',(22.4518538715375,-5.54933006834121,1.13786085343053));
#66591=CARTESIAN_POINT('Ctrl Pts',(22.4892349959569,-5.57824755506284,0.10653946750165));
#66592=CARTESIAN_POINT('Ctrl Pts',(22.4930928170571,-5.57815907267454,9.96846322134405E-5));
#66593=CARTESIAN_POINT('Origin',(16.5082437683087,0.,0.));
#66594=CARTESIAN_POINT('',(19.6832437683088,-5.57812419168581,0.000109767319341423));
#66595=CARTESIAN_POINT('',(19.9530928170571,-5.57809442763664,-0.000115493386879661));
#66596=CARTESIAN_POINT('',(16.5082437683087,-5.57784,5.11151866531329E-13));
#66597=CARTESIAN_POINT('Ctrl Pts',(19.6832437683088,-5.57812419168581,0.000109767319341463));
#66598=CARTESIAN_POINT('Ctrl Pts',(19.7124283396402,-5.57741063147403,-0.805125894194631));
#66599=CARTESIAN_POINT('Ctrl Pts',(19.775136214291,-5.19852697588659,-2.5359603525814));
#66600=CARTESIAN_POINT('Ctrl Pts',(19.8713673922609,-3.4720077142605,-4.66253371853033));
#66601=CARTESIAN_POINT('Ctrl Pts',(19.9719373022187,-0.825686473140719,
-5.75432978220954));
#66602=CARTESIAN_POINT('Ctrl Pts',(20.0725072121766,2.02086287490732,-5.45070416604466));
#66603=CARTESIAN_POINT('Ctrl Pts',(20.1730771221344,4.37735479309912,-3.82528833061492));
#66604=CARTESIAN_POINT('Ctrl Pts',(20.2736470320921,5.67234190241483,-1.27224293413637));
#66605=CARTESIAN_POINT('Ctrl Pts',(20.37421694205,5.59179100359806,1.58932005701102));
#66606=CARTESIAN_POINT('Ctrl Pts',(20.4747868520077,4.15523558961498,4.06547441574607));
#66607=CARTESIAN_POINT('Ctrl Pts',(20.5753567619656,1.71103912739439,5.55575467045122));
#66608=CARTESIAN_POINT('Ctrl Pts',(20.6759266719234,-1.14808285301524,5.69876922970695));
#66609=CARTESIAN_POINT('Ctrl Pts',(20.7764965818812,-3.72879572848776,4.45983714130576));
#66610=CARTESIAN_POINT('Ctrl Pts',(20.8689356140096,-5.26973851376936,2.32700126529614));
#66611=CARTESIAN_POINT('Ctrl Pts',(20.9278513428188,-5.57709884221868,0.700578410378731));
#66612=CARTESIAN_POINT('Ctrl Pts',(20.9532437683088,-5.5778058049599,-0.000143089372731907));
#66613=CARTESIAN_POINT('Ctrl Pts',(19.9530928170571,-5.57809442763664,-0.000115493386879852));
#66614=CARTESIAN_POINT('Ctrl Pts',(19.9578190796419,-5.57821483639134,-0.130520510715282));
#66615=CARTESIAN_POINT('Ctrl Pts',(19.9960686455461,-5.54195387079495,-1.18581934554418));
#66616=CARTESIAN_POINT('Ctrl Pts',(20.0678415147694,-4.90137626234256,-3.12579203238712));
#66617=CARTESIAN_POINT('Ctrl Pts',(20.1684114247273,-2.81520362818565,-5.08612754957154));
#66618=CARTESIAN_POINT('Ctrl Pts',(20.268981334685,-0.0463465410280725,
-5.81308154368905));
#66619=CARTESIAN_POINT('Ctrl Pts',(20.3695512446429,2.73374954418304,-5.13036825249749));
#66620=CARTESIAN_POINT('Ctrl Pts',(20.4701211546007,4.85091371732528,-3.20354508412377));
#66621=CARTESIAN_POINT('Ctrl Pts',(20.5706910645585,5.79173549027881,-0.499864986629304));
#66622=CARTESIAN_POINT('Ctrl Pts',(20.6712609745162,5.32806639229823,2.32503193781961));
#66623=CARTESIAN_POINT('Ctrl Pts',(20.7718308844741,3.57234578085699,4.58611061982589));
#66624=CARTESIAN_POINT('Ctrl Pts',(20.8724007944319,0.950334392674663,5.73506142385651));
#66625=CARTESIAN_POINT('Ctrl Pts',(20.9729707043897,-1.90213226762502,5.4932647697747));
#66626=CARTESIAN_POINT('Ctrl Pts',(21.0735406143475,-4.29333349045155,3.91935613764576));
#66627=CARTESIAN_POINT('Ctrl Pts',(21.1569146519033,-5.41256404288243,1.82663100194757));
#66628=CARTESIAN_POINT('Ctrl Pts',(21.2067653861398,-5.57740024564094,0.450679002736854));
#66629=CARTESIAN_POINT('Ctrl Pts',(21.2230928170571,-5.57736899471967,1.10549737201288E-5));
#66630=CARTESIAN_POINT('Origin',(55.8232233047034,0.,-1.80744194084639E-16));
#66631=CARTESIAN_POINT('',(56.,5.05,-6.18446633569413E-16));
#66632=CARTESIAN_POINT('Origin',(56.,0.,0.));
#66633=CARTESIAN_POINT('',(55.6464466094067,5.90355339059328,7.22976776338556E-16));
#66634=CARTESIAN_POINT('',(55.8232233047034,5.47677669529664,6.70711704953985E-16));
#66635=CARTESIAN_POINT('',(55.6464466094067,-5.90355339059328,-7.22976776338556E-16));
#66636=CARTESIAN_POINT('Origin',(55.6464466094067,0.,-3.61488388169278E-16));
#66637=CARTESIAN_POINT('Origin',(55.6464466094067,0.,-3.61488388169278E-16));
#66638=CARTESIAN_POINT('Origin',(55.6,0.,0.));
#66639=CARTESIAN_POINT('',(55.26731,-6.28269,-7.69407619853509E-16));
#66640=CARTESIAN_POINT('',(55.6,-5.95,-7.28664845492675E-16));
#66641=CARTESIAN_POINT('',(55.26731,3.34571636511773,-5.31774159209371));
#66642=CARTESIAN_POINT('Origin',(55.26731,0.,0.));
#66643=CARTESIAN_POINT('',(55.26731,6.25879749617516,-0.55033779021994));
#66644=CARTESIAN_POINT('Origin',(55.26731,0.,0.));
#66645=CARTESIAN_POINT('Origin',(55.26731,0.,0.));
#66646=CARTESIAN_POINT('Origin',(56.,0.,0.));
#66647=CARTESIAN_POINT('Origin',(-0.25,7.95,-6.));
#66648=CARTESIAN_POINT('',(-0.379994381348751,8.07999438134875,7.13596312065045));
#66649=CARTESIAN_POINT('',(0.,7.7,6.99070811863863));
#66650=CARTESIAN_POINT('Ctrl Pts',(-0.379994381348751,8.07999438134875,
7.13596312065045));
#66651=CARTESIAN_POINT('Ctrl Pts',(-0.188043578117705,7.88804357811771,
7.06333561964445));
#66652=CARTESIAN_POINT('Ctrl Pts',(-1.38777878078145E-16,7.7,6.99070811863862));
#66653=CARTESIAN_POINT('',(0.,7.7,-6.99070811863863));
#66654=CARTESIAN_POINT('',(0.,7.7,-6.));
#66655=CARTESIAN_POINT('',(-0.37999438134875,8.07999438134875,-7.13596312065045));
#66656=CARTESIAN_POINT('Ctrl Pts',(-1.38777878078145E-16,7.7,-6.99070811863862));
#66657=CARTESIAN_POINT('Ctrl Pts',(-0.188043578117704,7.8880435781177,-7.06333561964445));
#66658=CARTESIAN_POINT('Ctrl Pts',(-0.37999438134875,8.07999438134875,-7.13596312065045));
#66659=CARTESIAN_POINT('',(-0.5,8.2,-6.83212111192935));
#66660=CARTESIAN_POINT('',(-0.686724551909448,8.38672455190945,-6.3593535568152));
#66661=CARTESIAN_POINT('',(-0.5,8.2,6.83212111192935));
#66662=CARTESIAN_POINT('',(-0.5,8.2,-6.));
#66663=CARTESIAN_POINT('',(-2.49296364416094,10.1929636441609,1.78614006741046));
#66664=CARTESIAN_POINT('Origin',(0.,7.17,0.));
#66665=CARTESIAN_POINT('Origin',(0.,0.,0.));
#66666=CARTESIAN_POINT('',(0.,-7.17,-8.78071754988652E-16));
#66667=CARTESIAN_POINT('Origin',(0.,0.,0.));
#66668=CARTESIAN_POINT('Origin',(-3.3,8.02916838915042,7.26464935833121));
#66669=CARTESIAN_POINT('',(-6.,8.2,6.83212111192935));
#66670=CARTESIAN_POINT('',(-3.3,8.2,6.83212111192935));
#66671=CARTESIAN_POINT('',(-6.15556461521625,8.04443538478375,7.22599487971177));
#66672=CARTESIAN_POINT('',(-4.01298129963321,10.1870187003668,1.80119205984589));
#66673=CARTESIAN_POINT('',(-6.,7.85833677830084,7.69717760473307));
#66674=CARTESIAN_POINT('Ctrl Pts',(-6.15556461521625,8.04443538478375,7.22599487971177));
#66675=CARTESIAN_POINT('Ctrl Pts',(-6.08268462231632,7.95218239374537,7.45957006079633));
#66676=CARTESIAN_POINT('Ctrl Pts',(-6.,7.85833677830084,7.69717760473307));
#66677=CARTESIAN_POINT('',(-0.599999999999996,7.85833677830084,7.69717760473307));
#66678=CARTESIAN_POINT('',(-3.3,7.85833677830084,7.69717760473307));
#66679=CARTESIAN_POINT('Ctrl Pts',(-0.6,7.85833677830085,7.69717760473306));
#66680=CARTESIAN_POINT('Ctrl Pts',(-0.481638745218463,7.97028509154812,
7.41373587298517));
#66681=CARTESIAN_POINT('Ctrl Pts',(-0.37999438134875,8.07999438134875,7.13596312065045));
#66682=CARTESIAN_POINT('Origin',(-3.3,0.,0.));
#66683=CARTESIAN_POINT('',(-6.,7.85833677830084,-7.69717760473307));
#66684=CARTESIAN_POINT('Origin',(-6.,0.,0.));
#66685=CARTESIAN_POINT('',(-0.599999999999996,7.85833677830084,-7.69717760473307));
#66686=CARTESIAN_POINT('',(-3.3,7.85833677830084,-7.69717760473307));
#66687=CARTESIAN_POINT('Origin',(-0.599999999999996,0.,0.));
#66688=CARTESIAN_POINT('Origin',(-6.25,0.,0.));
#66689=CARTESIAN_POINT('',(-6.5,7.7,6.99070811863863));
#66690=CARTESIAN_POINT('Ctrl Pts',(-6.5,7.7,6.99070811863863));
#66691=CARTESIAN_POINT('Ctrl Pts',(-6.33063251438461,7.86936748561539,7.10651564020904));
#66692=CARTESIAN_POINT('Ctrl Pts',(-6.15556461521625,8.04443538478376,7.22599487971177));
#66693=CARTESIAN_POINT('',(-6.5,7.7,-6.99070811863863));
#66694=CARTESIAN_POINT('Origin',(-6.5,0.,0.));
#66695=CARTESIAN_POINT('',(-6.15556461521625,8.04443538478375,-7.22599487971178));
#66696=CARTESIAN_POINT('Ctrl Pts',(-6.15556461521625,8.04443538478375,-7.22599487971178));
#66697=CARTESIAN_POINT('Ctrl Pts',(-6.33063251438454,7.86936748561546,-7.1065156402091));
#66698=CARTESIAN_POINT('Ctrl Pts',(-6.5,7.7,-6.99070811863863));
#66699=CARTESIAN_POINT('Ctrl Pts',(-6.,7.85833677830084,-7.69717760473307));
#66700=CARTESIAN_POINT('Ctrl Pts',(-6.08268462231633,7.95218239374537,-7.45957006079634));
#66701=CARTESIAN_POINT('Ctrl Pts',(-6.15556461521625,8.04443538478375,-7.22599487971178));
#66702=CARTESIAN_POINT('Origin',(-6.25,7.95,-6.));
#66703=CARTESIAN_POINT('',(-6.,8.2,-6.83212111192935));
#66704=CARTESIAN_POINT('',(-6.,8.2,-6.));
#66705=CARTESIAN_POINT('',(-5.8192203918847,8.3807796081153,-6.37440554925063));
#66706=CARTESIAN_POINT('',(-6.5,7.7,-6.));
#66707=CARTESIAN_POINT('Origin',(0.,8.2,-12.));
#66708=CARTESIAN_POINT('',(-3.3,8.2,-6.83212111192935));
#66709=CARTESIAN_POINT('Origin',(-6.5,10.4,0.));
#66710=CARTESIAN_POINT('Origin',(-3.3,8.02916838915042,-7.26464935833121));
#66711=CARTESIAN_POINT('Ctrl Pts',(-0.37999438134875,8.07999438134875,-7.13596312065045));
#66712=CARTESIAN_POINT('Ctrl Pts',(-0.481638745218464,7.97028509154812,
-7.41373587298517));
#66713=CARTESIAN_POINT('Ctrl Pts',(-0.6,7.85833677830085,-7.69717760473306));
#66714=CARTESIAN_POINT('Origin',(-0.300000000000002,0.,0.));
#66715=CARTESIAN_POINT('Origin',(55.26731,1.21203632162606E-15,2.67744564496562E-16));
#66716=CARTESIAN_POINT('Ctrl Pts',(55.26731,-5.53879749490421,-0.66264931684701));
#66717=CARTESIAN_POINT('Ctrl Pts',(55.26731,-5.53639098513788,-0.70561892266728));
#66718=CARTESIAN_POINT('Ctrl Pts',(55.26731,-5.53347920854467,-0.748545142165827));
#66719=CARTESIAN_POINT('Ctrl Pts',(55.26731,-5.53006164828575,-0.79141917993666));
#66720=CARTESIAN_POINT('Ctrl Pts',(55.26731,-5.51741046348254,-0.950131048639964));
#66721=CARTESIAN_POINT('Ctrl Pts',(55.26731,-5.49783241559118,-1.10812730197615));
#66722=CARTESIAN_POINT('Ctrl Pts',(55.26731,-5.47155417770622,-1.26500836420001));
#66723=CARTESIAN_POINT('Ctrl Pts',(55.26731,-5.44498168391539,-1.42364613398091));
#66724=CARTESIAN_POINT('Ctrl Pts',(55.26731,-5.4115580176756,-1.58114430079878));
#66725=CARTESIAN_POINT('Ctrl Pts',(55.26731,-5.37146426041803,-1.73709118451399));
#66726=CARTESIAN_POINT('Ctrl Pts',(55.26731,-5.35511257576213,-1.80069196528392));
#66727=CARTESIAN_POINT('Ctrl Pts',(55.26731,-5.33765084923196,-1.86403467739513));
#66728=CARTESIAN_POINT('Ctrl Pts',(55.26731,-5.31908891537725,-1.927091041383));
#66729=CARTESIAN_POINT('Ctrl Pts',(55.26731,-5.31157503508314,-1.95261628969471));
#66730=CARTESIAN_POINT('Ctrl Pts',(55.26731,-5.30388243230773,-1.97808913032777));
#66731=CARTESIAN_POINT('Ctrl Pts',(55.26731,-5.29601425645973,-2.00350056357598));
#66732=CARTESIAN_POINT('Ctrl Pts',(55.26731,-5.24778551413657,-2.15926239323839));
#66733=CARTESIAN_POINT('Ctrl Pts',(55.26731,-5.19294007214862,-2.31280035724505));
#66734=CARTESIAN_POINT('Ctrl Pts',(55.26731,-5.13168699340163,-2.46369615505792));
#66735=CARTESIAN_POINT('Ctrl Pts',(55.26731,-5.07029795396065,-2.6149268894619));
#66736=CARTESIAN_POINT('Ctrl Pts',(55.26731,-5.00247261475932,-2.76350446256005));
#66737=CARTESIAN_POINT('Ctrl Pts',(55.26731,-4.92836992148161,-2.90899887332677));
#66738=CARTESIAN_POINT('Ctrl Pts',(55.26731,-4.90394573253089,-2.9569537157577));
#66739=CARTESIAN_POINT('Ctrl Pts',(55.26731,-4.87883919629439,-3.00457349651584));
#66740=CARTESIAN_POINT('Ctrl Pts',(55.26731,-4.85305483416844,-3.05184239250323));
#66741=CARTESIAN_POINT('Ctrl Pts',(55.26731,-4.83800368980644,-3.0794347360277));
#66742=CARTESIAN_POINT('Ctrl Pts',(55.26731,-4.82272157071552,-3.10690751352349));
#66743=CARTESIAN_POINT('Ctrl Pts',(55.26731,-4.80720928755211,-3.13425753405247));
#66744=CARTESIAN_POINT('Ctrl Pts',(55.26731,-4.79564225862179,-3.15465159696193));
#66745=CARTESIAN_POINT('Ctrl Pts',(55.26731,-4.78394939219416,-3.1749735513043));
#66746=CARTESIAN_POINT('Ctrl Pts',(55.26731,-4.7721359879562,-3.19521407307116));
#66747=CARTESIAN_POINT('Ctrl Pts',(55.26731,-4.72395212555498,-3.27776999819641));
#66748=CARTESIAN_POINT('Ctrl Pts',(55.26731,-4.67374052959922,-3.3590117700535));
#66749=CARTESIAN_POINT('Ctrl Pts',(55.26731,-4.6215443815017,-3.43885946673828));
#66750=CARTESIAN_POINT('Ctrl Pts',(55.26731,-4.5328034432177,-3.57461200369533));
#66751=CARTESIAN_POINT('Ctrl Pts',(55.26731,-4.43832903291709,-3.70633616772238));
#66752=CARTESIAN_POINT('Ctrl Pts',(55.26731,-4.33852183698003,-3.8338008634785));
#66753=CARTESIAN_POINT('Ctrl Pts',(55.26731,-4.23736781566362,-3.96298560241993));
#66754=CARTESIAN_POINT('Ctrl Pts',(55.26731,-4.13073572754274,-4.08779570010757));
#66755=CARTESIAN_POINT('Ctrl Pts',(55.26731,-4.01899373500795,-4.20796867396684));
#66756=CARTESIAN_POINT('Ctrl Pts',(55.26731,-3.909336498848,-4.32589959568748));
#66757=CARTESIAN_POINT('Ctrl Pts',(55.26731,-3.79475765651907,-4.43936521884963));
#66758=CARTESIAN_POINT('Ctrl Pts',(55.26731,-3.67556598183449,-4.54808950467785));
#66759=CARTESIAN_POINT('Ctrl Pts',(55.26731,-3.58617222582106,-4.62963271904902));
#66760=CARTESIAN_POINT('Ctrl Pts',(55.26731,-3.49418291445617,-4.70850841060584));
#66761=CARTESIAN_POINT('Ctrl Pts',(55.26731,-3.39971633932651,-4.7845873566953));
#66762=CARTESIAN_POINT('Ctrl Pts',(55.26731,-3.37842810366135,-4.80173190259724));
#66763=CARTESIAN_POINT('Ctrl Pts',(55.26731,-3.35701402694704,-4.81873437102781));
#66764=CARTESIAN_POINT('Ctrl Pts',(55.26731,-3.3354754008909,-4.83559319542517));
#66765=CARTESIAN_POINT('Ctrl Pts',(55.26731,-3.31814813154819,-4.84915568499034));
#66766=CARTESIAN_POINT('Ctrl Pts',(55.26731,-3.3007467856717,-4.8626200729148));
#66767=CARTESIAN_POINT('Ctrl Pts',(55.26731,-3.28327672842942,-4.87598236089846));
#66768=CARTESIAN_POINT('Ctrl Pts',(55.26731,-3.14959090197206,-4.97823437345244));
#66769=CARTESIAN_POINT('Ctrl Pts',(55.26731,-3.01180300905512,-5.07457437893082));
#66770=CARTESIAN_POINT('Ctrl Pts',(55.26731,-2.87031200820997,-5.1647462198623));
#66771=CARTESIAN_POINT('Ctrl Pts',(55.26731,-2.74730242599433,-5.24313990154057));
#66772=CARTESIAN_POINT('Ctrl Pts',(55.26731,-2.62149298241495,-5.31687137958735));
#66773=CARTESIAN_POINT('Ctrl Pts',(55.26731,-2.49312065219561,-5.38575260253262));
#66774=CARTESIAN_POINT('Ctrl Pts',(55.26731,-2.34617012834124,-5.46460239655165));
#66775=CARTESIAN_POINT('Ctrl Pts',(55.26731,-2.19586150139362,-5.53709781451365));
#66776=CARTESIAN_POINT('Ctrl Pts',(55.26731,-2.04264539888495,-5.60318412837367));
#66777=CARTESIAN_POINT('Ctrl Pts',(55.26731,-1.88854421239906,-5.66965220326634));
#66778=CARTESIAN_POINT('Ctrl Pts',(55.26731,-1.73150118930178,-5.72963719159267));
#66779=CARTESIAN_POINT('Ctrl Pts',(55.26731,-1.57194996293008,-5.78303699335734));
#66780=CARTESIAN_POINT('Ctrl Pts',(55.26731,-1.4929835329537,-5.80946607073076));
#66781=CARTESIAN_POINT('Ctrl Pts',(55.26731,-1.41340238971528,-5.83428134027811));
#66782=CARTESIAN_POINT('Ctrl Pts',(55.26731,-1.33325765941392,-5.85746592651278));
#66783=CARTESIAN_POINT('Ctrl Pts',(55.26731,-1.31267842894026,-5.86341916812661));
#66784=CARTESIAN_POINT('Ctrl Pts',(55.26731,-1.2920594397503,-5.86926559490217));
#66785=CARTESIAN_POINT('Ctrl Pts',(55.26731,-1.27141013285999,-5.87500251293336));
#66786=CARTESIAN_POINT('Ctrl Pts',(55.26731,-1.10752825083565,-5.92053319001446));
#66787=CARTESIAN_POINT('Ctrl Pts',(55.26731,-0.942046179526727,-5.95908657120551));
#66788=CARTESIAN_POINT('Ctrl Pts',(55.26731,-0.775444606041624,-5.99064537269145));
#66789=CARTESIAN_POINT('Ctrl Pts',(55.26731,-0.607515220055868,-6.0224556974388));
#66790=CARTESIAN_POINT('Ctrl Pts',(55.26731,-0.438447729379715,-6.04715977389526));
#66791=CARTESIAN_POINT('Ctrl Pts',(55.26731,-0.268707779413495,-6.0646939791095));
#66792=CARTESIAN_POINT('Ctrl Pts',(55.26731,-0.0990952702397115,-6.08221501963854));
#66793=CARTESIAN_POINT('Ctrl Pts',(55.26731,0.0711894188729789,-6.09257716755982));
#66794=CARTESIAN_POINT('Ctrl Pts',(55.26731,0.241697465736731,-6.09566772239982));
#66795=CARTESIAN_POINT('Ctrl Pts',(55.26731,0.291425473729497,-6.09656907068579));
#66796=CARTESIAN_POINT('Ctrl Pts',(55.26731,0.341172543128352,-6.0968515846414));
#66797=CARTESIAN_POINT('Ctrl Pts',(55.26731,0.390927654735083,-6.09651163725333));
#66798=CARTESIAN_POINT('Ctrl Pts',(55.26731,0.519364571915785,-6.09563410340571));
#66799=CARTESIAN_POINT('Ctrl Pts',(55.26731,0.647855132112174,-6.09060997358755));
#66800=CARTESIAN_POINT('Ctrl Pts',(55.26731,0.776220742198477,-6.08149242407852));
#66801=CARTESIAN_POINT('Ctrl Pts',(55.26731,0.832380696611235,-6.07750349616832));
#66802=CARTESIAN_POINT('Ctrl Pts',(55.26731,0.888516726202931,-6.07273084466002));
#66803=CARTESIAN_POINT('Ctrl Pts',(55.26731,0.94461377786397,-6.06717791703778));
#66804=CARTESIAN_POINT('Ctrl Pts',(55.26731,0.979456538284439,-6.06372890642056));
#66805=CARTESIAN_POINT('Ctrl Pts',(55.26731,1.01428425996497,-6.05997886518406));
#66806=CARTESIAN_POINT('Ctrl Pts',(55.26731,1.04909331400685,-6.05592850219243));
#66807=CARTESIAN_POINT('Ctrl Pts',(55.26731,1.07028621757498,-6.053462507219));
#66808=CARTESIAN_POINT('Ctrl Pts',(55.26731,1.09146790447692,-6.05088565499255));
#66809=CARTESIAN_POINT('Ctrl Pts',(55.26731,1.11262823854904,-6.04819950667145));
#66810=CARTESIAN_POINT('Ctrl Pts',(55.26731,1.28221027526524,-6.02667231803342));
#66811=CARTESIAN_POINT('Ctrl Pts',(55.26731,1.45059848057761,-5.99810910051797));
#66812=CARTESIAN_POINT('Ctrl Pts',(55.26731,1.61737767416904,-5.96273158735447));
#66813=CARTESIAN_POINT('Ctrl Pts',(55.26731,1.78721861570122,-5.92670461051541));
#66814=CARTESIAN_POINT('Ctrl Pts',(55.26731,1.95539160952368,-5.88361085063995));
#66815=CARTESIAN_POINT('Ctrl Pts',(55.26731,2.12146398918322,-5.83363090017481));
#66816=CARTESIAN_POINT('Ctrl Pts',(55.26731,2.28786991126281,-5.7835505691788));
#66817=CARTESIAN_POINT('Ctrl Pts',(55.26731,2.45216750385921,-5.72655622517196));
#66818=CARTESIAN_POINT('Ctrl Pts',(55.26731,2.61391653842935,-5.66277744479735));
#66819=CARTESIAN_POINT('Ctrl Pts',(55.26731,2.7740105837354,-5.59965123831338));
#66820=CARTESIAN_POINT('Ctrl Pts',(55.26731,2.93160864878227,-5.52987849972489));
#66821=CARTESIAN_POINT('Ctrl Pts',(55.26731,3.08626846857654,-5.45353667014268));
#66822=CARTESIAN_POINT('Ctrl Pts',(55.26731,3.17371866150044,-5.41037026962568));
#66823=CARTESIAN_POINT('Ctrl Pts',(55.26731,3.26022910922655,-5.36510275759276));
#66824=CARTESIAN_POINT('Ctrl Pts',(55.26731,3.34571636511758,-5.31774159209381));
#66825=CARTESIAN_POINT('Ctrl Pts',(55.26731,6.259054959814,-0.550339049542366));
#66826=CARTESIAN_POINT('Ctrl Pts',(55.26731,6.26062435353154,-0.501976787317531));
#66827=CARTESIAN_POINT('Ctrl Pts',(55.26731,6.26162468980508,-0.453612950749968));
#66828=CARTESIAN_POINT('Ctrl Pts',(55.26731,6.26205307910451,-0.405256685636834));
#66829=CARTESIAN_POINT('Ctrl Pts',(55.26731,6.26359989997391,-0.230652697762518));
#66830=CARTESIAN_POINT('Ctrl Pts',(55.26731,6.25769385372729,-0.0561469830970189));
#66831=CARTESIAN_POINT('Ctrl Pts',(55.26731,6.24446672156915,0.117807872010252));
#66832=CARTESIAN_POINT('Ctrl Pts',(55.26731,6.2312217581332,0.291997232776786));
#66833=CARTESIAN_POINT('Ctrl Pts',(55.26731,6.21063574375413,0.465634978729183));
#66834=CARTESIAN_POINT('Ctrl Pts',(55.26731,6.18279028992183,0.638254810814217));
#66835=CARTESIAN_POINT('Ctrl Pts',(55.26731,6.17518420463392,0.685406535226076));
#66836=CARTESIAN_POINT('Ctrl Pts',(55.26731,6.16703619046129,0.732482206629567));
#66837=CARTESIAN_POINT('Ctrl Pts',(55.26731,6.15834728588605,0.77947205650192));
#66838=CARTESIAN_POINT('Ctrl Pts',(55.26731,6.15200415638981,0.813775886192789));
#66839=CARTESIAN_POINT('Ctrl Pts',(55.26731,6.1453727600719,0.848033975717414));
#66840=CARTESIAN_POINT('Ctrl Pts',(55.26731,6.13845341352662,0.882242476691098));
#66841=CARTESIAN_POINT('Ctrl Pts',(55.26731,6.13310876166636,0.908665857449567));
#66842=CARTESIAN_POINT('Ctrl Pts',(55.26731,6.12759420574721,0.935050245759139));
#66843=CARTESIAN_POINT('Ctrl Pts',(55.26731,6.12191042011715,0.961393081297173));
#66844=CARTESIAN_POINT('Ctrl Pts',(55.26731,6.08539362493502,1.13063872011406));
#66845=CARTESIAN_POINT('Ctrl Pts',(55.26731,6.04189304342002,1.29818273238435));
#66846=CARTESIAN_POINT('Ctrl Pts',(55.26731,5.99151057004913,1.46357572936354));
#66847=CARTESIAN_POINT('Ctrl Pts',(55.26731,5.94147782389488,1.62782065979071));
#66848=CARTESIAN_POINT('Ctrl Pts',(55.26731,5.88465812170642,1.78994500032788));
#66849=CARTESIAN_POINT('Ctrl Pts',(55.26731,5.82110503590125,1.94948687666254));
#66850=CARTESIAN_POINT('Ctrl Pts',(55.26731,5.79867983920363,2.00578245874144));
#66851=CARTESIAN_POINT('Ctrl Pts',(55.26731,5.77541587560676,2.06175625579524));
#66852=CARTESIAN_POINT('Ctrl Pts',(55.26731,5.75131420661106,2.11738708461132));
#66853=CARTESIAN_POINT('Ctrl Pts',(55.26731,5.73724476762827,2.14986178799096));
#66854=CARTESIAN_POINT('Ctrl Pts',(55.26731,5.72288985275387,2.18221960906239));
#66855=CARTESIAN_POINT('Ctrl Pts',(55.26731,5.70824957074237,2.21445624811616));
#66856=CARTESIAN_POINT('Ctrl Pts',(55.26731,5.69864542930337,2.23560373972508));
#66857=CARTESIAN_POINT('Ctrl Pts',(55.26731,5.68891860432664,2.25669867882069));
#66858=CARTESIAN_POINT('Ctrl Pts',(55.26731,5.67907503084032,2.27772758874302));
#66859=CARTESIAN_POINT('Ctrl Pts',(55.26731,5.63447921087121,2.37299801897305));
#66860=CARTESIAN_POINT('Ctrl Pts',(55.26731,5.58745815531255,2.46697904036293));
#66861=CARTESIAN_POINT('Ctrl Pts',(55.26731,5.53803781346215,2.55957253982886));
#66862=CARTESIAN_POINT('Ctrl Pts',(55.26731,5.45804813929303,2.70944046010506));
#66863=CARTESIAN_POINT('Ctrl Pts',(55.26731,5.37177526959653,2.85567505990725));
#66864=CARTESIAN_POINT('Ctrl Pts',(55.26731,5.27955684762645,2.99796478200937));
#66865=CARTESIAN_POINT('Ctrl Pts',(55.26731,5.18687973109493,3.14096225339068));
#66866=CARTESIAN_POINT('Ctrl Pts',(55.26731,5.08819724887706,3.27997606150962));
#66867=CARTESIAN_POINT('Ctrl Pts',(55.26731,4.98381076759098,3.41465759654846));
#66868=CARTESIAN_POINT('Ctrl Pts',(55.26731,4.88303664984125,3.54467838758864));
#66869=CARTESIAN_POINT('Ctrl Pts',(55.26731,4.77694582819166,3.6706618191179));
#66870=CARTESIAN_POINT('Ctrl Pts',(55.26731,4.66578001467949,3.79225854630936));
#66871=CARTESIAN_POINT('Ctrl Pts',(55.26731,4.58240565454537,3.88345609170295));
#66872=CARTESIAN_POINT('Ctrl Pts',(55.26731,4.49617597963476,3.97218543802049));
#66873=CARTESIAN_POINT('Ctrl Pts',(55.26731,4.40718462220901,4.05828393055008));
#66874=CARTESIAN_POINT('Ctrl Pts',(55.26731,4.386430352664,4.07836353572824));
#66875=CARTESIAN_POINT('Ctrl Pts',(55.26731,4.36552584907783,4.09829998793731));
#66876=CARTESIAN_POINT('Ctrl Pts',(55.26731,4.34447225403319,4.118091110524));
#66877=CARTESIAN_POINT('Ctrl Pts',(55.26731,4.32939733162735,4.13226206976808));
#66878=CARTESIAN_POINT('Ctrl Pts',(55.26731,4.314246538133,4.14635792301651));
#66879=CARTESIAN_POINT('Ctrl Pts',(55.26731,4.29903007439866,4.16036906530759));
#66880=CARTESIAN_POINT('Ctrl Pts',(55.26731,4.17560888326235,4.2740138582724));
#66881=CARTESIAN_POINT('Ctrl Pts',(55.26731,4.04770434386886,4.3822455413649));
#66882=CARTESIAN_POINT('Ctrl Pts',(55.26731,3.91561946318572,4.48475177730016));
#66883=CARTESIAN_POINT('Ctrl Pts',(55.26731,3.79417535715088,4.57900009793888));
#66884=CARTESIAN_POINT('Ctrl Pts',(55.26731,3.66919656977907,4.66840821575284));
#66885=CARTESIAN_POINT('Ctrl Pts',(55.26731,3.54089521629959,4.75270229533564));
#66886=CARTESIAN_POINT('Ctrl Pts',(55.26731,3.40098928201791,4.84462059267715));
#66887=CARTESIAN_POINT('Ctrl Pts',(55.26731,3.2571322026833,4.93045873435785));
#66888=CARTESIAN_POINT('Ctrl Pts',(55.26731,3.10975766305844,5.01005242618096));
#66889=CARTESIAN_POINT('Ctrl Pts',(55.26731,2.96307989452868,5.08926980752361));
#66890=CARTESIAN_POINT('Ctrl Pts',(55.26731,2.81291710565447,5.16230182142269));
#66891=CARTESIAN_POINT('Ctrl Pts',(55.26731,2.65968537241045,5.22893643335111));
#66892=CARTESIAN_POINT('Ctrl Pts',(55.26731,2.5865649781927,5.26073369224521));
#66893=CARTESIAN_POINT('Ctrl Pts',(55.26731,2.51274565898121,5.29107345515416));
#66894=CARTESIAN_POINT('Ctrl Pts',(55.26731,2.43827244344798,5.31992845289072));
#66895=CARTESIAN_POINT('Ctrl Pts',(55.26731,2.41937185972979,5.32725157297495));
#66896=CARTESIAN_POINT('Ctrl Pts',(55.26731,2.40042679525609,5.33447993108298));
#66897=CARTESIAN_POINT('Ctrl Pts',(55.26731,2.38144583174371,5.34161011482402));
#66898=CARTESIAN_POINT('Ctrl Pts',(55.26731,2.22683096477766,5.39969106576447));
#66899=CARTESIAN_POINT('Ctrl Pts',(55.26731,2.07011540008946,5.45115874666631));
#66900=CARTESIAN_POINT('Ctrl Pts',(55.26731,1.911728292796,5.49589861617376));
#66901=CARTESIAN_POINT('Ctrl Pts',(55.26731,1.75351066848805,5.54059061154054));
#66902=CARTESIAN_POINT('Ctrl Pts',(55.26731,1.59362433851506,5.57856935937553));
#66903=CARTESIAN_POINT('Ctrl Pts',(55.26731,1.43248375220305,5.60967057749581));
#66904=CARTESIAN_POINT('Ctrl Pts',(55.26731,1.27339371223188,5.64037602636594));
#66905=CARTESIAN_POINT('Ctrl Pts',(55.26731,1.11308044188337,5.66437794116206));
#66906=CARTESIAN_POINT('Ctrl Pts',(55.26731,0.951940409530166,5.6814676859131));
#66907=CARTESIAN_POINT('Ctrl Pts',(55.26731,0.907459779355754,5.68618508980675));
#66908=CARTESIAN_POINT('Ctrl Pts',(55.26731,0.862916172292719,5.69037550710057));
#66909=CARTESIAN_POINT('Ctrl Pts',(55.26731,0.818318002073663,5.69403384682366));
#66910=CARTESIAN_POINT('Ctrl Pts',(55.26731,0.701153467936443,5.70364472698457));
#66911=CARTESIAN_POINT('Ctrl Pts',(55.26731,0.583612054961453,5.70958425773096));
#66912=CARTESIAN_POINT('Ctrl Pts',(55.26731,0.465862065703461,5.71186041381545));
#66913=CARTESIAN_POINT('Ctrl Pts',(55.26731,0.41434644540309,5.71285623210241));
#66914=CARTESIAN_POINT('Ctrl Pts',(55.26731,0.362790955096401,5.71315068969682));
#66915=CARTESIAN_POINT('Ctrl Pts',(55.26731,0.311209982030667,5.71274368078609));
#66916=CARTESIAN_POINT('Ctrl Pts',(55.26731,0.27708871341108,5.71247444080188));
#66917=CARTESIAN_POINT('Ctrl Pts',(55.26731,0.242956297684031,5.71189823375274));
#66918=CARTESIAN_POINT('Ctrl Pts',(55.26731,0.208816953097745,5.71101491794674));
#66919=CARTESIAN_POINT('Ctrl Pts',(55.26731,0.188374788502713,5.71048600073071));
#66920=CARTESIAN_POINT('Ctrl Pts',(55.26731,0.167930440883001,5.70984692698787));
#66921=CARTESIAN_POINT('Ctrl Pts',(55.26731,0.147498859806081,5.70909832637494));
#66922=CARTESIAN_POINT('Ctrl Pts',(55.26731,-0.0137838547239354,5.70318902652697));
#66923=CARTESIAN_POINT('Ctrl Pts',(55.26731,-0.174494943653233,5.69045414521296));
#66924=CARTESIAN_POINT('Ctrl Pts',(55.26731,-0.33421189439968,5.67101179972101));
#66925=CARTESIAN_POINT('Ctrl Pts',(55.26731,-0.494670179165839,5.65147921163383));
#66926=CARTESIAN_POINT('Ctrl Pts',(55.26731,-0.654125821445795,5.62517659128013));
#66927=CARTESIAN_POINT('Ctrl Pts',(55.26731,-0.81214282132803,5.59217212346982));
#66928=CARTESIAN_POINT('Ctrl Pts',(55.26731,-0.969071547367172,5.55939495967776));
#66929=CARTESIAN_POINT('Ctrl Pts',(55.26731,-1.12458207397616,5.52000770889059));
#66930=CARTESIAN_POINT('Ctrl Pts',(55.26731,-1.27822915468614,5.4740294698342));
#66931=CARTESIAN_POINT('Ctrl Pts',(55.26731,-1.42877972365552,5.42897784881958));
#66932=CARTESIAN_POINT('Ctrl Pts',(55.26731,-1.57754176552956,5.37759792723356));
#66933=CARTESIAN_POINT('Ctrl Pts',(55.26731,-1.72406969420736,5.31986579039788));
#66934=CARTESIAN_POINT('Ctrl Pts',(55.26731,-1.79587686650099,5.29157369936754));
#66935=CARTESIAN_POINT('Ctrl Pts',(55.26731,-1.86714703849359,5.26175546467072));
#66936=CARTESIAN_POINT('Ctrl Pts',(55.26731,-1.93782473268728,5.23040479991611));
#66937=CARTESIAN_POINT('Ctrl Pts',(18.4587229554446,-2.48002491540308,4.99617608622634));
#66938=CARTESIAN_POINT('Ctrl Pts',(18.4922462587639,-3.30865498737451,4.58485687155599));
#66939=CARTESIAN_POINT('Ctrl Pts',(18.5592928654024,-4.7565022034365,3.3424227331334));
#66940=CARTESIAN_POINT('Ctrl Pts',(18.6598627753602,-5.77493526257405,0.666469965513239));
#66941=CARTESIAN_POINT('Ctrl Pts',(18.760432685318,-5.39287434860188,-2.17036838028292));
#66942=CARTESIAN_POINT('Ctrl Pts',(18.8610025952758,-3.7030871350563,-4.48125359415228));
#66943=CARTESIAN_POINT('Ctrl Pts',(18.9615725052336,-1.1152833298924,-5.70525647060629));
#66944=CARTESIAN_POINT('Ctrl Pts',(19.0621424151914,1.74296490233074,-5.54583252750879));
#66945=CARTESIAN_POINT('Ctrl Pts',(19.1627123251492,4.17855117605108,-4.04150148361096));
#66946=CARTESIAN_POINT('Ctrl Pts',(19.263282235107,5.60083956100377,-1.55713407092352));
#66947=CARTESIAN_POINT('Ctrl Pts',(19.3638521450648,5.66493061750189,1.30484940988588));
#66948=CARTESIAN_POINT('Ctrl Pts',(19.4644220550226,4.35528013812923,3.85040169824184));
#66949=CARTESIAN_POINT('Ctrl Pts',(19.5649919649805,1.98947835131264,5.4622381255191));
#66950=CARTESIAN_POINT('Ctrl Pts',(19.6655618749382,-0.858770415672562,
5.74948485589373));
#66951=CARTESIAN_POINT('Ctrl Pts',(19.766131784896,-3.49876799771652,4.64248730288639));
#66952=CARTESIAN_POINT('Ctrl Pts',(19.8667016948538,-5.29031740242813,2.40969014364539));
#66953=CARTESIAN_POINT('Ctrl Pts',(19.9672716048116,-5.79896936542072,-0.407454580540862));
#66954=CARTESIAN_POINT('Ctrl Pts',(20.0678415147694,-4.90137626234256,-3.12579203238712));
#66955=CARTESIAN_POINT('Ctrl Pts',(20.1684114247273,-2.81520362818565,-5.08612754957154));
#66956=CARTESIAN_POINT('Ctrl Pts',(20.268981334685,-0.0463465410280725,
-5.81308154368905));
#66957=CARTESIAN_POINT('Ctrl Pts',(20.3695512446429,2.73374954418304,-5.13036825249749));
#66958=CARTESIAN_POINT('Ctrl Pts',(20.4701211546007,4.85091371732528,-3.20354508412377));
#66959=CARTESIAN_POINT('Ctrl Pts',(20.5706910645585,5.79173549027881,-0.499864986629304));
#66960=CARTESIAN_POINT('Ctrl Pts',(20.6712609745162,5.32806639229823,2.32503193781961));
#66961=CARTESIAN_POINT('Ctrl Pts',(20.7718308844741,3.57234578085699,4.58611061982589));
#66962=CARTESIAN_POINT('Ctrl Pts',(20.8724007944319,0.950334392674663,5.73506142385651));
#66963=CARTESIAN_POINT('Ctrl Pts',(20.9729707043897,-1.90213226762502,5.4932647697747));
#66964=CARTESIAN_POINT('Ctrl Pts',(21.0735406143475,-4.29333349045155,3.91935613764576));
#66965=CARTESIAN_POINT('Ctrl Pts',(21.1741105243052,-5.64340503766005,1.39500701610168));
#66966=CARTESIAN_POINT('Ctrl Pts',(21.2746804342631,-5.62495572124505,-1.46763010602068));
#66967=CARTESIAN_POINT('Ctrl Pts',(21.3752503442208,-4.24245948454918,-3.97436819079288));
#66968=CARTESIAN_POINT('Ctrl Pts',(21.4758202541787,-1.83117047488202,-5.51732541055725));
#66969=CARTESIAN_POINT('Ctrl Pts',(21.5763901641365,1.02417579862052,-5.72233596772863));
#66970=CARTESIAN_POINT('Ctrl Pts',(21.6769600740943,3.6311603225972,-4.53968497867921));
#66971=CARTESIAN_POINT('Ctrl Pts',(21.7775299840521,5.35759159415115,-2.25616429018983));
#66972=CARTESIAN_POINT('Ctrl Pts',(21.8780998940099,5.78481151609187,0.574474296499018));
#66973=CARTESIAN_POINT('Ctrl Pts',(21.9786698039677,4.809219625112,3.26580336081112));
#66974=CARTESIAN_POINT('Ctrl Pts',(22.0792397139255,2.66739611495663,5.16517792142356));
#66975=CARTESIAN_POINT('Ctrl Pts',(22.1798096238833,-0.121268656904642,
5.81200128242416));
#66976=CARTESIAN_POINT('Ctrl Pts',(22.2803795338411,-2.88052588385809,5.04941933557423));
#66977=CARTESIAN_POINT('Ctrl Pts',(22.3809494437989,-4.94125806361523,3.06235754653254));
#66978=CARTESIAN_POINT('Ctrl Pts',(22.4815193537567,-5.80373941652232,0.332676688621903));
#66979=CARTESIAN_POINT('Ctrl Pts',(22.5820892637145,-5.25881895694809,-2.4776779799019));
#66980=CARTESIAN_POINT('Ctrl Pts',(22.6826591736723,-3.43863942725612,-4.68719787115575));
#66981=CARTESIAN_POINT('Ctrl Pts',(22.7832290836301,-0.78459279653397,-5.7600763135287));
#66982=CARTESIAN_POINT('Ctrl Pts',(22.8837989935879,2.05971691194769,-5.4361412083098));
#66983=CARTESIAN_POINT('Ctrl Pts',(22.9843689035457,4.40454704234543,-3.79394653966204));
#66984=CARTESIAN_POINT('Ctrl Pts',(23.0849388135035,5.68127830653479,-1.2317231010842));
#66985=CARTESIAN_POINT('Ctrl Pts',(23.1855087234613,5.58030447199677,1.62919212920396));
#66986=CARTESIAN_POINT('Ctrl Pts',(23.2860786334191,4.12611160668567,4.09502967061549));
#66987=CARTESIAN_POINT('Ctrl Pts',(23.3866485433769,1.67134022862849,5.56782604202173));
#66988=CARTESIAN_POINT('Ctrl Pts',(23.4872184533347,-1.1887297161335,5.69042939118205));
#66989=CARTESIAN_POINT('Ctrl Pts',(23.5877883632925,-3.76053372802574,4.43310851146552));
#66990=CARTESIAN_POINT('Ctrl Pts',(23.6883582732503,-5.42041154804703,2.10076263386556));
#66991=CARTESIAN_POINT('Ctrl Pts',(23.7889281832081,-5.76584423371262,-0.741016374050092));
#66992=CARTESIAN_POINT('Ctrl Pts',(23.8894980931659,-4.71306465610696,-3.40309954914673));
#66993=CARTESIAN_POINT('Ctrl Pts',(23.9900680031237,-2.51737095653659,-5.23993401306099));
#66994=CARTESIAN_POINT('Ctrl Pts',(24.0906379130815,0.288783032968795,-5.80608898949342));
#66995=CARTESIAN_POINT('Ctrl Pts',(24.1912078230393,3.02490738557195,-4.9642723840216));
#66996=CARTESIAN_POINT('Ctrl Pts',(24.2917777329971,5.02749430110096,-2.91862399881259));
#66997=CARTESIAN_POINT('Ctrl Pts',(24.3923476429549,5.81091817642424,-0.165211806326761));
#66998=CARTESIAN_POINT('Ctrl Pts',(24.4929175529127,5.18519939616966,2.62826410697425));
#66999=CARTESIAN_POINT('Ctrl Pts',(24.5934874628705,3.30207422591229,4.78438823681912));
#67000=CARTESIAN_POINT('Ctrl Pts',(24.6940573728283,0.618198898391366,5.78030233777395));
#67001=CARTESIAN_POINT('Ctrl Pts',(24.7946272827861,-2.21558912982611,5.37449809766863));
#67002=CARTESIAN_POINT('Ctrl Pts',(24.895197192744,-4.51209870130343,3.66538269540076));
#67003=CARTESIAN_POINT('Ctrl Pts',(24.9957671027017,-5.71442822185861,1.06741514476474));
#67004=CARTESIAN_POINT('Ctrl Pts',(25.0963370126596,-5.53101381775679,-1.78939965961516));
#67005=CARTESIAN_POINT('Ctrl Pts',(25.1969069226173,-4.00633332410426,-4.21228658690491));
#67006=CARTESIAN_POINT('Ctrl Pts',(25.2974768325751,-1.51012044812308,-5.61369764292733));
#67007=CARTESIAN_POINT('Ctrl Pts',(25.3980467425329,1.35229533657296,-5.65379185297181));
#67008=CARTESIAN_POINT('Ctrl Pts',(25.4986166524907,3.88678066624468,-4.32284640561678));
#67009=CARTESIAN_POINT('Ctrl Pts',(25.5991865624485,5.47872503020431,-1.94361442612985));
#67010=CARTESIAN_POINT('Ctrl Pts',(25.6997564724064,5.74208329058304,0.906942378574534));
#67011=CARTESIAN_POINT('Ctrl Pts',(25.8003263823641,4.61299129594534,3.53756643719661));
#67012=CARTESIAN_POINT('Ctrl Pts',(25.900896292322,2.3652528830361,5.31033368003713));
#67013=CARTESIAN_POINT('Ctrl Pts',(26.0014662022797,-0.456057317931881,
5.79534957675619));
#67014=CARTESIAN_POINT('Ctrl Pts',(26.1020361122375,-3.1667740118886,4.87499818991498));
#67015=CARTESIAN_POINT('Ctrl Pts',(26.2026060221954,-5.10955073401222,2.77246393855764));
#67016=CARTESIAN_POINT('Ctrl Pts',(26.3031759321531,-5.81326580158569,-0.00239043128346468));
#67017=CARTESIAN_POINT('Ctrl Pts',(26.403745842111,-5.10726891650053,-2.77666512359608));
#67018=CARTESIAN_POINT('Ctrl Pts',(26.5043157520687,-3.16276371564756,-4.87760091366961));
#67019=CARTESIAN_POINT('Ctrl Pts',(26.6048856620266,-0.451291036347756,
-5.79572268095701));
#67020=CARTESIAN_POINT('Ctrl Pts',(26.7054555719843,2.36961933078211,-5.30838668723663));
#67021=CARTESIAN_POINT('Ctrl Pts',(26.8060254819422,4.61589905003359,-3.53377149147286));
#67022=CARTESIAN_POINT('Ctrl Pts',(26.9065953918999,5.74282722315021,-0.902219750998773));
#67023=CARTESIAN_POINT('Ctrl Pts',(27.0071653018578,5.47712473824325,1.94811950243589));
#67024=CARTESIAN_POINT('Ctrl Pts',(27.1077352118156,3.88322421917838,4.32604145352698));
#67025=CARTESIAN_POINT('Ctrl Pts',(27.2083051217733,1.34764516975351,5.65490207611833));
#67026=CARTESIAN_POINT('Ctrl Pts',(27.3088750317312,-1.51473667324498,5.61245381315286));
#67027=CARTESIAN_POINT('Ctrl Pts',(27.409444941689,-4.00979617691032,4.20899033185902));
#67028=CARTESIAN_POINT('Ctrl Pts',(27.5100148516468,-5.53248355942245,1.78485031830896));
#67029=CARTESIAN_POINT('Ctrl Pts',(27.6105847616046,-5.71354844129516,-1.07211436098069));
#67030=CARTESIAN_POINT('Ctrl Pts',(27.7111546715624,-4.50908274454013,-3.66909223063931));
#67031=CARTESIAN_POINT('Ctrl Pts',(27.8117245815202,-2.21116836378188,-5.3763183928277));
#67032=CARTESIAN_POINT('Ctrl Pts',(27.912294491478,0.622952441756332,-5.77979197284445));
#67033=CARTESIAN_POINT('Ctrl Pts',(28.0128644014358,3.30600781642397,-4.78167097485711));
#67034=CARTESIAN_POINT('Ctrl Pts',(28.1134343113936,5.18735914151516,-2.62399888166641));
#67035=CARTESIAN_POINT('Ctrl Pts',(28.2140042213514,5.8107803402164,0.169990681514914));
#67036=CARTESIAN_POINT('Ctrl Pts',(28.3145741313092,5.02509230850153,2.92275765076171));
#67037=CARTESIAN_POINT('Ctrl Pts',(28.415144041267,3.02082371771862,4.96675840569238));
#67038=CARTESIAN_POINT('Ctrl Pts',(28.5157139512248,0.284007975800641,5.80632452277075));
#67039=CARTESIAN_POINT('Ctrl Pts',(28.6162838611826,-2.5216794557668,5.23786194132788));
#67040=CARTESIAN_POINT('Ctrl Pts',(28.7168537711404,-4.71586179004478,3.39922234801476));
#67041=CARTESIAN_POINT('Ctrl Pts',(28.8174236810982,-5.76645169978597,0.736274261456154));
#67042=CARTESIAN_POINT('Ctrl Pts',(28.917993591056,-5.41868203625607,-2.10521969969957));
#67043=CARTESIAN_POINT('Ctrl Pts',(29.0185635010138,-3.75688664349095,-4.43619969591165));
#67044=CARTESIAN_POINT('Ctrl Pts',(29.1191334109716,-1.18404947371506,-5.69140508467306));
#67045=CARTESIAN_POINT('Ctrl Pts',(29.2197033209294,1.67591867417301,-5.56644963972599));
#67046=CARTESIAN_POINT('Ctrl Pts',(29.3202732308872,4.12947798625297,-4.09163494890484));
#67047=CARTESIAN_POINT('Ctrl Pts',(29.420843140845,5.58164244143966,-1.62460230517097));
#67048=CARTESIAN_POINT('Ctrl Pts',(29.5214130508028,5.68026340941513,1.2363949990626));
#67049=CARTESIAN_POINT('Ctrl Pts',(29.6219829607606,4.40142539034105,3.79756758034778));
#67050=CARTESIAN_POINT('Ctrl Pts',(29.7225528707184,2.05524550298248,5.43783329245368));
#67051=CARTESIAN_POINT('Ctrl Pts',(29.8231227806762,-0.789329649635071,
5.75942911218241));
#67052=CARTESIAN_POINT('Ctrl Pts',(29.923692690634,-3.44249304169372,4.68436833008867));
#67053=CARTESIAN_POINT('Ctrl Pts',(30.0242626005918,-5.26085483453837,2.47335226038701));
#67054=CARTESIAN_POINT('Ctrl Pts',(30.1248325105496,-5.80346385870219,-0.337449603325932));
#67055=CARTESIAN_POINT('Ctrl Pts',(30.2254024205074,-4.93873789291885,-3.06642022871864));
#67056=CARTESIAN_POINT('Ctrl Pts',(30.3259723304652,-2.87637223950989,-5.05178658830954));
#67057=CARTESIAN_POINT('Ctrl Pts',(30.426542240423,-0.116488794083507,-5.81209904895815));
#67058=CARTESIAN_POINT('Ctrl Pts',(30.5271121503808,2.67164308363124,-5.16298249345597));
#67059=CARTESIAN_POINT('Ctrl Pts',(30.6276820603386,4.81190381339239,-3.26184712773408));
#67060=CARTESIAN_POINT('Ctrl Pts',(30.7282519702964,5.78528201063068,-0.569716641428254));
#67061=CARTESIAN_POINT('Ctrl Pts',(30.8288218802542,5.35573430042772,2.26056963999551));
#67062=CARTESIAN_POINT('Ctrl Pts',(30.929391790212,3.62742563274069,4.54266972968354));
#67063=CARTESIAN_POINT('Ctrl Pts',(31.0299617001698,1.01946937170607,5.72317632038368));
#67064=CARTESIAN_POINT('Ctrl Pts',(31.1305316101276,-1.8357073343788,5.51581758006511));
#67065=CARTESIAN_POINT('Ctrl Pts',(31.2311015200854,-4.24572659210633,3.97087782475468));
#67066=CARTESIAN_POINT('Ctrl Pts',(31.3316714300432,-5.62616080609128,1.46300361518679));
#67067=CARTESIAN_POINT('Ctrl Pts',(31.4322413400011,-5.64225586775969,-1.39964771166842));
#67068=CARTESIAN_POINT('Ctrl Pts',(31.5328112499588,-4.29010873851205,-3.92288567330096));
#67069=CARTESIAN_POINT('Ctrl Pts',(31.6333811599166,-1.89761393322384,-5.49482723609051));
#67070=CARTESIAN_POINT('Ctrl Pts',(31.7339510698744,0.955050617350668,-5.73427792423296));
#67071=CARTESIAN_POINT('Ctrl Pts',(31.8345209798323,3.57611621535257,-4.58317115197979));
#67072=CARTESIAN_POINT('Ctrl Pts',(31.93509088979,5.32997670955485,-2.32064932069671));
#67073=CARTESIAN_POINT('Ctrl Pts',(32.0356607997479,5.79132243988692,0.504627973173819));
#67074=CARTESIAN_POINT('Ctrl Pts',(32.1362307097056,4.84827746388286,3.20753341794796));
#67075=CARTESIAN_POINT('Ctrl Pts',(32.2368006196635,2.72952937642347,5.13261477000649));
#67076=CARTESIAN_POINT('Ctrl Pts',(32.3373705296212,-0.051127235161469,
5.8130414586404));
#67077=CARTESIAN_POINT('Ctrl Pts',(32.4379404395791,-2.81938553623152,5.0838105975868));
#67078=CARTESIAN_POINT('Ctrl Pts',(32.5385103495368,-4.90394527177332,3.12176004290838));
#67079=CARTESIAN_POINT('Ctrl Pts',(32.6390802594946,-5.79930250036685,0.402685365125275));
#67080=CARTESIAN_POINT('Ctrl Pts',(32.7396501694525,-5.28833386482735,-2.41404016705763));
#67081=CARTESIAN_POINT('Ctrl Pts',(32.8402200794103,-3.49494881941665,-4.64536303680407));
#67082=CARTESIAN_POINT('Ctrl Pts',(32.940789989368,-0.854041693849599,-5.75018936898723));
#67083=CARTESIAN_POINT('Ctrl Pts',(33.0413598993259,1.99396980729241,-5.46059972911893));
#67084=CARTESIAN_POINT('Ctrl Pts',(33.1419298092837,4.35844534663238,-3.8468193555801));
#67085=CARTESIAN_POINT('Ctrl Pts',(33.2424997192414,5.66600164128877,-1.30018859976555));
#67086=CARTESIAN_POINT('Ctrl Pts',(33.3430696291993,5.59955741538933,1.56173677225253));
#67087=CARTESIAN_POINT('Ctrl Pts',(33.443639539157,4.17522533651758,4.04494232138717));
#67088=CARTESIAN_POINT('Ctrl Pts',(33.5442094491149,1.73840470769403,5.54725283958776));
#67089=CARTESIAN_POINT('Ctrl Pts',(33.6447793590727,-1.1199775662767,5.70435931942268));
#67090=CARTESIAN_POINT('Ctrl Pts',(33.7453492690304,-3.70676624453413,4.47816357477366));
#67091=CARTESIAN_POINT('Ctrl Pts',(33.8459191789883,-5.39466729938273,2.16601701817368));
#67092=CARTESIAN_POINT('Ctrl Pts',(33.9464890889461,-5.77436617801534,-0.67138680076386));
#67093=CARTESIAN_POINT('Ctrl Pts',(34.0470589989039,-4.75378622921922,-3.34597989846517));
#67094=CARTESIAN_POINT('Ctrl Pts',(34.1476289088617,-2.58041721203297,-5.20917575110413));
#67095=CARTESIAN_POINT('Ctrl Pts',(34.2481988188195,0.218700757774141,-5.80915096830823));
#67096=CARTESIAN_POINT('Ctrl Pts',(34.3487687287773,2.96478398208491,-5.00041207638131));
#67097=CARTESIAN_POINT('Ctrl Pts',(34.4493386387351,4.99190964291116,-2.97907756043006));
#67098=CARTESIAN_POINT('Ctrl Pts',(34.5499085486929,5.80850151251044,-0.235319300549913));
#67099=CARTESIAN_POINT('Ctrl Pts',(34.6504784586507,5.21653676545061,2.56550368714399));
#67100=CARTESIAN_POINT('Ctrl Pts',(34.7510483686085,3.35956634331347,4.74419423916461));
#67101=CARTESIAN_POINT('Ctrl Pts',(34.8516182785663,0.687903974933855,5.7724217721263));
#67102=CARTESIAN_POINT('Ctrl Pts',(34.952188188524,-2.15057451519974,5.40084199441352));
#67103=CARTESIAN_POINT('Ctrl Pts',(35.0527580984819,-4.46754053667362,3.71956268225518));
#67104=CARTESIAN_POINT('Ctrl Pts',(35.1533280084396,-5.70113182379116,1.13629262155616));
#67105=CARTESIAN_POINT('Ctrl Pts',(35.2538979183975,-5.55220355133712,-1.72252742171694));
#67106=CARTESIAN_POINT('Ctrl Pts',(35.3544678283553,-4.05687069717986,-4.16363604802468));
#67107=CARTESIAN_POINT('Ctrl Pts',(35.4550377383131,-1.57775019122715,-5.59506651686378));
#67108=CARTESIAN_POINT('Ctrl Pts',(35.5556076482709,1.28397337792556,-5.66969817175709));
#67109=CARTESIAN_POINT('Ctrl Pts',(35.6561775582287,3.83433450821241,-4.36943290063812));
#67110=CARTESIAN_POINT('Ctrl Pts',(35.7567474681865,5.45487282096287,-2.00958391244754));
#67111=CARTESIAN_POINT('Ctrl Pts',(35.8573173781443,5.75260917034078,0.837587444604104));
#67112=CARTESIAN_POINT('Ctrl Pts',(35.9578872881021,4.65534274792201,3.48164456735854));
#67113=CARTESIAN_POINT('Ctrl Pts',(36.05845719806,2.4291597165847,5.28140587962803));
#67114=CARTESIAN_POINT('Ctrl Pts',(36.1590271080177,-0.386092454934063,
5.80043081247336));
#67115=CARTESIAN_POINT('Ctrl Pts',(36.2595970179756,-3.10771753849076,4.91285626647109));
#67116=CARTESIAN_POINT('Ctrl Pts',(36.3601669279333,-5.07572379417585,2.83391830497715));
#67117=CARTESIAN_POINT('Ctrl Pts',(36.4607368378912,-5.81287139910188,0.0677575940443941));
#67118=CARTESIAN_POINT('Ctrl Pts',(36.5613067478488,-5.14040269363212,-2.71483427511641));
#67119=CARTESIAN_POINT('Ctrl Pts',(36.6618766578068,-3.22139075996267,-4.83908116956871));
#67120=CARTESIAN_POINT('Ctrl Pts',(36.7624465677644,-0.5211943400678,-5.78985504602047));
#67121=CARTESIAN_POINT('Ctrl Pts',(36.8630164777224,2.30539125863451,-5.33659405788552));
#67122=CARTESIAN_POINT('Ctrl Pts',(36.9635863876801,4.57292146166484,-3.58921360460651));
#67123=CARTESIAN_POINT('Ctrl Pts',(37.064156297638,5.73152214674337,-0.97145194190844));
#67124=CARTESIAN_POINT('Ctrl Pts',(37.1647262075957,5.50023364509525,1.88188598044871));
#67125=CARTESIAN_POINT('Ctrl Pts',(37.2652961175536,3.93514321927045,4.27886817252847));
#67126=CARTESIAN_POINT('Ctrl Pts',(37.3658660275113,1.41578395025668,5.63822851614255));
#67127=CARTESIAN_POINT('Ctrl Pts',(37.4664359374691,-1.44690170794694,5.63032329814084));
#67128=CARTESIAN_POINT('Ctrl Pts',(37.5670058474269,-3.9587149475079,4.25706952708373));
#67129=CARTESIAN_POINT('Ctrl Pts',(37.6675757573847,-5.51054322007353,1.85148006031634));
#67130=CARTESIAN_POINT('Ctrl Pts',(37.7681456673425,-5.72606950540495,-1.00309172727058));
#67131=CARTESIAN_POINT('Ctrl Pts',(37.8687155773003,-4.55302886484057,-3.61441463448453));
#67132=CARTESIAN_POINT('Ctrl Pts',(37.9692854872581,-2.27588264393015,-5.34924510422778));
#67133=CARTESIAN_POINT('Ctrl Pts',(38.0698553972159,0.553163158988311,-5.78688824097939));
#67134=CARTESIAN_POINT('Ctrl Pts',(38.1704253071738,3.24806737203082,-4.82121596081281));
#67135=CARTESIAN_POINT('Ctrl Pts',(38.2709952171315,5.15531804338536,-2.6864029603901));
#67136=CARTESIAN_POINT('Ctrl Pts',(38.3715651270894,5.81240852706456,0.0998604453944716));
#67137=CARTESIAN_POINT('Ctrl Pts',(38.4721350370471,5.0599949464186,2.86190777913362));
#67138=CARTESIAN_POINT('Ctrl Pts',(38.572704947005,3.08053694705489,4.92994494004518));
#67139=CARTESIAN_POINT('Ctrl Pts',(38.6732748569627,0.354051389844875,5.80247469683378));
#67140=CARTESIAN_POINT('Ctrl Pts',(38.7738447669205,-2.45829132462492,5.26790933457678));
#67141=CARTESIAN_POINT('Ctrl Pts',(38.8744146768784,-4.67450050904083,3.45588049345234));
#67142=CARTESIAN_POINT('Ctrl Pts',(38.9749845868361,-5.75714734395841,0.80580360758677));
#67143=CARTESIAN_POINT('Ctrl Pts',(39.075554496794,-5.44369090388365,-2.03967995945972));
#67144=CARTESIAN_POINT('Ctrl Pts',(39.1761244067517,-3.81014410570237,-4.39054289215228));
#67145=CARTESIAN_POINT('Ctrl Pts',(39.2766943167096,-1.25264064176956,-5.67670295300313));
#67146=CARTESIAN_POINT('Ctrl Pts',(39.3772642266673,1.60862709948338,-5.58626743441943));
#67147=CARTESIAN_POINT('Ctrl Pts',(39.4778341366252,4.07980415386393,-4.14116687180823));
#67148=CARTESIAN_POINT('Ctrl Pts',(39.578404046583,5.5616322129449,-1.69183690761873));
#67149=CARTESIAN_POINT('Ctrl Pts',(39.6789739565408,5.69476924799924,1.16776205028657));
#67150=CARTESIAN_POINT('Ctrl Pts',(39.7795438664986,4.44692964263445,3.74417971624045));
#67151=CARTESIAN_POINT('Ctrl Pts',(39.8801137764563,2.12071342697536,5.41263702410329));
#67152=CARTESIAN_POINT('Ctrl Pts',(39.9806836864142,-0.719773969154297,
5.76853451297425));
#67153=CARTESIAN_POINT('Ctrl Pts',(40.081253596372,-3.38571679736614,4.72556734816892));
#67154=CARTESIAN_POINT('Ctrl Pts',(40.1818235063298,-5.23062621673878,2.5366541693365));
#67155=CARTESIAN_POINT('Ctrl Pts',(40.2823934162876,-5.80711328122534,-0.267395461935357));
#67156=CARTESIAN_POINT('Ctrl Pts',(40.3829633262454,-4.9753803739444,-3.00660192386958));
#67157=CARTESIAN_POINT('Ctrl Pts',(40.4835332362031,-2.93712200893205,-5.01671000743458));
#67158=CARTESIAN_POINT('Ctrl Pts',(40.584103146161,-0.186614085112543,-5.81027023272455));
#67159=CARTESIAN_POINT('Ctrl Pts',(40.6846730561188,2.609147593704,-5.19484492822605));
#67160=CARTESIAN_POINT('Ctrl Pts',(40.7852429660765,4.7721932270764,-3.31967420050424));
#67161=CARTESIAN_POINT('Ctrl Pts',(40.8858128760344,5.77798611092356,-0.639485336830895));
#67162=CARTESIAN_POINT('Ctrl Pts',(40.9863827859921,5.38262233672791,2.19577817053662));
#67163=CARTESIAN_POINT('Ctrl Pts',(41.08695269595,3.6819772793914,4.49856736173782));
#67164=CARTESIAN_POINT('Ctrl Pts',(41.1875226059078,1.08845590135412,5.7104578402134));
#67165=CARTESIAN_POINT('Ctrl Pts',(41.2880925158656,-1.76901509578748,5.53756720816311));
#67166=CARTESIAN_POINT('Ctrl Pts',(41.3886624258233,-4.19750145501954,4.02182129502992));
#67167=CARTESIAN_POINT('Ctrl Pts',(41.4892323357812,-5.608097324739,1.53078717995108));
#67168=CARTESIAN_POINT('Ctrl Pts',(41.589802245739,-5.65873442082026,-1.33146150852038));
#67169=CARTESIAN_POINT('Ctrl Pts',(41.6903721556968,-4.33713329105347,-3.87083192733591));
#67170=CARTESIAN_POINT('Ctrl Pts',(41.7909420656546,-1.96378107173494,-5.4715289358956));
#67171=CARTESIAN_POINT('Ctrl Pts',(41.8915119756124,0.88578636700025,-5.74538488754965));
#67172=CARTESIAN_POINT('Ctrl Pts',(41.9920818855702,3.52055137424819,-4.62598994976497));
#67173=CARTESIAN_POINT('Ctrl Pts',(42.0926517955281,5.30158570383253,-2.38479643134711));
#67174=CARTESIAN_POINT('Ctrl Pts',(42.1932217054858,5.7969900639945,0.434708168771271));
#67175=CARTESIAN_POINT('Ctrl Pts',(42.2937916154436,4.88662932385308,3.14879641217187));
#67176=CARTESIAN_POINT('Ctrl Pts',(42.3943615254014,2.79126517922797,5.09930423619505));
#67177=CARTESIAN_POINT('Ctrl Pts',(42.4949314353592,0.0190216314411856,
5.81323517256825));
#67178=CARTESIAN_POINT('Ctrl Pts',(42.595501345317,-2.75783464559572,5.11746158379321));
#67179=CARTESIAN_POINT('Ctrl Pts',(42.6960712552748,-4.86591839509884,3.18070796620598));
#67180=CARTESIAN_POINT('Ctrl Pts',(42.7966411652326,-5.79402112251256,0.472635404858439));
#67181=CARTESIAN_POINT('Ctrl Pts',(42.8972110751905,-5.31707871537652,-2.35005083530915));
#67182=CARTESIAN_POINT('Ctrl Pts',(42.9977809851481,-3.55074929685554,-4.60285177090544));
#67183=CARTESIAN_POINT('Ctrl Pts',(43.0983508951061,-0.923366230433899,
-5.73946511432395));
#67184=CARTESIAN_POINT('Ctrl Pts',(43.1989208050638,1.92793235200782,-5.48426310821507));
#67185=CARTESIAN_POINT('Ctrl Pts',(43.2994907150216,4.31170899870712,-3.89913201937502));
#67186=CARTESIAN_POINT('Ctrl Pts',(43.4000606249794,5.64989992486267,-1.36846477232117));
#67187=CARTESIAN_POINT('Ctrl Pts',(43.5006305349373,5.61799498283493,1.49405400400684));
#67188=CARTESIAN_POINT('Ctrl Pts',(43.601200444895,4.22373109360091,3.99426597048771));
#67189=CARTESIAN_POINT('Ctrl Pts',(43.7017703548528,1.80521605007753,5.52587187750403));
#67190=CARTESIAN_POINT('Ctrl Pts',(43.8023402648106,-1.05106233160792,5.71745861105458));
#67191=CARTESIAN_POINT('Ctrl Pts',(43.9029101747684,-3.65245900266303,4.52256655317676));
#67192=CARTESIAN_POINT('Ctrl Pts',(44.0034800847262,-5.36813750971383,2.23095599930855));
#67193=CARTESIAN_POINT('Ctrl Pts',(44.104049994684,-5.78204729170571,-0.601659463921077));
#67194=CARTESIAN_POINT('Ctrl Pts',(44.2046199046419,-4.79381558281113,-3.28837302507556));
#67195=CARTESIAN_POINT('Ctrl Pts',(44.3051898145996,-2.64308772173875,-5.17765895837504));
#67196=CARTESIAN_POINT('Ctrl Pts',(44.4057597245574,0.148586636609559,-5.81136705134586));
#67197=CARTESIAN_POINT('Ctrl Pts',(44.5063296345153,2.90422886348763,-5.03582363695677));
#67198=CARTESIAN_POINT('Ctrl Pts',(44.606899544473,4.95559809101348,-3.03909732558712));
#67199=CARTESIAN_POINT('Ctrl Pts',(44.7074694544309,5.80523904738957,-0.305392528904701));
#67200=CARTESIAN_POINT('Ctrl Pts',(44.8080393643886,5.24711453208993,2.50236969314653));
#67201=CARTESIAN_POINT('Ctrl Pts',(44.9086092743465,3.41656925962507,4.70330941872129));
#67202=CARTESIAN_POINT('Ctrl Pts',(45.0091791843043,0.757508882781974,5.76370065899971));
#67203=CARTESIAN_POINT('Ctrl Pts',(45.109749094262,-2.08524674605032,5.42639945102955));
#67204=CARTESIAN_POINT('Ctrl Pts',(45.2103190042198,-4.42233183400564,3.77320104738504));
#67205=CARTESIAN_POINT('Ctrl Pts',(45.3108889141777,-5.68700525908472,1.20500463782932));
#67206=CARTESIAN_POINT('Ctrl Pts',(45.4114588241355,-5.57258480437296,-1.65540435909754));
#67207=CARTESIAN_POINT('Ctrl Pts',(45.5120287340932,-4.1068173316415,-4.11437922396275));
#67208=CARTESIAN_POINT('Ctrl Pts',(45.6125986440511,-1.64515019125313,-5.57562066879259));
#67209=CARTESIAN_POINT('Ctrl Pts',(45.7131685540088,1.21546445432158,-5.68477890109438));
#67210=CARTESIAN_POINT('Ctrl Pts',(45.8137384639667,3.78133001603,-4.41538314350158));
#67211=CARTESIAN_POINT('Ctrl Pts',(45.9143083739244,5.43022630392851,-2.07526077449805));
#67212=CARTESIAN_POINT('Ctrl Pts',(46.0148782838823,5.76229738761891,0.768110545877321));
#67213=CARTESIAN_POINT('Ctrl Pts',(46.11544819384,4.69701631516247,3.42521572008903));
#67214=CARTESIAN_POINT('Ctrl Pts',(46.2160181037979,2.4927128296055,5.25170903070299));
#67215=CARTESIAN_POINT('Ctrl Pts',(46.3165880137556,-0.316071371332041,
5.80466742219323));
#67216=CARTESIAN_POINT('Ctrl Pts',(46.4171579237135,-3.04820853680487,4.94999896062587));
#67217=CARTESIAN_POINT('Ctrl Pts',(46.5177278336712,-5.04115775608791,2.89496001220778));
#67218=CARTESIAN_POINT('Ctrl Pts',(46.6182977436291,-5.81163055909281,0.13789575289385));
#67219=CARTESIAN_POINT('Ctrl Pts',(46.7188676535869,-5.17278795433587,-2.65260810779222));
#67220=CARTESIAN_POINT('Ctrl Pts',(46.8194375635447,-3.27954872353672,-4.79985678577976));
#67221=CARTESIAN_POINT('Ctrl Pts',(46.9200074735025,-0.591021750409563,
-5.78314432507005));
#67222=CARTESIAN_POINT('Ctrl Pts',(47.0205773834603,2.24082748842343,-5.36402434382742));
#67223=CARTESIAN_POINT('Ctrl Pts',(47.1211472934181,4.52927799028237,-3.64413307671263));
#67224=CARTESIAN_POINT('Ctrl Pts',(47.2217172033759,5.71938247843022,-1.04054267546927));
#67225=CARTESIAN_POINT('Ctrl Pts',(47.3222871133337,5.52254163896719,1.8153784288464));
#67226=CARTESIAN_POINT('Ctrl Pts',(47.4228570232915,3.98648920601686,4.23107182689664));
#67227=CARTESIAN_POINT('Ctrl Pts',(47.5234269332493,1.48371657229165,5.62073394915242));
#67228=CARTESIAN_POINT('Ctrl Pts',(47.6239968432071,-1.37885605298849,5.64737292722768));
#67229=CARTESIAN_POINT('Ctrl Pts',(47.7245667531649,-3.90705727237777,4.30452883187085));
#67230=CARTESIAN_POINT('Ctrl Pts',(47.8251366631227,-5.48780046652238,1.91784020024717));
#67231=CARTESIAN_POINT('Ctrl Pts',(47.9257065730805,-5.73775677159133,-0.933923029004594));
#67232=CARTESIAN_POINT('Ctrl Pts',(48.0262764830383,-4.59631199877497,-3.55921072767047));
#67233=CARTESIAN_POINT('Ctrl Pts',(48.1268463929962,-2.34026552289286,-5.32139288874693));
#67234=CARTESIAN_POINT('Ctrl Pts',(48.2274163029538,0.483293327723093,-5.79314185510984));
#67235=CARTESIAN_POINT('Ctrl Pts',(48.3279862129118,3.18965396239895,-4.8600589085113));
#67236=CARTESIAN_POINT('Ctrl Pts',(48.4285561228695,5.12252625693867,-2.74841586027683));
#67237=CARTESIAN_POINT('Ctrl Pts',(48.5291260328273,5.81319034378827,0.0297156681595752));
#67238=CARTESIAN_POINT('Ctrl Pts',(48.629695942785,5.09416077643017,2.80064117264737));
#67239=CARTESIAN_POINT('Ctrl Pts',(48.730265852743,3.13980160598745,4.89241360364045));
#67240=CARTESIAN_POINT('Ctrl Pts',(48.8308357627007,0.424043248924028,5.79777994728061));
#67241=CARTESIAN_POINT('Ctrl Pts',(48.9314056726585,-2.39454523097487,5.29718964460052));
#67242=CARTESIAN_POINT('Ctrl Pts',(49.0319755826163,-4.63245855365558,3.51203541307753));
#67243=CARTESIAN_POINT('Ctrl Pts',(49.1325454925742,-5.74700466482796,0.875215617144052));
#67244=CARTESIAN_POINT('Ctrl Pts',(49.2331154025319,-5.46790709196603,-1.97384321253615));
#67245=CARTESIAN_POINT('Ctrl Pts',(49.3336853124898,-3.86284675623355,-4.3442467623172));
#67246=CARTESIAN_POINT('Ctrl Pts',(49.4342552224475,-1.3210494073637,-5.66117421188848));
#67247=CARTESIAN_POINT('Ctrl Pts',(49.5348251324054,1.54110128559463,-5.60527178837798));
#67248=CARTESIAN_POINT('Ctrl Pts',(49.6353950423631,4.02953624342044,-4.19009578136448));
#67249=CARTESIAN_POINT('Ctrl Pts',(49.735964952321,5.54081213095715,-1.75882515432473));
#67250=CARTESIAN_POINT('Ctrl Pts',(49.8365348622786,5.70844584642674,1.09895905859165));
#67251=CARTESIAN_POINT('Ctrl Pts',(49.9371047722366,4.49178635813174,3.69024664581502));
#67252=CARTESIAN_POINT('Ctrl Pts',(50.0376746821943,2.18587254464829,5.38665259809838));
#67253=CARTESIAN_POINT('Ctrl Pts',(50.1382445921522,-0.650113479250571,
5.77679993232794));
#67254=CARTESIAN_POINT('Ctrl Pts',(50.2388145021098,-3.32844754406752,4.76607825580302));
#67255=CARTESIAN_POINT('Ctrl Pts',(50.3393844120678,-5.19963594467117,2.5995867050227));
#67256=CARTESIAN_POINT('Ctrl Pts',(50.4399543220255,-5.80991710468783,-0.197302383926823));
#67257=CARTESIAN_POINT('Ctrl Pts',(50.5405242319834,-5.01129836816094,-2.94634581461765));
#67258=CARTESIAN_POINT('Ctrl Pts',(50.6410941419411,-2.99744409122436,-4.98090292156266));
#67259=CARTESIAN_POINT('Ctrl Pts',(50.7416640518989,-0.256712202451727,
-5.80759535773281));
#67260=CARTESIAN_POINT('Ctrl Pts',(50.8422339618567,2.54627217443023,-5.2259509189974));
#67261=CARTESIAN_POINT('Ctrl Pts',(50.9428038718146,4.73178774091697,-3.37701788105352));
#67262=CARTESIAN_POINT('Ctrl Pts',(51.0433737817723,5.76984885348993,-0.709160913988021));
#67263=CARTESIAN_POINT('Ctrl Pts',(51.1439436917302,5.40872658594295,2.13066696425354));
#67264=CARTESIAN_POINT('Ctrl Pts',(51.2445136016879,3.73599277729174,4.45380993780282));
#67265=CARTESIAN_POINT('Ctrl Pts',(51.3450835116458,1.15728393619704,5.69690783540226));
#67266=CARTESIAN_POINT('Ctrl Pts',(51.4456534216035,-1.70206526320226,5.55851048697829));
#67267=CARTESIAN_POINT('Ctrl Pts',(51.5462233315614,-4.14866510146161,4.07217913038731));
#67268=CARTESIAN_POINT('Ctrl Pts',(51.6467932415191,-5.58921722390637,1.59834784012599));
#67269=CARTESIAN_POINT('Ctrl Pts',(51.747363151477,-5.67438898091241,-1.2630814254622));
#67270=CARTESIAN_POINT('Ctrl Pts',(51.8479330614348,-4.38352629472378,-3.81821453267259));
#67271=CARTESIAN_POINT('Ctrl Pts',(51.9485029713925,-2.02966225553008,-5.44743390253828));
#67272=CARTESIAN_POINT('Ctrl Pts',(52.0490728813504,0.816393133438721,-5.75565524034613));
#67273=CARTESIAN_POINT('Ctrl Pts',(52.1496427913082,3.46447389032224,-4.66813513700239));
#67274=CARTESIAN_POINT('Ctrl Pts',(52.250212701266,5.27242271112307,-2.44859628140164));
#67275=CARTESIAN_POINT('Ctrl Pts',(52.3507826112238,5.80181356312538,0.364725064619975));
#67276=CARTESIAN_POINT('Ctrl Pts',(52.4513525211815,4.9242696204448,3.08960089643144));
#67277=CARTESIAN_POINT('Ctrl Pts',(52.5519224311394,2.85259453374416,5.06525117048629));
#67278=CARTESIAN_POINT('Ctrl Pts',(52.6524923410972,0.0891677282345522,
5.81258239599026));
#67279=CARTESIAN_POINT('Ctrl Pts',(52.753062251055,-2.6958821746702,5.15036739414614));
#67280=CARTESIAN_POINT('Ctrl Pts',(52.8536321610128,-4.82718297079972,3.23919273272347));
#67281=CARTESIAN_POINT('Ctrl Pts',(52.9542020709706,-5.78789605210394,0.542516622165996));
#67282=CARTESIAN_POINT('Ctrl Pts',(53.0547719809283,-5.34504932273691,-2.28571930256727));
#67283=CARTESIAN_POINT('Ctrl Pts',(53.1553418908863,-3.60603273460568,-4.55967026342535));
#67284=CARTESIAN_POINT('Ctrl Pts',(53.2559118008439,-0.99255631088897,-5.72790511170206));
#67285=CARTESIAN_POINT('Ctrl Pts',(53.3564817108019,1.86161416062682,-5.50712789877888));
#67286=CARTESIAN_POINT('Ctrl Pts',(53.4570516207595,4.26434480692677,-3.95087691570875));
#67287=CARTESIAN_POINT('Ctrl Pts',(53.5576215307175,5.63297549627246,-1.43654167257841));
#67288=CARTESIAN_POINT('Ctrl Pts',(53.6581914406752,5.63561450056838,1.42615367186469));
#67289=CARTESIAN_POINT('Ctrl Pts',(53.758761350633,4.2716217932542,3.94300801314016));
#67290=CARTESIAN_POINT('Ctrl Pts',(53.8593312605908,1.87176456925964,5.50368623779372));
#67291=CARTESIAN_POINT('Ctrl Pts',(53.9599011705486,-0.981994129710483,
5.72972541999358));
#67292=CARTESIAN_POINT('Ctrl Pts',(54.0604710805064,-3.59761974878958,4.56631086087063));
#67293=CARTESIAN_POINT('Ctrl Pts',(54.1610409904643,-5.34082635831325,2.29557035626498));
#67294=CARTESIAN_POINT('Ctrl Pts',(54.261610900422,-5.78888583753521,-0.531844976840823));
#67295=CARTESIAN_POINT('Ctrl Pts',(54.3621808103798,-4.83314809906796,-3.23028641703264));
#67296=CARTESIAN_POINT('Ctrl Pts',(54.4627507203376,-2.70537098973005,-5.14538998627536));
#67297=CARTESIAN_POINT('Ctrl Pts',(54.5633206302954,0.078446240209487,-5.81273346716538));
#67298=CARTESIAN_POINT('Ctrl Pts',(54.6638905402532,2.84325992667244,-5.0705086592284));
#67299=CARTESIAN_POINT('Ctrl Pts',(54.764460450211,4.91854716216131,-3.09866134240672));
#67300=CARTESIAN_POINT('Ctrl Pts',(54.8650303601689,5.8011660495001,-0.375447161461482));
#67301=CARTESIAN_POINT('Ctrl Pts',(54.9656002701266,5.27686000591952,2.43892212337069));
#67302=CARTESIAN_POINT('Ctrl Pts',(55.0661701800844,3.47320975124282,4.66163850225691));
#67303=CARTESIAN_POINT('Ctrl Pts',(55.1667400900422,0.826722671906332,5.75435770195244));
#67304=CARTESIAN_POINT('Ctrl Pts',(55.2337866966808,-1.07034715964058,5.55179856586871));
#67305=CARTESIAN_POINT('Ctrl Pts',(55.26731,-1.93782473268743,5.23040479991605));
#67306=CARTESIAN_POINT('Ctrl Pts',(18.5943714011907,-2.5844886242714,5.20662521554142));
#67307=CARTESIAN_POINT('Ctrl Pts',(18.62789470451,-3.44802228533999,4.77798039642798));
#67308=CARTESIAN_POINT('Ctrl Pts',(18.6949413111485,-4.95685577985632,3.48321239743886));
#67309=CARTESIAN_POINT('Ctrl Pts',(18.7955112211063,-6.01818731712236,0.694543040107923));
#67310=CARTESIAN_POINT('Ctrl Pts',(18.8960811310641,-5.62003321802158,-2.26178872417008));
#67311=CARTESIAN_POINT('Ctrl Pts',(18.9966510410219,-3.85906871975241,-4.67001313762182));
#67312=CARTESIAN_POINT('Ctrl Pts',(19.0972209509797,-1.1622613390067,-5.94557351228712));
#67313=CARTESIAN_POINT('Ctrl Pts',(19.1977908609375,1.81638213979233,-5.77943430746988));
#67314=CARTESIAN_POINT('Ctrl Pts',(19.2983607708953,4.35456027613521,-4.21173777105813));
#67315=CARTESIAN_POINT('Ctrl Pts',(19.3989306808532,5.83675834943404,-1.62272373465775));
#67316=CARTESIAN_POINT('Ctrl Pts',(19.4995005908109,5.90354905198227,1.35981232901817));
#67317=CARTESIAN_POINT('Ctrl Pts',(19.6000705007687,4.53873342263602,4.0125884728718));
#67318=CARTESIAN_POINT('Ctrl Pts',(19.7006404107265,2.0732792381507,5.69231873872973));
#67319=CARTESIAN_POINT('Ctrl Pts',(19.8012103206843,-0.894943577534932,
5.99166488739198));
#67320=CARTESIAN_POINT('Ctrl Pts',(19.9017802306421,-3.64614324352199,4.83803833909629));
#67321=CARTESIAN_POINT('Ctrl Pts',(20.0023501405999,-5.51315636405137,2.51119120843917));
#67322=CARTESIAN_POINT('Ctrl Pts',(20.1029200505578,-6.04323378541225,-0.424617398710297));
#67323=CARTESIAN_POINT('Ctrl Pts',(20.2034899605155,-5.1078322296771,-3.25745676963478));
#67324=CARTESIAN_POINT('Ctrl Pts',(20.3040598704734,-2.93378574822532,-5.30036561803028));
#67325=CARTESIAN_POINT('Ctrl Pts',(20.4046297804311,-0.0482987518864741,
-6.05794039741912));
#67326=CARTESIAN_POINT('Ctrl Pts',(20.505199690389,2.8489006520323,-5.3464698296177));
#67327=CARTESIAN_POINT('Ctrl Pts',(20.6057696003468,5.05524409931645,-3.33848493853243));
#67328=CARTESIAN_POINT('Ctrl Pts',(20.7063395103046,6.03569520469174,-0.520920319627098));
#67329=CARTESIAN_POINT('Ctrl Pts',(20.8069094202624,5.55249541838547,2.42296702627515));
#67330=CARTESIAN_POINT('Ctrl Pts',(20.9074793302202,3.72282027299234,4.77928695513278));
#67331=CARTESIAN_POINT('Ctrl Pts',(21.008049240178,0.9903644160455,5.97663391097251));
#67332=CARTESIAN_POINT('Ctrl Pts',(21.1086191501357,-1.98225395922582,5.72465228853798));
#67333=CARTESIAN_POINT('Ctrl Pts',(21.2091890600936,-4.47417745578252,4.08444741393546));
#67334=CARTESIAN_POINT('Ctrl Pts',(21.3097589700513,-5.88111677080375,1.45376755753582));
#67335=CARTESIAN_POINT('Ctrl Pts',(21.4103288800092,-5.86189033154339,-1.52944968015864));
#67336=CARTESIAN_POINT('Ctrl Pts',(21.510898789967,-4.42116053296483,-4.14177668698978));
#67337=CARTESIAN_POINT('Ctrl Pts',(21.6114686999248,-1.90830311100522,-5.74972641259574));
#67338=CARTESIAN_POINT('Ctrl Pts',(21.7120386098826,1.06731617265169,-5.96337243267167));
#67339=CARTESIAN_POINT('Ctrl Pts',(21.8126085198404,3.78411220321663,-4.73090577126927));
#67340=CARTESIAN_POINT('Ctrl Pts',(21.9131784297982,5.58326428197402,-2.35119853283214));
#67341=CARTESIAN_POINT('Ctrl Pts',(22.0137483397559,6.02847957858663,0.598672325837003));
#67342=CARTESIAN_POINT('Ctrl Pts',(22.1143182497138,5.01179376688014,3.4033656608453));
#67343=CARTESIAN_POINT('Ctrl Pts',(22.2148881596716,2.779752281001,5.38274575281322));
#67344=CARTESIAN_POINT('Ctrl Pts',(22.3154580696294,-0.126376740130381,
6.05681463334594));
#67345=CARTESIAN_POINT('Ctrl Pts',(22.4160279795872,-3.00185951056889,5.26211117917195));
#67346=CARTESIAN_POINT('Ctrl Pts',(22.516597889545,-5.14939393378118,3.19135029382499));
#67347=CARTESIAN_POINT('Ctrl Pts',(22.6171677995028,-6.04820476079752,0.34668970943132));
#67348=CARTESIAN_POINT('Ctrl Pts',(22.7177377094606,-5.48033113978855,-2.58204283105899));
#67349=CARTESIAN_POINT('Ctrl Pts',(22.8183076194184,-3.5834819350071,-4.88463220771401));
#67350=CARTESIAN_POINT('Ctrl Pts',(22.9188775293762,-0.817641445750429,
-6.00270247882989));
#67351=CARTESIAN_POINT('Ctrl Pts',(23.019447439334,2.14647639025152,-5.66512256612795));
#67352=CARTESIAN_POINT('Ctrl Pts',(23.1200173492918,4.59007554936591,-3.95375530783995));
#67353=CARTESIAN_POINT('Ctrl Pts',(23.2205872592496,5.92058533902773,-1.28360579090672));
#67354=CARTESIAN_POINT('Ctrl Pts',(23.3211571692074,5.81535828058497,1.69781702535671));
#67355=CARTESIAN_POINT('Ctrl Pts',(23.4217270791652,4.29991184512756,4.26752067450071));
#67356=CARTESIAN_POINT('Ctrl Pts',(23.522296989123,1.74174048871413,5.80235423368249));
#67357=CARTESIAN_POINT('Ctrl Pts',(23.6228668990808,-1.2388014368723,5.93012188602919));
#67358=CARTESIAN_POINT('Ctrl Pts',(23.7234368090386,-3.91893508041301,4.6198400858328));
#67359=CARTESIAN_POINT('Ctrl Pts',(23.8240067189964,-5.64873034048527,2.18925104171279));
#67360=CARTESIAN_POINT('Ctrl Pts',(23.9245766289542,-6.00871335557892,-0.772229495452498));
#67361=CARTESIAN_POINT('Ctrl Pts',(24.025146538912,-4.91158855441746,-3.54644504472784));
#67362=CARTESIAN_POINT('Ctrl Pts',(24.1257164488698,-2.62340775684606,-5.4606507235383));
#67363=CARTESIAN_POINT('Ctrl Pts',(24.2262863588276,0.300947163455891,-6.05065330257545));
#67364=CARTESIAN_POINT('Ctrl Pts',(24.3268562687854,3.15232265568373,-5.17337766431394));
#67365=CARTESIAN_POINT('Ctrl Pts',(24.4274261787433,5.23926261751802,-3.04156239584817));
#67366=CARTESIAN_POINT('Ctrl Pts',(24.527996088701,6.05568590471169,-0.172170864653346));
#67367=CARTESIAN_POINT('Ctrl Pts',(24.6285659986588,5.40361057292087,2.7389719530103));
#67368=CARTESIAN_POINT('Ctrl Pts',(24.7291359086166,3.44116432877971,4.98591642985454));
#67369=CARTESIAN_POINT('Ctrl Pts',(24.8297058185744,0.64423869716238,6.02378046447892));
#67370=CARTESIAN_POINT('Ctrl Pts',(24.9302757285322,-2.30891426393765,5.60088292191012));
#67371=CARTESIAN_POINT('Ctrl Pts',(25.03084563849,-4.70215750361244,3.81977609217878));
#67372=CARTESIAN_POINT('Ctrl Pts',(25.1314155484478,-5.95513159641322,1.11237684826688));
#67373=CARTESIAN_POINT('Ctrl Pts',(25.2319854584056,-5.76399140343187,-1.86477282378385));
#67374=CARTESIAN_POINT('Ctrl Pts',(25.3325553683634,-4.17508825692739,-4.3897166913169));
#67375=CARTESIAN_POINT('Ctrl Pts',(25.4331252783212,-1.57372980215375,-5.85015803999965));
#67376=CARTESIAN_POINT('Ctrl Pts',(25.533695188279,1.40925677493045,-5.89194109996629));
#67377=CARTESIAN_POINT('Ctrl Pts',(25.6342650982368,4.05049979722267,-4.50493351514298));
#67378=CARTESIAN_POINT('Ctrl Pts',(25.7348350081947,5.70950010547477,-2.02548343087346));
#67379=CARTESIAN_POINT('Ctrl Pts',(25.8354049181524,5.98395155305067,0.945144641788645));
#67380=CARTESIAN_POINT('Ctrl Pts',(25.9359748281102,4.80729990016889,3.68657595242462));
#67381=CARTESIAN_POINT('Ctrl Pts',(26.0365447380681,2.46488215975777,5.53401576810792));
#67382=CARTESIAN_POINT('Ctrl Pts',(26.1371146480258,-0.475267382553351,
6.03946152386455));
#67383=CARTESIAN_POINT('Ctrl Pts',(26.2376845579837,-3.30016499371908,5.08034305902568));
#67384=CARTESIAN_POINT('Ctrl Pts',(26.3382544679414,-5.32477543478461,2.8892457756781));
#67385=CARTESIAN_POINT('Ctrl Pts',(26.4388243778993,-6.05813241663425,-0.00249112112580119));
#67386=CARTESIAN_POINT('Ctrl Pts',(26.539394287857,-5.32239750246424,-2.89362392320112));
#67387=CARTESIAN_POINT('Ctrl Pts',(26.6399641978149,-3.29598577561902,-5.08305541481463));
#67388=CARTESIAN_POINT('Ctrl Pts',(26.7405341077727,-0.470300335465298,
-6.03985034397546));
#67389=CARTESIAN_POINT('Ctrl Pts',(26.8411040177305,2.46943253119076,-5.53198676399865));
#67390=CARTESIAN_POINT('Ctrl Pts',(26.9416739276883,4.81033013479139,-3.68262115584499));
#67391=CARTESIAN_POINT('Ctrl Pts',(27.0422438376461,5.98472682157525,-0.940223087504847));
#67392=CARTESIAN_POINT('Ctrl Pts',(27.1428137476039,5.70783240595158,2.03017827018424));
#67393=CARTESIAN_POINT('Ctrl Pts',(27.2433836575617,4.04679354535049,4.50826314498931));
#67394=CARTESIAN_POINT('Ctrl Pts',(27.3439535675195,1.40441073359784,5.89309808797669));
#67395=CARTESIAN_POINT('Ctrl Pts',(27.4445234774773,-1.57854047209525,5.84886181757755));
#67396=CARTESIAN_POINT('Ctrl Pts',(27.5450933874351,-4.17869697215815,4.38628159128385));
#67397=CARTESIAN_POINT('Ctrl Pts',(27.6456632973929,-5.7655230536149,1.8600318549408));
#67398=CARTESIAN_POINT('Ctrl Pts',(27.7462332073507,-5.95421475769761,-1.11727400505664));
#67399=CARTESIAN_POINT('Ctrl Pts',(27.8468031173085,-4.69901450859748,-3.82364188060932));
#67400=CARTESIAN_POINT('Ctrl Pts',(27.9473730272663,-2.30430728620892,-5.60277989161486));
#67401=CARTESIAN_POINT('Ctrl Pts',(28.0479429372241,0.649192469471501,-6.02324860193738));
#67402=CARTESIAN_POINT('Ctrl Pts',(28.1485128471819,3.44526361014859,-4.98308471127526));
#67403=CARTESIAN_POINT('Ctrl Pts',(28.2490827571396,5.40586129114638,-2.73452706771108));
#67404=CARTESIAN_POINT('Ctrl Pts',(28.3496526670975,6.05554226256158,0.177151035813719));
#67405=CARTESIAN_POINT('Ctrl Pts',(28.4502225770553,5.23675944809004,3.04587016565037));
#67406=CARTESIAN_POINT('Ctrl Pts',(28.5507924870131,3.14806697540939,5.17596840228919));
#67407=CARTESIAN_POINT('Ctrl Pts',(28.6513623969709,0.295970971138304,6.05089875699492));
#67408=CARTESIAN_POINT('Ctrl Pts',(28.7519323069287,-2.62789773885353,5.45849137191659));
#67409=CARTESIAN_POINT('Ctrl Pts',(28.8525022168865,-4.91450350934312,3.54240452797438));
#67410=CARTESIAN_POINT('Ctrl Pts',(28.9530721268443,-6.00934640936257,0.767287635401802));
#67411=CARTESIAN_POINT('Ctrl Pts',(29.0536420368021,-5.64692797812932,-2.19389584825251));
#67412=CARTESIAN_POINT('Ctrl Pts',(29.1542119467599,-3.91513437323725,-4.62306147727406));
#67413=CARTESIAN_POINT('Ctrl Pts',(29.2547818567177,-1.23392405309511,-5.93113867772054));
#67414=CARTESIAN_POINT('Ctrl Pts',(29.3553517666755,1.74651178772539,-5.80091985451407));
#67415=CARTESIAN_POINT('Ctrl Pts',(29.4559216766333,4.30342002346993,-4.2639829601861));
#67416=CARTESIAN_POINT('Ctrl Pts',(29.5564915865911,5.81675260803036,-1.69303386857182));
#67417=CARTESIAN_POINT('Ctrl Pts',(29.6570614965489,5.91952769237091,1.28847447875902));
#67418=CARTESIAN_POINT('Ctrl Pts',(29.7576314065067,4.58682240701069,3.95752887414659));
#67419=CARTESIAN_POINT('Ctrl Pts',(29.8582013164645,2.14181663641865,5.66688592430795));
#67420=CARTESIAN_POINT('Ctrl Pts',(29.9587712264223,-0.822577824767718,
6.00202801604255));
#67421=CARTESIAN_POINT('Ctrl Pts',(30.0593411363801,-3.5874978715465,4.88168348060468));
#67422=CARTESIAN_POINT('Ctrl Pts',(30.1599110463379,-5.4824527726963,2.57753490341331));
#67423=CARTESIAN_POINT('Ctrl Pts',(30.2604809562957,-6.04791759591984,-0.351663669039821));
#67424=CARTESIAN_POINT('Ctrl Pts',(30.3610508662535,-5.14676760835371,-3.19558410447297));
#67425=CARTESIAN_POINT('Ctrl Pts',(30.4616207762113,-2.99753090624697,-5.26457814542186));
#67426=CARTESIAN_POINT('Ctrl Pts',(30.5621906861691,-0.12139553973591,-6.0569165180058));
#67427=CARTESIAN_POINT('Ctrl Pts',(30.6627605961269,2.78417814066035,-5.38045784894078));
#67428=CARTESIAN_POINT('Ctrl Pts',(30.7633305060847,5.01459101864687,-3.39924278316002));
#67429=CARTESIAN_POINT('Ctrl Pts',(30.8639004160425,6.02896989131526,-0.593714268628649));
#67430=CARTESIAN_POINT('Ctrl Pts',(30.9644703260003,5.58132875524992,2.35578944495891));
#67431=CARTESIAN_POINT('Ctrl Pts',(31.0650402359581,3.78022020060429,4.73401624607505));
#67432=CARTESIAN_POINT('Ctrl Pts',(31.1656101459159,1.06241150143411,5.96424818269493));
#67433=CARTESIAN_POINT('Ctrl Pts',(31.2661800558737,-1.91303107227957,5.74815506920718));
#67434=CARTESIAN_POINT('Ctrl Pts',(31.3667499658316,-4.42456525775745,4.13813929961341));
#67435=CARTESIAN_POINT('Ctrl Pts',(31.4673198757893,-5.86314617702181,1.5246283120924));
#67436=CARTESIAN_POINT('Ctrl Pts',(31.5678897857471,-5.87991919552279,-1.45860372866722));
#67437=CARTESIAN_POINT('Ctrl Pts',(31.6684596957049,-4.47081687071256,-4.08812562083301));
#67438=CARTESIAN_POINT('Ctrl Pts',(31.7690296056627,-1.97754530336189,-5.72628056912257));
#67439=CARTESIAN_POINT('Ctrl Pts',(31.8695995156205,0.995279297726343,-5.97581740874642));
#67440=CARTESIAN_POINT('Ctrl Pts',(31.9701694255783,3.72674952588087,-4.77622367090424));
#67441=CARTESIAN_POINT('Ctrl Pts',(32.0707393355362,5.55448620210214,-2.41839980437813));
#67442=CARTESIAN_POINT('Ctrl Pts',(32.1713092454939,6.03526475577469,0.525883932881758));
#67443=CARTESIAN_POINT('Ctrl Pts',(32.2718791554517,5.05249680150087,3.34264126911381));
#67444=CARTESIAN_POINT('Ctrl Pts',(32.3724490654095,2.8445027221972,5.34881097502727));
#67445=CARTESIAN_POINT('Ctrl Pts',(32.4730189753674,-0.053280818609776,
6.05789862390643));
#67446=CARTESIAN_POINT('Ctrl Pts',(32.5735888853251,-2.93814380676952,5.29795107130118));
#67447=CARTESIAN_POINT('Ctrl Pts',(32.674158795283,-5.11050945102608,3.2532549445336));
#67448=CARTESIAN_POINT('Ctrl Pts',(32.7747287052407,-6.04358095268194,0.419647294211818));
#67449=CARTESIAN_POINT('Ctrl Pts',(32.8752986151986,-5.51108927580026,-2.51572446371195));
#67450=CARTESIAN_POINT('Ctrl Pts',(32.9758685251563,-3.64216319364069,-4.84103520479332));
#67451=CARTESIAN_POINT('Ctrl Pts',(33.0764384351142,-0.890015672301798,
-5.99239907601425));
#67452=CARTESIAN_POINT('Ctrl Pts',(33.1770083450719,2.07795988341927,-5.69061132973071));
#67453=CARTESIAN_POINT('Ctrl Pts',(33.2775782550298,4.54203195617863,-4.00885523462889));
#67454=CARTESIAN_POINT('Ctrl Pts',(33.3781481649875,5.90466518947603,-1.35495519606713));
#67455=CARTESIAN_POINT('Ctrl Pts',(33.4787180749454,5.83542219723063,1.62752031115663));
#67456=CARTESIAN_POINT('Ctrl Pts',(33.5792879849031,4.35109434545558,4.21532354394106));
#67457=CARTESIAN_POINT('Ctrl Pts',(33.679857894861,1.81162986045434,5.78091444599118));
#67458=CARTESIAN_POINT('Ctrl Pts',(33.7804278048188,-1.16715330620413,5.94463857126538));
#67459=CARTESIAN_POINT('Ctrl Pts',(33.8809977147765,-3.86290280082714,4.66679296032308));
#67460=CARTESIAN_POINT('Ctrl Pts',(33.9815676247344,-5.62190169154708,2.25725407381167));
#67461=CARTESIAN_POINT('Ctrl Pts',(34.0821375346921,-6.01759426156107,-0.699666982490047));
#67462=CARTESIAN_POINT('Ctrl Pts',(34.18270744465,-4.95402540326419,-3.48691939783132));
#67463=CARTESIAN_POINT('Ctrl Pts',(34.2832773546078,-2.6891096492429,-5.42859686083872));
#67464=CARTESIAN_POINT('Ctrl Pts',(34.3838472645656,0.227912879857088,-6.0538442581846));
#67465=CARTESIAN_POINT('Ctrl Pts',(34.4844171745234,3.08966673178568,-5.21103963424345));
#67466=CARTESIAN_POINT('Ctrl Pts',(34.5849870844812,5.20217906092996,-3.10456238481063));
#67467=CARTESIAN_POINT('Ctrl Pts',(34.685556994439,6.05316744598368,-0.24523142955757));
#67468=CARTESIAN_POINT('Ctrl Pts',(34.7861269043967,5.43626793612645,2.67356793626095));
#67469=CARTESIAN_POINT('Ctrl Pts',(34.8866968143546,3.50107813145393,4.94402937902015));
#67470=CARTESIAN_POINT('Ctrl Pts',(34.9872667243123,0.716879893732276,6.01556795332924));
#67471=CARTESIAN_POINT('Ctrl Pts',(35.0878366342702,-2.24116110110868,5.62833647732939));
#67472=CARTESIAN_POINT('Ctrl Pts',(35.188406544228,-4.65572245818653,3.87623825061062));
#67473=CARTESIAN_POINT('Ctrl Pts',(35.2889764541858,-5.94127512693356,1.18415558489583));
#67474=CARTESIAN_POINT('Ctrl Pts',(35.3895463641436,-5.78607369181921,-1.79508379080112));
#67475=CARTESIAN_POINT('Ctrl Pts',(35.4901162741014,-4.22775436725687,-4.33901689248841));
#67476=CARTESIAN_POINT('Ctrl Pts',(35.5906861840592,-1.64420824800695,-5.83074213289743));
#67477=CARTESIAN_POINT('Ctrl Pts',(35.691256094017,1.33805695600305,-5.90851742534887));
#67478=CARTESIAN_POINT('Ctrl Pts',(35.7918260039748,3.9958445000201,-4.55348232837445));
#67479=CARTESIAN_POINT('Ctrl Pts',(35.8923959139326,5.68464319251983,-2.09423168653741));
#67480=CARTESIAN_POINT('Ctrl Pts',(35.9929658238904,5.99492080433738,0.872868336510265));
#67481=CARTESIAN_POINT('Ctrl Pts',(36.0935357338482,4.85143528170287,3.62829853934429));
#67482=CARTESIAN_POINT('Ctrl Pts',(36.194105643806,2.53148087951004,5.50386946973076));
#67483=CARTESIAN_POINT('Ctrl Pts',(36.2946755537638,-0.402355456792645,
6.04475679159621));
#67484=CARTESIAN_POINT('Ctrl Pts',(36.3952454637216,-3.23862094118222,5.11979579499956));
#67485=CARTESIAN_POINT('Ctrl Pts',(36.4958153736794,-5.2895236352329,2.95328872538259));
#67486=CARTESIAN_POINT('Ctrl Pts',(36.5963852836372,-6.05772140111323,0.0706116821359479));
#67487=CARTESIAN_POINT('Ctrl Pts',(36.696955193595,-5.35692694188392,-2.82918863324405));
#67488=CARTESIAN_POINT('Ctrl Pts',(36.7975251035528,-3.35708231064414,-5.04291314050912));
#67489=CARTESIAN_POINT('Ctrl Pts',(36.8980950135106,-0.54314810894586,-6.03373555228499));
#67490=CARTESIAN_POINT('Ctrl Pts',(36.9986649234684,2.40249904161435,-5.56138228664435));
#67491=CARTESIAN_POINT('Ctrl Pts',(37.0992348334262,4.76554224272314,-3.74039860388978));
#67492=CARTESIAN_POINT('Ctrl Pts',(37.199804743384,5.97294555228697,-1.01237147953434));
#67493=CARTESIAN_POINT('Ctrl Pts',(37.3003746533419,5.73191470710404,1.96115485712974));
#67494=CARTESIAN_POINT('Ctrl Pts',(37.4009445632996,4.10089947964499,4.45910282915821));
#67495=CARTESIAN_POINT('Ctrl Pts',(37.5015144732574,1.47541965854388,5.87572220363945));
#67496=CARTESIAN_POINT('Ctrl Pts',(37.6020843832152,-1.50784815967059,5.86748400172828));
#67497=CARTESIAN_POINT('Ctrl Pts',(37.702654293173,-4.12546409716388,4.43638598029649));
#67498=CARTESIAN_POINT('Ctrl Pts',(37.8032242031308,-5.74265854241269,1.92946817761106));
#67499=CARTESIAN_POINT('Ctrl Pts',(37.9037941130886,-5.9672632345716,-1.04534399720345));
#67500=CARTESIAN_POINT('Ctrl Pts',(38.0043640230464,-4.74481172913825,-3.76666115255824));
#67501=CARTESIAN_POINT('Ctrl Pts',(38.1049339330042,-2.37174746385888,-5.57456622086761));
#67502=CARTESIAN_POINT('Ctrl Pts',(38.205503842962,0.576463519738073,-6.03064377936308));
#67503=CARTESIAN_POINT('Ctrl Pts',(38.3060737529198,3.38488259603486,-5.02429541271407));
#67504=CARTESIAN_POINT('Ctrl Pts',(38.4066436628776,5.37247055659719,-2.79955973353948));
#67505=CARTESIAN_POINT('Ctrl Pts',(38.5072135728355,6.0572390319614,0.104066771077096));
#67506=CARTESIAN_POINT('Ctrl Pts',(38.6077834827932,5.27313225632011,2.98245717329113));
#67507=CARTESIAN_POINT('Ctrl Pts',(38.708353392751,3.21029544778464,5.13760427836678));
#67508=CARTESIAN_POINT('Ctrl Pts',(38.8089233027089,0.368964756675754,6.04688676853557));
#67509=CARTESIAN_POINT('Ctrl Pts',(38.9094932126666,-2.56183957031156,5.48980442266801));
#67510=CARTESIAN_POINT('Ctrl Pts',(39.0100631226245,-4.87140000680326,3.60144923008454));
#67511=CARTESIAN_POINT('Ctrl Pts',(39.1106330325822,-5.99965013508599,0.839745699436374));
#67512=CARTESIAN_POINT('Ctrl Pts',(39.2112029425401,-5.6729902702813,-2.12559544044792));
#67513=CARTESIAN_POINT('Ctrl Pts',(39.3117728524979,-3.97063514840612,-4.57548151579714));
#67514=CARTESIAN_POINT('Ctrl Pts',(39.4123427624556,-1.30540442107904,-5.91581726227125));
#67515=CARTESIAN_POINT('Ctrl Pts',(39.5129126724135,1.67638575463012,-5.82157241514975));
#67516=CARTESIAN_POINT('Ctrl Pts',(39.6134825823712,4.25165382792243,-4.31560126873092));
#67517=CARTESIAN_POINT('Ctrl Pts',(39.7140524923291,5.79589950788908,-1.76310052963817));
#67518=CARTESIAN_POINT('Ctrl Pts',(39.8146224022869,5.93464454646915,1.21695057016433));
#67519=CARTESIAN_POINT('Ctrl Pts',(39.9151923122447,4.63424339124267,3.90189220428793));
#67520=CARTESIAN_POINT('Ctrl Pts',(40.0157622222025,2.21004220292946,5.64062833773242));
#67521=CARTESIAN_POINT('Ctrl Pts',(40.1163321321603,-0.750092317126442,
6.01151695489143));
#67522=CARTESIAN_POINT('Ctrl Pts',(40.2169020421181,-3.52833009598016,4.92461788537547));
#67523=CARTESIAN_POINT('Ctrl Pts',(40.3174719520759,-5.45095086384642,2.64350321790825));
#67524=CARTESIAN_POINT('Ctrl Pts',(40.4180418620337,-6.05172073956474,-0.278658704298321));
#67525=CARTESIAN_POINT('Ctrl Pts',(40.5186117719915,-5.1849535454334,-3.13324613058997));
#67526=CARTESIAN_POINT('Ctrl Pts',(40.6191816819493,-3.06083957989115,-5.22802406740167));
#67527=CARTESIAN_POINT('Ctrl Pts',(40.719751591907,-0.19447465108379,-6.05501066830152));
#67528=CARTESIAN_POINT('Ctrl Pts',(40.8203215018649,2.71905021320203,-5.41366239446507));
#67529=CARTESIAN_POINT('Ctrl Pts',(40.9208914118227,4.97320774142276,-3.4595056502067));
#67530=CARTESIAN_POINT('Ctrl Pts',(41.0214613217805,6.02136667342831,-0.666421763814872));
#67531=CARTESIAN_POINT('Ctrl Pts',(41.1220312317383,5.60934937049263,2.2882688266271));
#67532=CARTESIAN_POINT('Ctrl Pts',(41.2226011416961,3.83706967390126,4.68805619641941));
#67533=CARTESIAN_POINT('Ctrl Pts',(41.3231710516539,1.13430388444848,5.95099397419325));
#67534=CARTESIAN_POINT('Ctrl Pts',(41.4237409616117,-1.84352962054176,5.77082083601151));
#67535=CARTESIAN_POINT('Ctrl Pts',(41.5243108715695,-4.37430877951378,4.19122861278503));
#67536=CARTESIAN_POINT('Ctrl Pts',(41.6248807815273,-5.84432182498416,1.59526705888798));
#67537=CARTESIAN_POINT('Ctrl Pts',(41.7254506914851,-5.89709185885572,-1.38754538353777));
#67538=CARTESIAN_POINT('Ctrl Pts',(41.8260206014429,-4.51982219334054,-4.03387926489447));
#67539=CARTESIAN_POINT('Ctrl Pts',(41.9265905114008,-2.04649953673286,-5.70200089699322));
#67540=CARTESIAN_POINT('Ctrl Pts',(42.0271604213585,0.923097495847049,-5.98739222001702));
#67541=CARTESIAN_POINT('Ctrl Pts',(42.1277303313163,3.66884418031286,-4.8208460838056));
#67542=CARTESIAN_POINT('Ctrl Pts',(42.2283002412741,5.52489930929906,-2.48524892219391));
#67543=CARTESIAN_POINT('Ctrl Pts',(42.3288701512318,6.04117111177205,0.453018963676277));
#67544=CARTESIAN_POINT('Ctrl Pts',(42.4294400611898,5.09246412005362,3.28143014082667));
#67545=CARTESIAN_POINT('Ctrl Pts',(42.5300099711475,2.90883896296137,5.31409733357577));
#67546=CARTESIAN_POINT('Ctrl Pts',(42.6305798811053,0.01982286136298,6.05810049746014));
#67547=CARTESIAN_POINT('Ctrl Pts',(42.731149791063,-2.87400026705184,5.33301950569705));
#67548=CARTESIAN_POINT('Ctrl Pts',(42.831719701021,-5.07088080472847,3.31468587461856));
#67549=CARTESIAN_POINT('Ctrl Pts',(42.9322896109787,-6.03807711241803,0.492543772321716));
#67550=CARTESIAN_POINT('Ctrl Pts',(43.0328595209366,-5.54104491809615,-2.44903977076732));
#67551=CARTESIAN_POINT('Ctrl Pts',(43.1334294308942,-3.70031410102634,-4.79673327764896));
#67552=CARTESIAN_POINT('Ctrl Pts',(43.2339993408522,-0.962260299794141,
-5.98122309386629));
#67553=CARTESIAN_POINT('Ctrl Pts',(43.3345692508099,2.00914079579688,-5.71527145862941));
#67554=CARTESIAN_POINT('Ctrl Pts',(43.4351391607677,4.49332697793318,-4.06337141454449));
#67555=CARTESIAN_POINT('Ctrl Pts',(43.5357090707255,5.8878852359054,-1.42610730029916));
#67556=CARTESIAN_POINT('Ctrl Pts',(43.6362789806834,5.85463639263101,1.55698660663465));
#67557=CARTESIAN_POINT('Ctrl Pts',(43.7368488906411,4.40164326398255,4.16251260175827));
#67558=CARTESIAN_POINT('Ctrl Pts',(43.8374188005989,1.88125543287904,5.75863287416575));
#67559=CARTESIAN_POINT('Ctrl Pts',(43.9379887105567,-1.095335221259,5.95828963178433));
#67560=CARTESIAN_POINT('Ctrl Pts',(44.0385586205146,-3.80630802713771,4.71306628276184));
#67561=CARTESIAN_POINT('Ctrl Pts',(44.1391285304723,-5.59425441301462,2.32492841731219));
#67562=CARTESIAN_POINT('Ctrl Pts',(44.2396984404302,-6.02559891943012,-0.627002587970594));
#67563=CARTESIAN_POINT('Ctrl Pts',(44.3402683503879,-4.99574087489218,-3.42688600541233));
#67564=CARTESIAN_POINT('Ctrl Pts',(44.4408382603457,-2.7544199686699,-5.39575251650331));
#67565=CARTESIAN_POINT('Ctrl Pts',(44.5414081703035,0.154845408871141,-6.05615368716076));
#67566=CARTESIAN_POINT('Ctrl Pts',(44.6419780802614,3.02656090805623,-5.2479428019925));
#67567=CARTESIAN_POINT('Ctrl Pts',(44.7425479902191,5.16433799238815,-3.16711030492081));
#67568=CARTESIAN_POINT('Ctrl Pts',(44.843117900177,6.04976755917625,-0.318256285245154));
#67569=CARTESIAN_POINT('Ctrl Pts',(44.9436878101347,5.46813370067749,2.60777460963838));
#67570=CARTESIAN_POINT('Ctrl Pts',(45.0442577200926,3.56048212689068,4.90142240653173));
#67571=CARTESIAN_POINT('Ctrl Pts',(45.1448276300503,0.789416702298039,6.00647948912606));
#67572=CARTESIAN_POINT('Ctrl Pts',(45.2453975400082,-2.17308159304928,5.65497046615715));
#67573=CARTESIAN_POINT('Ctrl Pts',(45.3459674499659,-4.60860947273312,3.93213597310593));
#67574=CARTESIAN_POINT('Ctrl Pts',(45.4465373599238,-5.92655352250245,1.25576189147193));
#67575=CARTESIAN_POINT('Ctrl Pts',(45.5471072698815,-5.80731344481216,-1.72513336784826));
#67576=CARTESIAN_POINT('Ctrl Pts',(45.6476771798394,-4.2798048558568,-4.28768527050947));
#67577=CARTESIAN_POINT('Ctrl Pts',(45.7482470897971,-1.71444727353495,-5.81047718603454));
#67578=CARTESIAN_POINT('Ctrl Pts',(45.848816999755,1.26666229677368,-5.92423338577162));
#67579=CARTESIAN_POINT('Ctrl Pts',(45.9493869097128,3.94060735049394,-4.60136808920917));
#67580=CARTESIAN_POINT('Ctrl Pts',(46.0499568196705,5.6589585139073,-2.16267499200307));
#67581=CARTESIAN_POINT('Ctrl Pts',(46.1505267296284,6.00501710909191,0.800464929071172));
#67582=CARTESIAN_POINT('Ctrl Pts',(46.2510966395861,4.89486422461261,3.56949279390883));
#67583=CARTESIAN_POINT('Ctrl Pts',(46.351666549544,2.59771097930425,5.47292172894527));
#67584=CARTESIAN_POINT('Ctrl Pts',(46.4522364595017,-0.329384942301194,
6.04917185596049));
#67585=CARTESIAN_POINT('Ctrl Pts',(46.5528063694596,-3.17660529894262,5.15850301520595));
#67586=CARTESIAN_POINT('Ctrl Pts',(46.6533762794173,-5.25350160510346,3.01690163385131));
#67587=CARTESIAN_POINT('Ctrl Pts',(46.7539461893752,-6.05642829439157,0.143704203323096));
#67588=CARTESIAN_POINT('Ctrl Pts',(46.8545160993329,-5.39067633583681,-2.76434137280626));
#67589=CARTESIAN_POINT('Ctrl Pts',(46.9550860092908,-3.41769000629041,-5.00203654565438));
#67590=CARTESIAN_POINT('Ctrl Pts',(47.0556559192486,-0.615916792264225,
-6.02674216207779));
#67591=CARTESIAN_POINT('Ctrl Pts',(47.1562258292064,2.33521571368719,-5.58996799218991));
#67592=CARTESIAN_POINT('Ctrl Pts',(47.2567957391642,4.72006041929019,-3.79763139620073));
#67593=CARTESIAN_POINT('Ctrl Pts',(47.3573656491219,5.96029453637867,-1.08437245574289));
#67594=CARTESIAN_POINT('Ctrl Pts',(47.4579355590799,5.7551623591878,1.8918458717737));
#67595=CARTESIAN_POINT('Ctrl Pts',(47.5585054690375,4.1544082641027,4.40929320394034));
#67596=CARTESIAN_POINT('Ctrl Pts',(47.6590753789954,1.54621374120647,5.85749072979751));
#67597=CARTESIAN_POINT('Ctrl Pts',(47.7596452889532,-1.4369362829072,5.88525179597474));
#67598=CARTESIAN_POINT('Ctrl Pts',(47.860215198911,-4.07163049537184,4.48584436782168));
#67599=CARTESIAN_POINT('Ctrl Pts',(47.9607851088687,-5.7189578176851,1.9986235420153));
#67600=CARTESIAN_POINT('Ctrl Pts',(48.0613550188267,-5.97944279225262,-0.973261772257315));
#67601=CARTESIAN_POINT('Ctrl Pts',(48.1619249287844,-4.78991803697473,-3.70913194456918));
#67602=CARTESIAN_POINT('Ctrl Pts',(48.2624948387422,-2.43884228102927,-5.54554081325017));
#67603=CARTESIAN_POINT('Ctrl Pts',(48.3630647487,0.503650628640414,-6.03716080847854));
#67604=CARTESIAN_POINT('Ctrl Pts',(48.4636346586578,3.3240086944217,-5.06477450461206));
#67605=CARTESIAN_POINT('Ctrl Pts',(48.5642045686156,5.33829751320773,-2.86418474328027));
#67606=CARTESIAN_POINT('Ctrl Pts',(48.6647744785734,6.05805378040047,0.0309673527246042));
#67607=CARTESIAN_POINT('Ctrl Pts',(48.7653443885312,5.30873722079254,2.91860989235135));
#67608=CARTESIAN_POINT('Ctrl Pts',(48.865914298489,3.27205645505567,5.098492045506));
#67609=CARTESIAN_POINT('Ctrl Pts',(48.9664842084468,0.44190481564781,6.04199426655359));
#67610=CARTESIAN_POINT('Ctrl Pts',(49.0670541184046,-2.49540836115029,5.5203180790839));
#67611=CARTESIAN_POINT('Ctrl Pts',(49.1676240283624,-4.82758715848853,3.65996950948447));
#67612=CARTESIAN_POINT('Ctrl Pts',(49.2681939383203,-5.98908022561877,0.912081484441761));
#67613=CARTESIAN_POINT('Ctrl Pts',(49.3687638482779,-5.69822649360848,-2.05698551543216));
#67614=CARTESIAN_POINT('Ctrl Pts',(49.4693337582359,-4.02555774209492,-4.52723529852593));
#67615=CARTESIAN_POINT('Ctrl Pts',(49.5699036681935,-1.37669470343887,-5.8996344189011));
#67616=CARTESIAN_POINT('Ctrl Pts',(49.6704735781515,1.6060156157028,-5.84137727126729));
#67617=CARTESIAN_POINT('Ctrl Pts',(49.7710434881091,4.19926853054085,-4.36659116377622));
#67618=CARTESIAN_POINT('Ctrl Pts',(49.8716133980671,5.77420244157352,-1.83291045795632));
#67619=CARTESIAN_POINT('Ctrl Pts',(49.9721833080248,5.94889723112367,1.1452494560961));
#67620=CARTESIAN_POINT('Ctrl Pts',(50.0727532179827,4.68098956310768,3.84568736290879));
#67621=CARTESIAN_POINT('Ctrl Pts',(50.1733231279404,2.27794595556811,5.61354939469407));
#67622=CARTESIAN_POINT('Ctrl Pts',(50.2738930378982,-0.677497585275496,
6.02013053057035));
#67623=CARTESIAN_POINT('Ctrl Pts',(50.374462947856,-3.46864854489916,4.96683519508433));
#67624=CARTESIAN_POINT('Ctrl Pts',(50.4750328578139,-5.4186552182969,2.70908660038451));
#67625=CARTESIAN_POINT('Ctrl Pts',(50.5756027677716,-6.05464266579148,-0.205613162849079));
#67626=CARTESIAN_POINT('Ctrl Pts',(50.6761726777295,-5.22238447884166,-3.0704519110895));
#67627=CARTESIAN_POINT('Ctrl Pts',(50.7767425876872,-3.12370255135105,-5.19070871402375));
#67628=CARTESIAN_POINT('Ctrl Pts',(50.877312497645,-0.26752544413057,-6.0522231221182));
#67629=CARTESIAN_POINT('Ctrl Pts',(50.9778824076028,2.65352635299801,-5.44607863302619));
#67630=CARTESIAN_POINT('Ctrl Pts',(51.0784523175607,4.93110029375614,-3.519264763566));
#67631=CARTESIAN_POINT('Ctrl Pts',(51.1790222275184,6.01288665811098,-0.739032218425107));
#67632=CARTESIAN_POINT('Ctrl Pts',(51.2795921374763,5.63655318393917,2.22041500350376));
#67633=CARTESIAN_POINT('Ctrl Pts',(51.380162047434,3.89336041476873,4.64141349847986));
#67634=CARTESIAN_POINT('Ctrl Pts',(51.4807319573918,1.20603109653318,5.93687321553647));
#67635=CARTESIAN_POINT('Ctrl Pts',(51.5813018673497,-1.7737597244255,5.79264628845618));
#67636=CARTESIAN_POINT('Ctrl Pts',(51.6818717773074,-4.32341533911426,4.24370762290134));
#67637=CARTESIAN_POINT('Ctrl Pts',(51.7824416872653,-5.82464645578769,1.66567351189812));
#67638=CARTESIAN_POINT('Ctrl Pts',(51.8830115972231,-5.91340582095539,-1.31628499188082));
#67639=CARTESIAN_POINT('Ctrl Pts',(51.9835815071809,-4.56816936497055,-3.97904551822462));
#67640=CARTESIAN_POINT('Ctrl Pts',(52.0841514171387,-2.11515577039187,-5.67689093167526));
#67641=CARTESIAN_POINT('Ctrl Pts',(52.1847213270964,0.850781277720655,-5.99809518102555));
#67642=CARTESIAN_POINT('Ctrl Pts',(52.2852912370543,3.61040459836179,-4.86476651230871));
#67643=CARTESIAN_POINT('Ctrl Pts',(52.385861147012,5.49450791184205,-2.55173615208908));
#67644=CARTESIAN_POINT('Ctrl Pts',(52.4864310569699,6.04619778652662,0.380088028407498));
#67645=CARTESIAN_POINT('Ctrl Pts',(52.5870009669276,5.13168990272672,3.21974118920008));
#67646=CARTESIAN_POINT('Ctrl Pts',(52.6875708768855,2.97275163500614,5.27860988326863));
#67647=CARTESIAN_POINT('Ctrl Pts',(52.7881407868432,0.0929236548564317,
6.05742022460096));
#67648=CARTESIAN_POINT('Ctrl Pts',(52.8887106968011,-2.80943823166339,5.3673113759123));
#67649=CARTESIAN_POINT('Ctrl Pts',(52.9892806067589,-5.03051376533478,3.37563413881495));
#67650=CARTESIAN_POINT('Ctrl Pts',(53.0898505167167,-6.03169404154821,0.56536852906504));
#67651=CARTESIAN_POINT('Ctrl Pts',(53.1904204266745,-5.57019370450064,-2.38199846262534));
#67652=CARTESIAN_POINT('Ctrl Pts',(53.2909903366322,-3.75792618995677,-4.7517328769804));
#67653=CARTESIAN_POINT('Ctrl Pts',(53.3915602465901,-1.03436480759078,-5.96917616035072));
#67654=CARTESIAN_POINT('Ctrl Pts',(53.4921301565479,1.94002914690096,-5.7390993608176));
#67655=CARTESIAN_POINT('Ctrl Pts',(53.5927000665057,4.44396770976864,-4.11729591147515));
#67656=CARTESIAN_POINT('Ctrl Pts',(53.6932699764635,5.87024791585588,-1.49705173847708));
#67657=CARTESIAN_POINT('Ctrl Pts',(53.7938398864213,5.87299808039652,1.48622617398105));
#67658=CARTESIAN_POINT('Ctrl Pts',(53.894409796379,4.45155121760574,4.10909555467727));
#67659=CARTESIAN_POINT('Ctrl Pts',(53.9949797063369,1.95060711145293,5.73551273005053));
#67660=CARTESIAN_POINT('Ctrl Pts',(54.0955496162947,-1.02335772579348,5.97107314374103));
#67661=CARTESIAN_POINT('Ctrl Pts',(54.1961195262525,-3.74915883201502,4.75865318993734));
#67662=CARTESIAN_POINT('Ctrl Pts',(54.2966894362103,-5.56579286020032,2.39226446280162));
#67663=CARTESIAN_POINT('Ctrl Pts',(54.3972593461681,-6.03272551876107,-0.554247372267884));
#67664=CARTESIAN_POINT('Ctrl Pts',(54.4978292561259,-5.03673015697496,-3.36635267093772));
#67665=CARTESIAN_POINT('Ctrl Pts',(54.5983991660837,-2.81932673497138,-5.36212430946776));
#67666=CARTESIAN_POINT('Ctrl Pts',(54.6989690760415,0.0817505558831741,
-6.05757765920217));
#67667=CARTESIAN_POINT('Ctrl Pts',(54.7995389859993,2.96302383524132,-5.28408882816219));
#67668=CARTESIAN_POINT('Ctrl Pts',(54.9001088959571,5.12572640282613,-3.22918327964378));
#67669=CARTESIAN_POINT('Ctrl Pts',(55.000678805915,6.04552299830646,-0.391261761841782));
#67670=CARTESIAN_POINT('Ctrl Pts',(55.1012487158727,5.49913211454772,2.54165449878592));
#67671=CARTESIAN_POINT('Ctrl Pts',(55.2018186258305,3.6195084315661,4.85799622605417));
#67672=CARTESIAN_POINT('Ctrl Pts',(55.3023885357883,0.861545917421489,5.99674298766766));
#67673=CARTESIAN_POINT('Ctrl Pts',(55.3694351424269,-1.11543236559086,5.78565164753667));
#67674=CARTESIAN_POINT('Ctrl Pts',(55.4029584457461,-2.01944986373189,5.45072012049539));
#67675=CARTESIAN_POINT('Ctrl Pts',(18.7300198469368,-2.68895233313972,5.4170743448565));
#67676=CARTESIAN_POINT('Ctrl Pts',(18.7635431502561,-3.58738958330546,4.97110392129998));
#67677=CARTESIAN_POINT('Ctrl Pts',(18.8305897568946,-5.15720935627613,3.62400206174433));
#67678=CARTESIAN_POINT('Ctrl Pts',(18.9311596668524,-6.26143937167068,0.722616114702605));
#67679=CARTESIAN_POINT('Ctrl Pts',(19.0317295768102,-5.84719208744128,-2.35320906805725));
#67680=CARTESIAN_POINT('Ctrl Pts',(19.1322994867681,-4.01505030444853,-4.85877268109136));
#67681=CARTESIAN_POINT('Ctrl Pts',(19.2328693967258,-1.209239348121,-6.18589055396794));
#67682=CARTESIAN_POINT('Ctrl Pts',(19.3334393066836,1.88979937725391,-6.01303608743097));
#67683=CARTESIAN_POINT('Ctrl Pts',(19.4340092166414,4.53056937621935,-4.3819740585053));
#67684=CARTESIAN_POINT('Ctrl Pts',(19.5345791265992,6.0726771378643,-1.68831339839199));
#67685=CARTESIAN_POINT('Ctrl Pts',(19.635149036557,6.14216748646266,1.41477524815045));
#67686=CARTESIAN_POINT('Ctrl Pts',(19.7357189465149,4.72218670714282,4.17477524750178));
#67687=CARTESIAN_POINT('Ctrl Pts',(19.8362888564726,2.15708012498876,5.92239935194035));
#67688=CARTESIAN_POINT('Ctrl Pts',(19.9368587664304,-0.9311167393973,6.23384491889024));
#67689=CARTESIAN_POINT('Ctrl Pts',(20.0374286763883,-3.79351848932746,5.0335893753062));
#67690=CARTESIAN_POINT('Ctrl Pts',(20.137998586346,-5.7359953256746,2.61269227323296));
#67691=CARTESIAN_POINT('Ctrl Pts',(20.2385684963038,-6.28749820540378,-0.44178021687973));
#67692=CARTESIAN_POINT('Ctrl Pts',(20.3391384062616,-5.31428819701165,-3.38912150688244));
#67693=CARTESIAN_POINT('Ctrl Pts',(20.4397083162195,-3.052367868265,-5.51460368648902));
#67694=CARTESIAN_POINT('Ctrl Pts',(20.5402782261772,-0.0502509627448719,
-6.3027992511492));
#67695=CARTESIAN_POINT('Ctrl Pts',(20.6408481361351,2.96405175988155,-5.56257140673792));
#67696=CARTESIAN_POINT('Ctrl Pts',(20.7414180460928,5.25957448130762,-3.47342479294108));
#67697=CARTESIAN_POINT('Ctrl Pts',(20.8419879560507,6.27965491910467,-0.541975652624894));
#67698=CARTESIAN_POINT('Ctrl Pts',(20.9425578660084,5.7769244444727,2.52090211473068));
#67699=CARTESIAN_POINT('Ctrl Pts',(21.0431277759663,3.87329476512769,4.97246329043967));
#67700=CARTESIAN_POINT('Ctrl Pts',(21.1436976859241,1.03039443941634,6.21820639808852));
#67701=CARTESIAN_POINT('Ctrl Pts',(21.2442675958818,-2.06237565082662,5.95603980730125));
#67702=CARTESIAN_POINT('Ctrl Pts',(21.3448375058397,-4.65502142111349,4.24953869022517));
#67703=CARTESIAN_POINT('Ctrl Pts',(21.4454074157974,-6.11882850394745,1.51252809896995));
#67704=CARTESIAN_POINT('Ctrl Pts',(21.5459773257553,-6.09882494184173,-1.5912692542966));
#67705=CARTESIAN_POINT('Ctrl Pts',(21.6465472357131,-4.59986158138049,-4.30918518318667));
#67706=CARTESIAN_POINT('Ctrl Pts',(21.7471171456709,-1.98543574712842,-5.98212741463425));
#67707=CARTESIAN_POINT('Ctrl Pts',(21.8476870556287,1.11045654668285,-6.2044088976147));
#67708=CARTESIAN_POINT('Ctrl Pts',(21.9482569655865,3.93706408383606,-4.92212656385934));
#67709=CARTESIAN_POINT('Ctrl Pts',(22.0488268755443,5.80893696979688,-2.44623277547445));
#67710=CARTESIAN_POINT('Ctrl Pts',(22.1493967855021,6.27214764108139,0.622870355174984));
#67711=CARTESIAN_POINT('Ctrl Pts',(22.2499666954599,5.21436790864827,3.54092796087949));
#67712=CARTESIAN_POINT('Ctrl Pts',(22.3505366054177,2.89210844704538,5.60031358420288));
#67713=CARTESIAN_POINT('Ctrl Pts',(22.4511065153755,-0.131484823356128,
6.30162798426772));
#67714=CARTESIAN_POINT('Ctrl Pts',(22.5516764253333,-3.12319313727969,5.47480302276966));
#67715=CARTESIAN_POINT('Ctrl Pts',(22.6522463352911,-5.35752980394714,3.32034304111744));
#67716=CARTESIAN_POINT('Ctrl Pts',(22.7528162452489,-6.2926701050727,0.360702730240734));
#67717=CARTESIAN_POINT('Ctrl Pts',(22.8533861552067,-5.70184332262903,-2.68640768221608));
#67718=CARTESIAN_POINT('Ctrl Pts',(22.9539560651645,-3.72832444275807,-5.08206654427227));
#67719=CARTESIAN_POINT('Ctrl Pts',(23.0545259751223,-0.850690094966891,
-6.24532864413108));
#67720=CARTESIAN_POINT('Ctrl Pts',(23.1550958850801,2.23323586855536,-5.89410392394609));
#67721=CARTESIAN_POINT('Ctrl Pts',(23.2556657950379,4.77560405638639,-4.11356407601786));
#67722=CARTESIAN_POINT('Ctrl Pts',(23.3562357049957,6.15989237152066,-1.33548848072923));
#67723=CARTESIAN_POINT('Ctrl Pts',(23.4568056149535,6.05041208917317,1.76644192150945));
#67724=CARTESIAN_POINT('Ctrl Pts',(23.5573755249113,4.47371208356945,4.44001167838594));
#67725=CARTESIAN_POINT('Ctrl Pts',(23.6579454348691,1.81214074879979,6.03688242534326));
#67726=CARTESIAN_POINT('Ctrl Pts',(23.7585153448269,-1.2888731576111,6.16981438087633));
#67727=CARTESIAN_POINT('Ctrl Pts',(23.8590852547847,-4.07733643280026,4.80657166020007));
#67728=CARTESIAN_POINT('Ctrl Pts',(23.9596551647425,-5.87704913292351,2.27773944956002));
#67729=CARTESIAN_POINT('Ctrl Pts',(24.0602250747003,-6.25158247744522,-0.803442616854901));
#67730=CARTESIAN_POINT('Ctrl Pts',(24.1607949846581,-5.11011245272797,-3.68979054030895));
#67731=CARTESIAN_POINT('Ctrl Pts',(24.2613648946159,-2.72944455715552,-5.6813674340156));
#67732=CARTESIAN_POINT('Ctrl Pts',(24.3619348045737,0.313111293942983,-6.29521761565747));
#67733=CARTESIAN_POINT('Ctrl Pts',(24.4625047145315,3.2797379257955,-5.38248294460629));
#67734=CARTESIAN_POINT('Ctrl Pts',(24.5630746244893,5.45103093393507,-3.16450079288374));
#67735=CARTESIAN_POINT('Ctrl Pts',(24.6636445344471,6.30045363299915,-0.179129922979928));
#67736=CARTESIAN_POINT('Ctrl Pts',(24.7642144444049,5.62202174967209,2.84967979904634));
#67737=CARTESIAN_POINT('Ctrl Pts',(24.8647843543627,3.58025443164712,5.18744462288997));
#67738=CARTESIAN_POINT('Ctrl Pts',(24.9653542643205,0.670278495933398,6.26725859118388));
#67739=CARTESIAN_POINT('Ctrl Pts',(25.0659241742783,-2.4022393980492,5.82726774615162));
#67740=CARTESIAN_POINT('Ctrl Pts',(25.1664940842361,-4.89221630592146,3.9741694889568));
#67741=CARTESIAN_POINT('Ctrl Pts',(25.2670639941939,-6.19583497096784,1.15733855176901));
#67742=CARTESIAN_POINT('Ctrl Pts',(25.3676339041517,-5.99696898910696,-1.94014598795254));
#67743=CARTESIAN_POINT('Ctrl Pts',(25.4682038141095,-4.34384318975053,-4.5671467957289));
#67744=CARTESIAN_POINT('Ctrl Pts',(25.5687737240674,-1.63733915618441,-6.08661843707195));
#67745=CARTESIAN_POINT('Ctrl Pts',(25.6693436340251,1.46621821328794,-6.13009034696077));
#67746=CARTESIAN_POINT('Ctrl Pts',(25.769913543983,4.21421892820066,-4.68702062466917));
#67747=CARTESIAN_POINT('Ctrl Pts',(25.8704834539407,5.94027518074521,-2.10735243561707));
#67748=CARTESIAN_POINT('Ctrl Pts',(25.9710533638985,6.22581981551831,0.983346905002763));
#67749=CARTESIAN_POINT('Ctrl Pts',(26.0716232738563,5.00160850439243,3.83558546765264));
#67750=CARTESIAN_POINT('Ctrl Pts',(26.1721931838142,2.56451143647945,5.75769785617871));
#67751=CARTESIAN_POINT('Ctrl Pts',(26.2727630937719,-0.494477447174819,
6.2835734709729));
#67752=CARTESIAN_POINT('Ctrl Pts',(26.3733330037298,-3.43355597554957,5.28568792813638));
#67753=CARTESIAN_POINT('Ctrl Pts',(26.4739029136875,-5.54000013555698,3.00602761279857));
#67754=CARTESIAN_POINT('Ctrl Pts',(26.5744728236454,-6.30299903168285,-0.0025918109681364));
#67755=CARTESIAN_POINT('Ctrl Pts',(26.6750427336031,-5.53752608842792,-3.01058272280617));
#67756=CARTESIAN_POINT('Ctrl Pts',(26.775612643561,-3.42920783559051,-5.28850991595965));
#67757=CARTESIAN_POINT('Ctrl Pts',(26.8761825535188,-0.489309634582833,
-6.28397800699392));
#67758=CARTESIAN_POINT('Ctrl Pts',(26.9767524634765,2.5692457315994,-5.75558684076064));
#67759=CARTESIAN_POINT('Ctrl Pts',(27.0773223734344,5.0047612195492,-3.83147082021713));
#67760=CARTESIAN_POINT('Ctrl Pts',(27.1778922833922,6.22662642000029,-0.978226424010917));
#67761=CARTESIAN_POINT('Ctrl Pts',(27.27846219335,5.93854007365992,2.11223703793258));
#67762=CARTESIAN_POINT('Ctrl Pts',(27.3790321033077,4.2103628715226,4.69048483645164));
#67763=CARTESIAN_POINT('Ctrl Pts',(27.4796020132656,1.46117629744218,6.13129409983505));
#67764=CARTESIAN_POINT('Ctrl Pts',(27.5801719232234,-1.64234427094553,6.08526982200225));
#67765=CARTESIAN_POINT('Ctrl Pts',(27.6807418331812,-4.34759776740598,4.56357285070868));
#67766=CARTESIAN_POINT('Ctrl Pts',(27.781311743139,-5.99856254780733,1.93521339157265));
#67767=CARTESIAN_POINT('Ctrl Pts',(27.8818816530967,-6.19488107410007,-1.16243364913257));
#67768=CARTESIAN_POINT('Ctrl Pts',(27.9824515630546,-4.88894627265482,-3.97819153057936));
#67769=CARTESIAN_POINT('Ctrl Pts',(28.0830214730123,-2.39744620863596,-5.829241390402));
#67770=CARTESIAN_POINT('Ctrl Pts',(28.1835913829702,0.675432497186664,-6.26670523103035));
#67771=CARTESIAN_POINT('Ctrl Pts',(28.284161292928,3.58451940387321,-5.1844984476934));
#67772=CARTESIAN_POINT('Ctrl Pts',(28.3847312028858,5.6243634407776,-2.84505525375576));
#67773=CARTESIAN_POINT('Ctrl Pts',(28.4853011128436,6.30030418490677,0.18431139011253));
#67774=CARTESIAN_POINT('Ctrl Pts',(28.5858710228014,5.44842658767854,3.16898268053903));
#67775=CARTESIAN_POINT('Ctrl Pts',(28.6864409327592,3.27531023310016,5.38517839888599));
#67776=CARTESIAN_POINT('Ctrl Pts',(28.787010842717,0.307933966475966,6.2954729912191));
#67777=CARTESIAN_POINT('Ctrl Pts',(28.8875807526748,-2.73411602194027,5.6791208025053));
#67778=CARTESIAN_POINT('Ctrl Pts',(28.9881506626326,-5.11314522864148,3.685586707934));
#67779=CARTESIAN_POINT('Ctrl Pts',(29.0887205725904,-6.25224111893916,0.798301009347454));
#67780=CARTESIAN_POINT('Ctrl Pts',(29.1892904825482,-5.87517392000258,-2.28257199680546));
#67781=CARTESIAN_POINT('Ctrl Pts',(29.289860392506,-4.07338210298355,-4.80992325863648));
#67782=CARTESIAN_POINT('Ctrl Pts',(29.3904303024638,-1.28379863247516,-6.17087227076803));
#67783=CARTESIAN_POINT('Ctrl Pts',(29.4910002124216,1.81710490127779,-6.03539006930216));
#67784=CARTESIAN_POINT('Ctrl Pts',(29.5915701223794,4.47736206068688,-4.43633097146737));
#67785=CARTESIAN_POINT('Ctrl Pts',(29.6921400323372,6.05186277462106,-1.76146543197267));
#67786=CARTESIAN_POINT('Ctrl Pts',(29.792709942295,6.15879197532669,1.34055395845544));
#67787=CARTESIAN_POINT('Ctrl Pts',(29.8932798522528,4.77221942368032,4.11749016794541));
#67788=CARTESIAN_POINT('Ctrl Pts',(29.9938497622106,2.22838776985482,5.89593855616223));
#67789=CARTESIAN_POINT('Ctrl Pts',(30.0944196721684,-0.855825999900363,
6.24462691990268));
#67790=CARTESIAN_POINT('Ctrl Pts',(30.1949895821262,-3.73250270139929,5.07899863112071));
#67791=CARTESIAN_POINT('Ctrl Pts',(30.295559492084,-5.70405071085424,2.6817175464396));
#67792=CARTESIAN_POINT('Ctrl Pts',(30.3961294020418,-6.29237133313748,-0.365877734753705));
#67793=CARTESIAN_POINT('Ctrl Pts',(30.4966993119996,-5.35479732378858,-3.32474798022731));
#67794=CARTESIAN_POINT('Ctrl Pts',(30.5972692219574,-3.11868957298405,-5.47736970253418));
#67795=CARTESIAN_POINT('Ctrl Pts',(30.6978391319152,-0.12630228538831,-6.30173398705345));
#67796=CARTESIAN_POINT('Ctrl Pts',(30.798409041873,2.89671319768946,-5.59793320442559));
#67797=CARTESIAN_POINT('Ctrl Pts',(30.8989789518308,5.21727822390134,-3.53663843858597));
#67798=CARTESIAN_POINT('Ctrl Pts',(30.9995488617886,6.27265777199985,-0.61771189582904));
#67799=CARTESIAN_POINT('Ctrl Pts',(31.1001187717464,5.80692321007211,2.45100924992232));
#67800=CARTESIAN_POINT('Ctrl Pts',(31.2006886817042,3.9330147684679,4.92536276246656));
#67801=CARTESIAN_POINT('Ctrl Pts',(31.301258591662,1.10535363116214,6.20532004500618));
#67802=CARTESIAN_POINT('Ctrl Pts',(31.4018285016199,-1.99035481018033,5.98049255834927));
#67803=CARTESIAN_POINT('Ctrl Pts',(31.5023984115776,-4.60340392340859,4.30540077447214));
#67804=CARTESIAN_POINT('Ctrl Pts',(31.6029683215354,-6.10013154795234,1.58625300899802));
#67805=CARTESIAN_POINT('Ctrl Pts',(31.7035382314932,-6.11758252328589,-1.51755974566603));
#67806=CARTESIAN_POINT('Ctrl Pts',(31.804108141451,-4.65152500291308,-4.25336556836506));
#67807=CARTESIAN_POINT('Ctrl Pts',(31.9046780514089,-2.05747667349994,-5.95773390215462));
#67808=CARTESIAN_POINT('Ctrl Pts',(32.0052479613666,1.03550797810202,-6.21735689325986));
#67809=CARTESIAN_POINT('Ctrl Pts',(32.1058178713245,3.87738283640918,-4.9692761898287));
#67810=CARTESIAN_POINT('Ctrl Pts',(32.2063877812822,5.77899569464942,-2.51615028805955));
#67811=CARTESIAN_POINT('Ctrl Pts',(32.30695769124,6.27920707166246,0.547139892589688));
#67812=CARTESIAN_POINT('Ctrl Pts',(32.4075276011978,5.25671613911887,3.47774912027968));
#67813=CARTESIAN_POINT('Ctrl Pts',(32.5080975111557,2.95947606797094,5.56500718004803));
#67814=CARTESIAN_POINT('Ctrl Pts',(32.6086674211134,-0.0554344020580869,
6.3027557891725));
#67815=CARTESIAN_POINT('Ctrl Pts',(32.7092373310713,-3.05690207730752,5.51209154501553));
#67816=CARTESIAN_POINT('Ctrl Pts',(32.809807241029,-5.31707363027884,3.38474984615883));
#67817=CARTESIAN_POINT('Ctrl Pts',(32.9103771509868,-6.28785940499703,0.436609223298352));
#67818=CARTESIAN_POINT('Ctrl Pts',(33.0109470609447,-5.73384468677316,-2.61740876036626));
#67819=CARTESIAN_POINT('Ctrl Pts',(33.1115169709025,-3.78937756786474,-5.03670737278258));
#67820=CARTESIAN_POINT('Ctrl Pts',(33.2120868808602,-0.925989650754001,
-6.23460878304126));
#67821=CARTESIAN_POINT('Ctrl Pts',(33.3126567908181,2.16194995954613,-5.92062293034251));
#67822=CARTESIAN_POINT('Ctrl Pts',(33.4132267007759,4.72561856572486,-4.17089111367767));
#67823=CARTESIAN_POINT('Ctrl Pts',(33.5137966107337,6.14332873766329,-1.40972179236871));
#67824=CARTESIAN_POINT('Ctrl Pts',(33.6143665206914,6.07128697907194,1.69330385006073));
#67825=CARTESIAN_POINT('Ctrl Pts',(33.7149364306493,4.52696335439357,4.38570476649495));
#67826=CARTESIAN_POINT('Ctrl Pts',(33.8155063406071,1.88485501321466,6.01457605239459));
#67827=CARTESIAN_POINT('Ctrl Pts',(33.9160762505649,-1.21432904613156,6.18491782310809));
#67828=CARTESIAN_POINT('Ctrl Pts',(34.0166461605227,-4.01903935712015,4.8554223458725));
#67829=CARTESIAN_POINT('Ctrl Pts',(34.1172160704805,-5.84913608371143,2.34849112944965));
#67830=CARTESIAN_POINT('Ctrl Pts',(34.2177859804383,-6.2608223451068,-0.727947164216232));
#67831=CARTESIAN_POINT('Ctrl Pts',(34.3183558903961,-5.15426457730915,-3.62785889719748));
#67832=CARTESIAN_POINT('Ctrl Pts',(34.4189258003539,-2.79780208645283,-5.6480179705733));
#67833=CARTESIAN_POINT('Ctrl Pts',(34.5194957103117,0.237125001940042,-6.29853754806097));
#67834=CARTESIAN_POINT('Ctrl Pts',(34.6200656202695,3.21454948148645,-5.42166719210558));
#67835=CARTESIAN_POINT('Ctrl Pts',(34.7206355302273,5.41244847894878,-3.2300472091912));
#67836=CARTESIAN_POINT('Ctrl Pts',(34.8212054401851,6.29783337945691,-0.255143558565227));
#67837=CARTESIAN_POINT('Ctrl Pts',(34.9217753501429,5.6559991068023,2.78163218537792));
#67838=CARTESIAN_POINT('Ctrl Pts',(35.0223452601007,3.64258991959439,5.14386451887569));
#67839=CARTESIAN_POINT('Ctrl Pts',(35.1229151700585,0.745855812530698,6.2587141345322));
#67840=CARTESIAN_POINT('Ctrl Pts',(35.2234850800163,-2.33174768701761,5.85583096024525));
#67841=CARTESIAN_POINT('Ctrl Pts',(35.3240549899741,-4.84390437969943,4.03291381896607));
#67842=CARTESIAN_POINT('Ctrl Pts',(35.4246248999319,-6.18141843007595,1.23201854823549));
#67843=CARTESIAN_POINT('Ctrl Pts',(35.5251948098897,-6.01994383230129,-1.86764015988531));
#67844=CARTESIAN_POINT('Ctrl Pts',(35.6257647198475,-4.39863803733388,-4.51439773695212));
#67845=CARTESIAN_POINT('Ctrl Pts',(35.7263346298053,-1.71066630478676,-6.06641774893109));
#67846=CARTESIAN_POINT('Ctrl Pts',(35.8269045397631,1.39214053408053,-6.14733667894063));
#67847=CARTESIAN_POINT('Ctrl Pts',(35.9274744497209,4.15735449182779,-4.73753175611078));
#67848=CARTESIAN_POINT('Ctrl Pts',(36.0280443596787,5.91441356407679,-2.17887946062728));
#67849=CARTESIAN_POINT('Ctrl Pts',(36.1286142696366,6.23723243833396,0.908149228416427));
#67850=CARTESIAN_POINT('Ctrl Pts',(36.2291841795942,5.04752781548373,3.77495251133004));
#67851=CARTESIAN_POINT('Ctrl Pts',(36.3297540895522,2.63380204243537,5.72633305983351));
#67852=CARTESIAN_POINT('Ctrl Pts',(36.4303239995099,-0.418618458651225,
6.28908277071906));
#67853=CARTESIAN_POINT('Ctrl Pts',(36.5308939094677,-3.36952434387368,5.32673532352805));
#67854=CARTESIAN_POINT('Ctrl Pts',(36.6314638194255,-5.50332347628994,3.07265914578803));
#67855=CARTESIAN_POINT('Ctrl Pts',(36.7320337293833,-6.30257140312459,0.0734657702275063));
#67856=CARTESIAN_POINT('Ctrl Pts',(36.8326036393411,-5.57345119013571,-2.9435429913717));
#67857=CARTESIAN_POINT('Ctrl Pts',(36.9331735492989,-3.49277386132561,-5.24674511144952));
#67858=CARTESIAN_POINT('Ctrl Pts',(37.0337434592567,-0.565101877823921,
-6.27761605854952));
#67859=CARTESIAN_POINT('Ctrl Pts',(37.1343133692145,2.49960682459419,-5.78617051540318));
#67860=CARTESIAN_POINT('Ctrl Pts',(37.2348832791723,4.95816302378145,-3.89158360317305));
#67861=CARTESIAN_POINT('Ctrl Pts',(37.3354531891301,6.21436895783059,-1.05329101716025));
#67862=CARTESIAN_POINT('Ctrl Pts',(37.4360230990879,5.96359576911283,2.04042373381078));
#67863=CARTESIAN_POINT('Ctrl Pts',(37.5365930090457,4.26665574001952,4.63933748578796));
#67864=CARTESIAN_POINT('Ctrl Pts',(37.6371629190035,1.53505536683108,6.11321589113635));
#67865=CARTESIAN_POINT('Ctrl Pts',(37.7377328289614,-1.56879461139425,6.10464470531572));
#67866=CARTESIAN_POINT('Ctrl Pts',(37.8383027389191,-4.29221324681985,4.61570243350924));
#67867=CARTESIAN_POINT('Ctrl Pts',(37.938872648877,-5.97477386475187,2.00745629490579));
#67868=CARTESIAN_POINT('Ctrl Pts',(38.0394425588347,-6.20845696373824,-1.08759626713632));
#67869=CARTESIAN_POINT('Ctrl Pts',(38.1400124687925,-4.93659459343594,-3.91890767063194));
#67870=CARTESIAN_POINT('Ctrl Pts',(38.2405823787503,-2.46761228378761,-5.79988733750746));
#67871=CARTESIAN_POINT('Ctrl Pts',(38.3411522887081,0.599763880487827,-6.27439931774677));
#67872=CARTESIAN_POINT('Ctrl Pts',(38.4417221986659,3.52169782003892,-5.22737486461532));
#67873=CARTESIAN_POINT('Ctrl Pts',(38.5422921086238,5.58962306980901,-2.91271650668886));
#67874=CARTESIAN_POINT('Ctrl Pts',(38.6428620185815,6.30206953685826,0.108273096759718));
#67875=CARTESIAN_POINT('Ctrl Pts',(38.7434319285394,5.4862695662216,3.10300656744865));
#67876=CARTESIAN_POINT('Ctrl Pts',(38.8440018384971,3.34005394851439,5.34526361668836));
#67877=CARTESIAN_POINT('Ctrl Pts',(38.944571748455,0.38387812350663,6.29129884023737));
#67878=CARTESIAN_POINT('Ctrl Pts',(39.0451416584127,-2.6653878159982,5.71169951075923));
#67879=CARTESIAN_POINT('Ctrl Pts',(39.1457115683706,-5.06829950456569,3.74701796671673));
#67880=CARTESIAN_POINT('Ctrl Pts',(39.2462814783283,-6.24215292621357,0.873687791285975));
#67881=CARTESIAN_POINT('Ctrl Pts',(39.3468513882862,-5.90228963667894,-2.21151092143611));
#67882=CARTESIAN_POINT('Ctrl Pts',(39.447421298244,-4.13112619110987,-4.76042013944201));
#67883=CARTESIAN_POINT('Ctrl Pts',(39.5479912082017,-1.35816820038853,-6.15493157153938));
#67884=CARTESIAN_POINT('Ctrl Pts',(39.6485611181596,1.74414440977687,-6.05687739588006));
#67885=CARTESIAN_POINT('Ctrl Pts',(39.7491310281174,4.42350350198092,-4.49003566565361));
#67886=CARTESIAN_POINT('Ctrl Pts',(39.8497009380751,6.03016680283326,-1.8343641516576));
#67887=CARTESIAN_POINT('Ctrl Pts',(39.950270848033,6.17451984493906,1.26613909004208));
#67888=CARTESIAN_POINT('Ctrl Pts',(40.0508407579908,4.82155713985089,4.05960469233543));
#67889=CARTESIAN_POINT('Ctrl Pts',(40.1514106679486,2.29937097888354,5.86861965136154));
#67890=CARTESIAN_POINT('Ctrl Pts',(40.2519805779064,-0.780410665098583,
6.25449939680861));
#67891=CARTESIAN_POINT('Ctrl Pts',(40.3525504878642,-3.67094339459419,5.12366842258203));
#67892=CARTESIAN_POINT('Ctrl Pts',(40.453120397822,-5.67127551095404,2.75035226648001));
#67893=CARTESIAN_POINT('Ctrl Pts',(40.5536903077798,-6.29632819790416,-0.289921946661285));
#67894=CARTESIAN_POINT('Ctrl Pts',(40.6542602177376,-5.39452671692239,-3.25989033731036));
#67895=CARTESIAN_POINT('Ctrl Pts',(40.7548301276954,-3.18455715085024,-5.43933812736875));
#67896=CARTESIAN_POINT('Ctrl Pts',(40.8554000376532,-0.202335217055038,
-6.29975110387848));
#67897=CARTESIAN_POINT('Ctrl Pts',(40.955969947611,2.82895283270006,-5.63247986070409));
#67898=CARTESIAN_POINT('Ctrl Pts',(41.0565398575688,5.17422225576911,-3.59933709990915));
#67899=CARTESIAN_POINT('Ctrl Pts',(41.1571097675266,6.26474723593307,-0.693358190798846));
#67900=CARTESIAN_POINT('Ctrl Pts',(41.2576796774844,5.83607640425734,2.38075948271757));
#67901=CARTESIAN_POINT('Ctrl Pts',(41.3582495874421,3.99216206841114,4.87754503110101));
#67902=CARTESIAN_POINT('Ctrl Pts',(41.4588194974001,1.18015186754284,6.1915301081731));
#67903=CARTESIAN_POINT('Ctrl Pts',(41.5593894073578,-1.91804414529604,6.0040744638599));
#67904=CARTESIAN_POINT('Ctrl Pts',(41.6599593173156,-4.55111610400801,4.36063593054014));
#67905=CARTESIAN_POINT('Ctrl Pts',(41.7605292272734,-6.08054632522933,1.65974693782488));
#67906=CARTESIAN_POINT('Ctrl Pts',(41.8610991372312,-6.13544929689117,-1.44362925855516));
#67907=CARTESIAN_POINT('Ctrl Pts',(41.961669047189,-4.70251109562762,-4.19692660245303));
#67908=CARTESIAN_POINT('Ctrl Pts',(42.0622389571469,-2.12921800173078,-5.93247285809084));
#67909=CARTESIAN_POINT('Ctrl Pts',(42.1628088671045,0.96040862469385,-6.22939955248438));
#67910=CARTESIAN_POINT('Ctrl Pts',(42.2633787770625,3.81713698637752,-5.01570221784623));
#67911=CARTESIAN_POINT('Ctrl Pts',(42.3639486870201,5.74821291476561,-2.5857014130407));
#67912=CARTESIAN_POINT('Ctrl Pts',(42.4645185969781,6.28535215954959,0.471329758581282));
#67913=CARTESIAN_POINT('Ctrl Pts',(42.5650885069357,5.29829891625416,3.41406386948147));
#67914=CARTESIAN_POINT('Ctrl Pts',(42.6656584168937,3.02641274669477,5.52889043095649));
#67915=CARTESIAN_POINT('Ctrl Pts',(42.7662283268514,0.0206240912847744,
6.30296582235201));
#67916=CARTESIAN_POINT('Ctrl Pts',(42.8667982368092,-2.99016588850797,5.5485774276009));
#67917=CARTESIAN_POINT('Ctrl Pts',(42.967368146767,-5.2758432143581,3.44866378303112));
#67918=CARTESIAN_POINT('Ctrl Pts',(43.0679380567248,-6.2821331023235,0.512452139784996));
#67919=CARTESIAN_POINT('Ctrl Pts',(43.1685079666826,-5.76501112081578,-2.54802870622549));
#67920=CARTESIAN_POINT('Ctrl Pts',(43.2690778766404,-3.84987890519716,-4.99061478439249));
#67921=CARTESIAN_POINT('Ctrl Pts',(43.3696477865983,-1.00115436915438,-6.22298107340863));
#67922=CARTESIAN_POINT('Ctrl Pts',(43.470217696556,2.09034923958594,-5.94627980904374));
#67923=CARTESIAN_POINT('Ctrl Pts',(43.5707876065138,4.67494495715925,-4.22761080971396));
#67924=CARTESIAN_POINT('Ctrl Pts',(43.6713575164716,6.12587054694812,-1.48374982827714));
#67925=CARTESIAN_POINT('Ctrl Pts',(43.7719274264294,6.09127780242711,1.61991920926246));
#67926=CARTESIAN_POINT('Ctrl Pts',(43.8724973363872,4.57955543436417,4.33075923302884));
#67927=CARTESIAN_POINT('Ctrl Pts',(43.973067246345,1.95729481568055,5.99139387082747));
#67928=CARTESIAN_POINT('Ctrl Pts',(44.0736371563028,-1.13960811091008,6.19912065251409));
#67929=CARTESIAN_POINT('Ctrl Pts',(44.1742070662607,-3.96015705161237,4.9035660123469));
#67930=CARTESIAN_POINT('Ctrl Pts',(44.2747769762184,-5.82037131631542,2.41890083531584));
#67931=CARTESIAN_POINT('Ctrl Pts',(44.3753468861763,-6.26915054715452,-0.652345712020124));
#67932=CARTESIAN_POINT('Ctrl Pts',(44.475916796134,-5.19766616697324,-3.56539898574908));
#67933=CARTESIAN_POINT('Ctrl Pts',(44.5764867060918,-2.86575221560104,-5.61384607463161));
#67934=CARTESIAN_POINT('Ctrl Pts',(44.6770566160497,0.161104181132725,-6.30094032297563));
#67935=CARTESIAN_POINT('Ctrl Pts',(44.7776265260074,3.14889295262483,-5.46006196702825));
#67936=CARTESIAN_POINT('Ctrl Pts',(44.8781964359653,5.37307789376282,-3.29512328425448));
#67937=CARTESIAN_POINT('Ctrl Pts',(44.978766345923,6.29429607096292,-0.331120041585609));
#67938=CARTESIAN_POINT('Ctrl Pts',(45.0793362558809,5.68915286926505,2.71317952613023));
#67939=CARTESIAN_POINT('Ctrl Pts',(45.1799061658387,3.7043949941563,5.09953539434219));
#67940=CARTESIAN_POINT('Ctrl Pts',(45.2804760757965,0.821324521814106,6.24925831925242));
#67941=CARTESIAN_POINT('Ctrl Pts',(45.3810459857542,-2.26091644004823,5.88354148128475));
#67942=CARTESIAN_POINT('Ctrl Pts',(45.4816158957121,-4.79488711146061,4.09107089882682));
#67943=CARTESIAN_POINT('Ctrl Pts',(45.5821858056699,-6.16610178592019,1.30651914511453));
#67944=CARTESIAN_POINT('Ctrl Pts',(45.6827557156277,-6.04204208525136,-1.79486237659897));
#67945=CARTESIAN_POINT('Ctrl Pts',(45.7833256255854,-4.4527923800721,-4.46099131705619));
#67946=CARTESIAN_POINT('Ctrl Pts',(45.8838955355434,-1.78374435581676,-6.04533370327649));
#67947=CARTESIAN_POINT('Ctrl Pts',(45.984465445501,1.31786013922577,-6.16368787044887));
#67948=CARTESIAN_POINT('Ctrl Pts',(46.085035355459,4.09988468495787,-4.78735303491675));
#67949=CARTESIAN_POINT('Ctrl Pts',(46.1856052654166,5.88769072388608,-2.25008920950809));
#67950=CARTESIAN_POINT('Ctrl Pts',(46.2861751753745,6.24773683056493,0.832819312265029));
#67951=CARTESIAN_POINT('Ctrl Pts',(46.3867450853323,5.09271213406274,3.71376986772862));
#67952=CARTESIAN_POINT('Ctrl Pts',(46.4873149952901,2.70270912900301,5.69413442718755));
#67953=CARTESIAN_POINT('Ctrl Pts',(46.5878849052478,-0.342698513270351,
6.29367628972773));
#67954=CARTESIAN_POINT('Ctrl Pts',(46.6884548152057,-3.30500206108037,5.36700706978603));
#67955=CARTESIAN_POINT('Ctrl Pts',(46.7890247251635,-5.46584545411902,3.13884325549484));
#67956=CARTESIAN_POINT('Ctrl Pts',(46.8895946351213,-6.30122602969034,0.149512653752343));
#67957=CARTESIAN_POINT('Ctrl Pts',(46.990164545079,-5.60856471733773,-2.87607463782029));
#67958=CARTESIAN_POINT('Ctrl Pts',(47.0907344550369,-3.5558312890441,-5.20421630552899));
#67959=CARTESIAN_POINT('Ctrl Pts',(47.1913043649946,-0.640811834118883,
-6.27033999908552));
#67960=CARTESIAN_POINT('Ctrl Pts',(47.2918742749525,2.42960393895095,-5.8159116405524));
#67961=CARTESIAN_POINT('Ctrl Pts',(47.3924441849103,4.910842848298,-3.95112971568884));
#67962=CARTESIAN_POINT('Ctrl Pts',(47.4930140948681,6.20120659432713,-1.1282022360165));
#67963=CARTESIAN_POINT('Ctrl Pts',(47.5935840048259,5.9877830794084,1.96831331470099));
#67964=CARTESIAN_POINT('Ctrl Pts',(47.6941539147837,4.32232732218855,4.58751458098405));
#67965=CARTESIAN_POINT('Ctrl Pts',(47.7947238247415,1.60871091012128,6.09424751044258));
#67966=CARTESIAN_POINT('Ctrl Pts',(47.8952937346993,-1.49501651282591,6.12313066472181));
#67967=CARTESIAN_POINT('Ctrl Pts',(47.9958636446571,-4.23620371836591,4.6671599037725));
#67968=CARTESIAN_POINT('Ctrl Pts',(48.0964335546149,-5.95011516884782,2.07940688378343));
#67969=CARTESIAN_POINT('Ctrl Pts',(48.1970034645728,-6.22112881291391,-1.01260051551003));
#67970=CARTESIAN_POINT('Ctrl Pts',(48.2975733745305,-4.98352407517448,-3.85905316146789));
#67971=CARTESIAN_POINT('Ctrl Pts',(48.3981432844883,-2.53741903916567,-5.7696887377534));
#67972=CARTESIAN_POINT('Ctrl Pts',(48.4987131944461,0.524007929557735,-6.28117976184725));
#67973=CARTESIAN_POINT('Ctrl Pts',(48.5992831044039,3.45836342644444,-5.26949010071282));
#67974=CARTESIAN_POINT('Ctrl Pts',(48.6998530143616,5.55406876947679,-2.97995362628372));
#67975=CARTESIAN_POINT('Ctrl Pts',(48.8004229243196,6.30291721701269,0.0322190372896381));
#67976=CARTESIAN_POINT('Ctrl Pts',(48.9009928342773,5.52331366515492,3.03657861205532));
#67977=CARTESIAN_POINT('Ctrl Pts',(49.0015627442351,3.40431130412388,5.30457048737156));
#67978=CARTESIAN_POINT('Ctrl Pts',(49.1021326541929,0.459766382371591,6.28620858582657));
#67979=CARTESIAN_POINT('Ctrl Pts',(49.2027025641507,-2.59627149132571,5.74344651356729));
#67980=CARTESIAN_POINT('Ctrl Pts',(49.3032724741086,-5.02271576332149,3.80790360589141));
#67981=CARTESIAN_POINT('Ctrl Pts',(49.4038423840663,-6.23115578640957,0.948947351739475));
#67982=CARTESIAN_POINT('Ctrl Pts',(49.5044122940242,-5.92854589525094,-2.14012781832817));
#67983=CARTESIAN_POINT('Ctrl Pts',(49.6049822039819,-4.18826872795629,-4.71022383473465));
#67984=CARTESIAN_POINT('Ctrl Pts',(49.7055521139398,-1.43233999951405,-6.13809462591371));
#67985=CARTESIAN_POINT('Ctrl Pts',(49.8061220238974,1.67092994581097,-6.07748275415662));
#67986=CARTESIAN_POINT('Ctrl Pts',(49.9066919338554,4.36900081766127,-4.54308654618796));
#67987=CARTESIAN_POINT('Ctrl Pts',(50.0072618438131,6.00759275218989,-1.90699576158792));
#67988=CARTESIAN_POINT('Ctrl Pts',(50.107831753771,6.18934861582061,1.19153985360055));
#67989=CARTESIAN_POINT('Ctrl Pts',(50.2084016637287,4.87019276808361,4.00112808000257));
#67990=CARTESIAN_POINT('Ctrl Pts',(50.3089715736866,2.37001936648793,5.84044619128974));
#67991=CARTESIAN_POINT('Ctrl Pts',(50.4095414836443,-0.704881691300416,
6.26346112881276));
#67992=CARTESIAN_POINT('Ctrl Pts',(50.5101113936022,-3.6088495457308,5.16759213436563));
#67993=CARTESIAN_POINT('Ctrl Pts',(50.6106813035599,-5.63767449192264,2.81858649574634));
#67994=CARTESIAN_POINT('Ctrl Pts',(50.7112512135177,-6.29936822689513,-0.213923941771339));
#67995=CARTESIAN_POINT('Ctrl Pts',(50.8118211234756,-5.43347058952238,-3.19455800756135));
#67996=CARTESIAN_POINT('Ctrl Pts',(50.9123910334333,-3.24996101147774,-5.40051450648485));
#67997=CARTESIAN_POINT('Ctrl Pts',(51.0129609433911,-0.278338685809411,
-6.29685088650358));
#67998=CARTESIAN_POINT('Ctrl Pts',(51.113530853349,2.76078053156579,-5.66620634705498));
#67999=CARTESIAN_POINT('Ctrl Pts',(51.2141007633068,5.13041284659533,-3.66151164607849));
#68000=CARTESIAN_POINT('Ctrl Pts',(51.3146706732645,6.25592446273203,-0.768903522862193));
#68001=CARTESIAN_POINT('Ctrl Pts',(51.4152405832224,5.86437978193538,2.31016304275399));
#68002=CARTESIAN_POINT('Ctrl Pts',(51.5158104931801,4.05072805224571,4.8290170591569));
#68003=CARTESIAN_POINT('Ctrl Pts',(51.616380403138,1.25477825686932,6.17683859567069));
#68004=CARTESIAN_POINT('Ctrl Pts',(51.7169503130957,-1.84545418564875,6.02678208993408));
#68005=CARTESIAN_POINT('Ctrl Pts',(51.8175202230536,-4.49816557676692,4.41523611541536));
#68006=CARTESIAN_POINT('Ctrl Pts',(51.9180901330113,-6.06007568766899,1.73299918367025));
#68007=CARTESIAN_POINT('Ctrl Pts',(52.0186600429692,-6.15242266099837,-1.36948855829945));
#68008=CARTESIAN_POINT('Ctrl Pts',(52.1192299529269,-4.75281243521733,-4.13987650377665));
#68009=CARTESIAN_POINT('Ctrl Pts',(52.2197998628848,-2.20064928525366,-5.90634796081224));
#68010=CARTESIAN_POINT('Ctrl Pts',(52.3203697728425,0.885169422002587,-6.24053512170498));
#68011=CARTESIAN_POINT('Ctrl Pts',(52.4209396828005,3.75633530640134,-5.06139788761504));
#68012=CARTESIAN_POINT('Ctrl Pts',(52.5215095927581,5.71659311256105,-2.65487602277651));
#68013=CARTESIAN_POINT('Ctrl Pts',(52.6220795027161,6.29058200992785,0.395450992195018));
#68014=CARTESIAN_POINT('Ctrl Pts',(52.7226494126737,5.33911018500865,3.34988148196873));
#68015=CARTESIAN_POINT('Ctrl Pts',(52.8232193226317,3.09290873626811,5.49196859605096));
#68016=CARTESIAN_POINT('Ctrl Pts',(52.9237892325893,0.0966795814783073,
6.30225805321166));
#68017=CARTESIAN_POINT('Ctrl Pts',(53.0243591425472,-2.92299428865657,5.58425535767847));
#68018=CARTESIAN_POINT('Ctrl Pts',(53.1249290525049,-5.23384455986985,3.51207554490642));
#68019=CARTESIAN_POINT('Ctrl Pts',(53.2254989624628,-6.27549203099247,0.588220435964089));
#68020=CARTESIAN_POINT('Ctrl Pts',(53.3260688724206,-5.79533808626437,-2.47827762268341));
#68021=CARTESIAN_POINT('Ctrl Pts',(53.4266387823784,-3.90981964530785,-4.94379549053544));
#68022=CARTESIAN_POINT('Ctrl Pts',(53.5272086923362,-1.0761733042926,-6.21044720899938));
#68023=CARTESIAN_POINT('Ctrl Pts',(53.627778602294,2.01844413317511,-5.97107082285632));
#68024=CARTESIAN_POINT('Ctrl Pts',(53.7283485122517,4.62359061261052,-4.28371490724156));
#68025=CARTESIAN_POINT('Ctrl Pts',(53.8289184222097,6.10752033543931,-1.55756180437573));
#68026=CARTESIAN_POINT('Ctrl Pts',(53.9294883321674,6.11038166022464,1.54629867609741));
#68027=CARTESIAN_POINT('Ctrl Pts',(54.0300582421252,4.63148064195728,4.27518309621438));
#68028=CARTESIAN_POINT('Ctrl Pts',(54.130628152083,2.02944965364622,5.96733922230733));
#68029=CARTESIAN_POINT('Ctrl Pts',(54.2311980620408,-1.06472132187648,6.21242086748847));
#68030=CARTESIAN_POINT('Ctrl Pts',(54.3317679719986,-3.90069791524047,4.95099551900406));
#68031=CARTESIAN_POINT('Ctrl Pts',(54.4323378819564,-5.79075936208739,2.48895856933826));
#68032=CARTESIAN_POINT('Ctrl Pts',(54.5329077919142,-6.27656519998693,-0.576649767694941));
#68033=CARTESIAN_POINT('Ctrl Pts',(54.633477701872,-5.24031221488195,-3.50241892484281));
#68034=CARTESIAN_POINT('Ctrl Pts',(54.7340476118299,-2.93328248021272,-5.57885863266014));
#68035=CARTESIAN_POINT('Ctrl Pts',(54.8346175217876,0.085054871556865,-6.30242185123897));
#68036=CARTESIAN_POINT('Ctrl Pts',(54.9351874317455,3.0827877438102,-5.49766899709598));
#68037=CARTESIAN_POINT('Ctrl Pts',(55.0357573417032,5.33290564349095,-3.35970521688084));
#68038=CARTESIAN_POINT('Ctrl Pts',(55.1363272516611,6.28987994711282,-0.407076362222084));
#68039=CARTESIAN_POINT('Ctrl Pts',(55.2368971616187,5.72140422317592,2.64438687420114));
#68040=CARTESIAN_POINT('Ctrl Pts',(55.3374670715767,3.76580711188938,5.05435394985144));
#68041=CARTESIAN_POINT('Ctrl Pts',(55.4380369815344,0.896369162936647,6.23912827338287));
#68042=CARTESIAN_POINT('Ctrl Pts',(55.505083588173,-1.16051757154113,6.01950472920463));
#68043=CARTESIAN_POINT('Ctrl Pts',(55.5386068914922,-2.10107499477635,5.67103544107472));
#68044=CARTESIAN_POINT('Ctrl Pts',(18.8656682926829,-2.79341604200804,5.62752347417158));
#68045=CARTESIAN_POINT('Ctrl Pts',(18.8991915960022,-3.72675688127093,5.16422744617198));
#68046=CARTESIAN_POINT('Ctrl Pts',(18.9662382026407,-5.35756293269594,3.76479172604979));
#68047=CARTESIAN_POINT('Ctrl Pts',(19.0668081125985,-6.50469142621899,0.75068918929729));
#68048=CARTESIAN_POINT('Ctrl Pts',(19.1673780225563,-6.07435095686098,-2.44462941194441));
#68049=CARTESIAN_POINT('Ctrl Pts',(19.2679479325142,-4.17103188914465,-5.04753222456091));
#68050=CARTESIAN_POINT('Ctrl Pts',(19.3685178424719,-1.2562173572353,-6.42620759564877));
#68051=CARTESIAN_POINT('Ctrl Pts',(19.4690877524297,1.9632166147155,-6.24663786739205));
#68052=CARTESIAN_POINT('Ctrl Pts',(19.5696576623875,4.70657847630348,-4.55221034595246));
#68053=CARTESIAN_POINT('Ctrl Pts',(19.6702275723453,6.30859592629457,-1.75390306212622));
#68054=CARTESIAN_POINT('Ctrl Pts',(19.7707974823031,6.38078592094303,1.46973816728273));
#68055=CARTESIAN_POINT('Ctrl Pts',(19.8713673922609,4.90563999164961,4.33696202213174));
#68056=CARTESIAN_POINT('Ctrl Pts',(19.9719373022188,2.24088101182681,6.15247996515098));
#68057=CARTESIAN_POINT('Ctrl Pts',(20.0725072121765,-0.967289901259671,
6.47602495038849));
#68058=CARTESIAN_POINT('Ctrl Pts',(20.1730771221343,-3.94089373513293,5.22914041151611));
#68059=CARTESIAN_POINT('Ctrl Pts',(20.2736470320921,-5.95883428729783,2.71419333802675));
#68060=CARTESIAN_POINT('Ctrl Pts',(20.3742169420499,-6.53176262539532,-0.458943035049169));
#68061=CARTESIAN_POINT('Ctrl Pts',(20.4747868520077,-5.52074416434619,-3.52078624413008));
#68062=CARTESIAN_POINT('Ctrl Pts',(20.5753567619656,-3.17094998830467,-5.72884175494776));
#68063=CARTESIAN_POINT('Ctrl Pts',(20.6759266719233,-0.0522031736032762,
-6.54765810487926));
#68064=CARTESIAN_POINT('Ctrl Pts',(20.7764965818812,3.07920286773082,-5.77867298385814));
#68065=CARTESIAN_POINT('Ctrl Pts',(20.8770664918389,5.46390486329879,-3.60836464734974));
#68066=CARTESIAN_POINT('Ctrl Pts',(20.9776364017968,6.52361463351761,-0.563030985622693));
#68067=CARTESIAN_POINT('Ctrl Pts',(21.0782063117546,6.00135347055993,2.61883720318622));
#68068=CARTESIAN_POINT('Ctrl Pts',(21.1787762217123,4.02376925726304,5.16563962574656));
#68069=CARTESIAN_POINT('Ctrl Pts',(21.2793461316702,1.07042446278717,6.45977888520451));
#68070=CARTESIAN_POINT('Ctrl Pts',(21.3799160416279,-2.14249734242742,6.18742732606452));
#68071=CARTESIAN_POINT('Ctrl Pts',(21.4804859515858,-4.83586538644446,4.41462996651488));
#68072=CARTESIAN_POINT('Ctrl Pts',(21.5810558615435,-6.35654023709114,1.57128864040408));
#68073=CARTESIAN_POINT('Ctrl Pts',(21.6816257715014,-6.33575955214008,-1.65308882843456));
#68074=CARTESIAN_POINT('Ctrl Pts',(21.7821956814592,-4.77856262979613,-4.47659367938356));
#68075=CARTESIAN_POINT('Ctrl Pts',(21.882765591417,-2.06256838325162,-6.21452841667276));
#68076=CARTESIAN_POINT('Ctrl Pts',(21.9833355013748,1.15359692071403,-6.44544536255773));
#68077=CARTESIAN_POINT('Ctrl Pts',(22.0839054113326,4.0900159644555,-5.11334735644941));
#68078=CARTESIAN_POINT('Ctrl Pts',(22.1844753212904,6.03460965761974,-2.54126701811676));
#68079=CARTESIAN_POINT('Ctrl Pts',(22.2850452312482,6.51581570357615,0.647068384512964));
#68080=CARTESIAN_POINT('Ctrl Pts',(22.385615141206,5.41694205041641,3.67849026091368));
#68081=CARTESIAN_POINT('Ctrl Pts',(22.4861850511638,3.00446461308975,5.81788141559254));
#68082=CARTESIAN_POINT('Ctrl Pts',(22.5867549611216,-0.136592906581867,
6.5464413351895));
#68083=CARTESIAN_POINT('Ctrl Pts',(22.6873248710794,-3.24452676399049,5.68749486636738));
#68084=CARTESIAN_POINT('Ctrl Pts',(22.7878947810372,-5.5656656741131,3.44933578840989));
#68085=CARTESIAN_POINT('Ctrl Pts',(22.888464690995,-6.53713544934789,0.374715751050151));
#68086=CARTESIAN_POINT('Ctrl Pts',(22.9890346009528,-5.9233555054695,-2.79077253337317));
#68087=CARTESIAN_POINT('Ctrl Pts',(23.0896045109106,-3.87316695050906,-5.27950088083053));
#68088=CARTESIAN_POINT('Ctrl Pts',(23.1901744208684,-0.883738744183345,
-6.48795480943227));
#68089=CARTESIAN_POINT('Ctrl Pts',(23.2907443308262,2.31999534685918,-6.12308528176423));
#68090=CARTESIAN_POINT('Ctrl Pts',(23.391314240784,4.96113256340688,-4.27337284419578));
#68091=CARTESIAN_POINT('Ctrl Pts',(23.4918841507418,6.39919940401359,-1.38737117055174));
#68092=CARTESIAN_POINT('Ctrl Pts',(23.5924540606996,6.28546589776137,1.83506681766218));
#68093=CARTESIAN_POINT('Ctrl Pts',(23.6930239706574,4.64751232201134,4.61250268227118));
#68094=CARTESIAN_POINT('Ctrl Pts',(23.7935938806152,1.88254100888544,6.27141061700401));
#68095=CARTESIAN_POINT('Ctrl Pts',(23.894163790573,-1.33894487834989,6.40950687572348));
#68096=CARTESIAN_POINT('Ctrl Pts',(23.9947337005308,-4.23573778518752,4.99330323456734));
#68097=CARTESIAN_POINT('Ctrl Pts',(24.0953036104886,-6.10536792536175,2.36622785740725));
#68098=CARTESIAN_POINT('Ctrl Pts',(24.1958735204464,-6.49445159931153,-0.834655738257308));
#68099=CARTESIAN_POINT('Ctrl Pts',(24.2964434304042,-5.30863635103847,-3.83313603589005));
#68100=CARTESIAN_POINT('Ctrl Pts',(24.397013340362,-2.83548135746499,-5.90208414449291));
#68101=CARTESIAN_POINT('Ctrl Pts',(24.4975832503198,0.325275424430082,-6.53978192873951));
#68102=CARTESIAN_POINT('Ctrl Pts',(24.5981531602776,3.40715319590727,-5.59158822489862));
#68103=CARTESIAN_POINT('Ctrl Pts',(24.6987230702354,5.66279925035214,-3.28743918991932));
#68104=CARTESIAN_POINT('Ctrl Pts',(24.7992929801932,6.54522136128659,-0.186088981306509));
#68105=CARTESIAN_POINT('Ctrl Pts',(24.899862890151,5.84043292642331,2.96038764508239));
#68106=CARTESIAN_POINT('Ctrl Pts',(25.0004328001088,3.71934453451454,5.3889728159254));
#68107=CARTESIAN_POINT('Ctrl Pts',(25.1010027100666,0.696318294704414,6.51073671788884));
#68108=CARTESIAN_POINT('Ctrl Pts',(25.2015726200244,-2.49556453216075,6.05365257039312));
#68109=CARTESIAN_POINT('Ctrl Pts',(25.3021425299822,-5.08227510823047,4.12856288573482));
#68110=CARTESIAN_POINT('Ctrl Pts',(25.40271243994,-6.43653834552245,1.20230025527115));
#68111=CARTESIAN_POINT('Ctrl Pts',(25.5032823498979,-6.22994657478204,-2.01551915212123));
#68112=CARTESIAN_POINT('Ctrl Pts',(25.6038522598556,-4.51259812257367,-4.7445769001409));
#68113=CARTESIAN_POINT('Ctrl Pts',(25.7044221698134,-1.70094851021507,-6.32307883414425));
#68114=CARTESIAN_POINT('Ctrl Pts',(25.8049920797713,1.52317965164543,-6.36823959395525));
#68115=CARTESIAN_POINT('Ctrl Pts',(25.905561989729,4.37793805917866,-4.86910773419536));
#68116=CARTESIAN_POINT('Ctrl Pts',(26.0061318996868,6.17105025601567,-2.18922144036068));
#68117=CARTESIAN_POINT('Ctrl Pts',(26.1067018096447,6.46768807798595,1.02154916821688));
#68118=CARTESIAN_POINT('Ctrl Pts',(26.2072717196024,5.19591710861598,3.98459498288065));
#68119=CARTESIAN_POINT('Ctrl Pts',(26.3078416295603,2.66414071320113,5.98137994424951));
#68120=CARTESIAN_POINT('Ctrl Pts',(26.408411539518,-0.513687511796294,6.52768541808125));
#68121=CARTESIAN_POINT('Ctrl Pts',(26.5089814494759,-3.56694695738004,5.49103279724709));
#68122=CARTESIAN_POINT('Ctrl Pts',(26.6095513594336,-5.75522483632937,3.12280944991903));
#68123=CARTESIAN_POINT('Ctrl Pts',(26.7101212693915,-6.54786564673141,-0.00269250081047194));
#68124=CARTESIAN_POINT('Ctrl Pts',(26.8106911793493,-5.75265467439162,-3.12754152241121));
#68125=CARTESIAN_POINT('Ctrl Pts',(26.911261089307,-3.56242989556197,-5.49396441710467));
#68126=CARTESIAN_POINT('Ctrl Pts',(27.0118309992649,-0.508318933700379,
-6.52810567001237));
#68127=CARTESIAN_POINT('Ctrl Pts',(27.1124009092226,2.66905893200806,-5.97918691752266));
#68128=CARTESIAN_POINT('Ctrl Pts',(27.2129708191805,5.199192304307,-3.98032048458925));
#68129=CARTESIAN_POINT('Ctrl Pts',(27.3135407291383,6.46852601842535,-1.01622976051699));
#68130=CARTESIAN_POINT('Ctrl Pts',(27.414110639096,6.16924774136823,2.19429580568093));
#68131=CARTESIAN_POINT('Ctrl Pts',(27.5146805490539,4.37393219769472,4.87270652791397));
#68132=CARTESIAN_POINT('Ctrl Pts',(27.6152504590117,1.5179418612865,6.36949011169342));
#68133=CARTESIAN_POINT('Ctrl Pts',(27.7158203689695,-1.70614806979581,6.32167782642693));
#68134=CARTESIAN_POINT('Ctrl Pts',(27.8163902789273,-4.51649856265382,4.74086411013352));
#68135=CARTESIAN_POINT('Ctrl Pts',(27.9169601888851,-6.23160204199977,2.01039492820449));
#68136=CARTESIAN_POINT('Ctrl Pts',(28.0175300988428,-6.43554739050252,-1.20759329320851));
#68137=CARTESIAN_POINT('Ctrl Pts',(28.1181000088007,-5.07887803671217,-4.13274118054939));
#68138=CARTESIAN_POINT('Ctrl Pts',(28.2186699187585,-2.490585131063,-6.05570288918915));
#68139=CARTESIAN_POINT('Ctrl Pts',(28.3192398287163,0.701672524901834,-6.51016186012329));
#68140=CARTESIAN_POINT('Ctrl Pts',(28.4198097386741,3.72377519759783,-5.38591218411155));
#68141=CARTESIAN_POINT('Ctrl Pts',(28.5203796486319,5.84286559040883,-2.95558343980043));
#68142=CARTESIAN_POINT('Ctrl Pts',(28.6209495585897,6.54506610725194,0.191471744411332));
#68143=CARTESIAN_POINT('Ctrl Pts',(28.7215194685475,5.66009372726706,3.29209519542769));
#68144=CARTESIAN_POINT('Ctrl Pts',(28.8220893785053,3.40255349079092,5.59438839548278));
#68145=CARTESIAN_POINT('Ctrl Pts',(28.9226592884631,0.319896961813634,6.54004722544329));
#68146=CARTESIAN_POINT('Ctrl Pts',(29.0232291984209,-2.84033430502701,5.899750233094));
#68147=CARTESIAN_POINT('Ctrl Pts',(29.1237991083787,-5.31178694793982,3.82876888789362));
#68148=CARTESIAN_POINT('Ctrl Pts',(29.2243690183365,-6.49513582851576,0.829314383293102));
#68149=CARTESIAN_POINT('Ctrl Pts',(29.3249389282943,-6.10341986187583,-2.3712481453584));
#68150=CARTESIAN_POINT('Ctrl Pts',(29.4255088382521,-4.23162983272986,-4.99678503999889));
#68151=CARTESIAN_POINT('Ctrl Pts',(29.5260787482099,-1.33367321185521,-6.41060586381551));
#68152=CARTESIAN_POINT('Ctrl Pts',(29.6266486581677,1.88769801483017,-6.26986028409025));
#68153=CARTESIAN_POINT('Ctrl Pts',(29.7272185681255,4.65130409790384,-4.60867898274863));
#68154=CARTESIAN_POINT('Ctrl Pts',(29.8277884780834,6.28697294121176,-1.82989699537353));
#68155=CARTESIAN_POINT('Ctrl Pts',(29.9283583880411,6.39805625828247,1.39263343815186));
#68156=CARTESIAN_POINT('Ctrl Pts',(30.028928297999,4.95761644034995,4.27745146174423));
#68157=CARTESIAN_POINT('Ctrl Pts',(30.1294982079567,2.314958903291,6.1249911880165));
#68158=CARTESIAN_POINT('Ctrl Pts',(30.2300681179145,-0.88907417503301,6.48722582376283));
#68159=CARTESIAN_POINT('Ctrl Pts',(30.3306380278723,-3.87750753125207,5.27631378163672));
#68160=CARTESIAN_POINT('Ctrl Pts',(30.4312079378301,-5.92564864901217,2.78590018946591));
#68161=CARTESIAN_POINT('Ctrl Pts',(30.5317778477879,-6.53682507035513,-0.380091800467598));
#68162=CARTESIAN_POINT('Ctrl Pts',(30.6323477577457,-5.56282703922345,-3.45391185598164));
#68163=CARTESIAN_POINT('Ctrl Pts',(30.7329176677035,-3.23984823972113,-5.69016125964651));
#68164=CARTESIAN_POINT('Ctrl Pts',(30.8334875776613,-0.131209031040714,
-6.54655145610109));
#68165=CARTESIAN_POINT('Ctrl Pts',(30.9340574876191,3.00924825471858,-5.81540855991041));
#68166=CARTESIAN_POINT('Ctrl Pts',(31.034627397577,5.41996542915581,-3.67403409401191));
#68167=CARTESIAN_POINT('Ctrl Pts',(31.1351973075347,6.51634565268443,-0.641709523029432));
#68168=CARTESIAN_POINT('Ctrl Pts',(31.2357672174926,6.03251766489431,2.54622905488571));
#68169=CARTESIAN_POINT('Ctrl Pts',(31.3363371274503,4.0858093363315,5.11670927885807));
#68170=CARTESIAN_POINT('Ctrl Pts',(31.4369070374082,1.14829576089017,6.44639190731743));
#68171=CARTESIAN_POINT('Ctrl Pts',(31.5374769473659,-2.0676785480811,6.21283004749135));
#68172=CARTESIAN_POINT('Ctrl Pts',(31.6380468573237,-4.78224258905971,4.47266224933087));
#68173=CARTESIAN_POINT('Ctrl Pts',(31.7386167672815,-6.33711691888288,1.64787770590364));
#68174=CARTESIAN_POINT('Ctrl Pts',(31.8391866772393,-6.35524585104898,-1.57651576266484));
#68175=CARTESIAN_POINT('Ctrl Pts',(31.9397565871971,-4.83223313511359,-4.4186055158971));
#68176=CARTESIAN_POINT('Ctrl Pts',(32.040326497155,-2.13740804363799,-6.18918723518668));
#68177=CARTESIAN_POINT('Ctrl Pts',(32.1408964071127,1.07573665847769,-6.45889637777332));
#68178=CARTESIAN_POINT('Ctrl Pts',(32.2414663170705,4.02801614693748,-5.16232870875315));
#68179=CARTESIAN_POINT('Ctrl Pts',(32.3420362270284,6.0035051871967,-2.61390077174097));
#68180=CARTESIAN_POINT('Ctrl Pts',(32.4426061369861,6.52314938755023,0.568395852297626));
#68181=CARTESIAN_POINT('Ctrl Pts',(32.543176046944,5.46093547673687,3.61285697144554));
#68182=CARTESIAN_POINT('Ctrl Pts',(32.6437459569018,3.07444941374469,5.78120338506881));
#68183=CARTESIAN_POINT('Ctrl Pts',(32.7443158668595,-0.0575879855063994,
6.54761295443854));
#68184=CARTESIAN_POINT('Ctrl Pts',(32.8448857768174,-3.17566034784553,5.72623201872991));
#68185=CARTESIAN_POINT('Ctrl Pts',(32.9454556867752,-5.5236378095316,3.51624474778404));
#68186=CARTESIAN_POINT('Ctrl Pts',(33.0460255967329,-6.53213785731212,0.453571152384891));
#68187=CARTESIAN_POINT('Ctrl Pts',(33.1465955066908,-5.95660009774608,-2.71909305702058));
#68188=CARTESIAN_POINT('Ctrl Pts',(33.2471654166485,-3.93659194208878,-5.23237954077183));
#68189=CARTESIAN_POINT('Ctrl Pts',(33.3477353266064,-0.961963629206205,
-6.47681849006828));
#68190=CARTESIAN_POINT('Ctrl Pts',(33.4483052365642,2.245940035673,-6.15063453095429));
#68191=CARTESIAN_POINT('Ctrl Pts',(33.548875146522,4.90920517527109,-4.33292699272645));
#68192=CARTESIAN_POINT('Ctrl Pts',(33.6494450564797,6.38199228585055,-1.46448838867028));
#68193=CARTESIAN_POINT('Ctrl Pts',(33.7500149664376,6.30715176091324,1.75908738896483));
#68194=CARTESIAN_POINT('Ctrl Pts',(33.8505848763953,4.70283236333157,4.55608598904884));
#68195=CARTESIAN_POINT('Ctrl Pts',(33.9511547863532,1.95808016597497,6.24823765879799));
#68196=CARTESIAN_POINT('Ctrl Pts',(34.051724696311,-1.261504786059,6.42519707495081));
#68197=CARTESIAN_POINT('Ctrl Pts',(34.1522946062687,-4.17517591341315,5.04405173142193));
#68198=CARTESIAN_POINT('Ctrl Pts',(34.2528645162266,-6.07637047587579,2.43972818508764));
#68199=CARTESIAN_POINT('Ctrl Pts',(34.3534344261843,-6.50405042865251,-0.756227345942419));
#68200=CARTESIAN_POINT('Ctrl Pts',(34.4540043361422,-5.35450375135413,-3.76879839656363));
#68201=CARTESIAN_POINT('Ctrl Pts',(34.5545742461,-2.90649452366275,-5.8674390803079));
#68202=CARTESIAN_POINT('Ctrl Pts',(34.6551441560578,0.246337124022986,-6.54323083793734));
#68203=CARTESIAN_POINT('Ctrl Pts',(34.7557140660156,3.33943223118723,-5.63229474996771));
#68204=CARTESIAN_POINT('Ctrl Pts',(34.8562839759734,5.62271789696759,-3.35553203357178));
#68205=CARTESIAN_POINT('Ctrl Pts',(34.9568538859312,6.54249931293014,-0.265055687572883));
#68206=CARTESIAN_POINT('Ctrl Pts',(35.057423795889,5.87573027747814,2.88969643449489));
#68207=CARTESIAN_POINT('Ctrl Pts',(35.1579937058468,3.78410170773486,5.34369965873123));
#68208=CARTESIAN_POINT('Ctrl Pts',(35.2585636158046,0.774831731329118,6.50186031573515));
#68209=CARTESIAN_POINT('Ctrl Pts',(35.3591335257624,-2.42233427292655,6.08332544316112));
#68210=CARTESIAN_POINT('Ctrl Pts',(35.4597034357202,-5.03208630121234,4.18958938732152));
#68211=CARTESIAN_POINT('Ctrl Pts',(35.560273345678,-6.42156173321834,1.27988151157515));
#68212=CARTESIAN_POINT('Ctrl Pts',(35.6608432556358,-6.25381397278339,-1.94019652896949));
#68213=CARTESIAN_POINT('Ctrl Pts',(35.7614131655936,-4.56952170741089,-4.68977858141583));
#68214=CARTESIAN_POINT('Ctrl Pts',(35.8619830755514,-1.77712436156657,-6.30209336496475));
#68215=CARTESIAN_POINT('Ctrl Pts',(35.9625529855092,1.44622411215802,-6.38615593253239));
#68216=CARTESIAN_POINT('Ctrl Pts',(36.063122895467,4.31886448363548,-4.92158118384713));
#68217=CARTESIAN_POINT('Ctrl Pts',(36.1636928054248,6.14418393563375,-2.26352723471714));
#68218=CARTESIAN_POINT('Ctrl Pts',(36.2642627153826,6.47954407233056,0.943430120322585));
#68219=CARTESIAN_POINT('Ctrl Pts',(36.3648326253404,5.24362034926458,3.92160648331579));
#68220=CARTESIAN_POINT('Ctrl Pts',(36.4654025352982,2.73612320536071,5.94879664993625));
#68221=CARTESIAN_POINT('Ctrl Pts',(36.565972445256,-0.434881460509812,6.5334087498419));
#68222=CARTESIAN_POINT('Ctrl Pts',(36.6665423552139,-3.50042774656513,5.53367485205654));
#68223=CARTESIAN_POINT('Ctrl Pts',(36.7671122651716,-5.717123317347,3.19202956619347));
#68224=CARTESIAN_POINT('Ctrl Pts',(36.8676821751294,-6.54742140513593,0.0763198583190625));
#68225=CARTESIAN_POINT('Ctrl Pts',(36.9682520850872,-5.78997543838753,-3.05789734949935));
#68226=CARTESIAN_POINT('Ctrl Pts',(37.068821995045,-3.62846541200707,-5.45057708238993));
#68227=CARTESIAN_POINT('Ctrl Pts',(37.1693919050029,-0.587055646701985,
-6.52149656481404));
#68228=CARTESIAN_POINT('Ctrl Pts',(37.2699618149606,2.59671460757404,-6.010958744162));
#68229=CARTESIAN_POINT('Ctrl Pts',(37.3705317249185,5.15078380483974,-4.04276860245633));
#68230=CARTESIAN_POINT('Ctrl Pts',(37.4711016348762,6.45579236337419,-1.09421055478614));
#68231=CARTESIAN_POINT('Ctrl Pts',(37.5716715448341,6.19527683112161,2.1196926104918));
#68232=CARTESIAN_POINT('Ctrl Pts',(37.6722414547918,4.43241200039406,4.81957214241771));
#68233=CARTESIAN_POINT('Ctrl Pts',(37.7728113647496,1.59469107511828,6.35070957863325));
#68234=CARTESIAN_POINT('Ctrl Pts',(37.8733812747074,-1.6297410631179,6.34180540890317));
#68235=CARTESIAN_POINT('Ctrl Pts',(37.9739511846652,-4.45896239647582,4.79501888672199));
#68236=CARTESIAN_POINT('Ctrl Pts',(38.0745210946231,-6.20688918709104,2.08544441220052));
#68237=CARTESIAN_POINT('Ctrl Pts',(38.1750910045808,-6.44965069290488,-1.12984853706919));
#68238=CARTESIAN_POINT('Ctrl Pts',(38.2756609145387,-5.12837745773363,-4.07115418870565));
#68239=CARTESIAN_POINT('Ctrl Pts',(38.3762308244964,-2.56347710371634,-6.0252084541473));
#68240=CARTESIAN_POINT('Ctrl Pts',(38.4768007344543,0.623064241237588,-6.51815485613047));
#68241=CARTESIAN_POINT('Ctrl Pts',(38.577370644412,3.65851304404296,-5.43045431651657));
#68242=CARTESIAN_POINT('Ctrl Pts',(38.6779405543699,5.80677558302084,-3.02587327983824));
#68243=CARTESIAN_POINT('Ctrl Pts',(38.7785104643276,6.54690004175509,0.112479422442342));
#68244=CARTESIAN_POINT('Ctrl Pts',(38.8790803742854,5.69940687612311,3.22355596160616));
#68245=CARTESIAN_POINT('Ctrl Pts',(38.9796502842433,3.46981244924414,5.55292295500994));
#68246=CARTESIAN_POINT('Ctrl Pts',(39.080220194201,0.398791490337503,6.53571091193916));
#68247=CARTESIAN_POINT('Ctrl Pts',(39.1807901041589,-2.76893606168483,5.93359459885046));
#68248=CARTESIAN_POINT('Ctrl Pts',(39.2813600141166,-5.26519900232813,3.89258670334893));
#68249=CARTESIAN_POINT('Ctrl Pts',(39.3819299240745,-6.48465571734115,0.907629883135581));
#68250=CARTESIAN_POINT('Ctrl Pts',(39.4824998340322,-6.13158900307658,-2.29742640242431));
#68251=CARTESIAN_POINT('Ctrl Pts',(39.5830697439901,-4.29161723381362,-4.94535876308686));
#68252=CARTESIAN_POINT('Ctrl Pts',(39.6836396539478,-1.41093197969802,-6.39404588080751));
#68253=CARTESIAN_POINT('Ctrl Pts',(39.7842095639057,1.81190306492362,-6.29218237661038));
#68254=CARTESIAN_POINT('Ctrl Pts',(39.8847794738634,4.59535317603941,-4.66447006257631));
#68255=CARTESIAN_POINT('Ctrl Pts',(39.9853493838213,6.26443409777744,-1.90562777367704));
#68256=CARTESIAN_POINT('Ctrl Pts',(40.0859192937791,6.41439514340897,1.31532760991984));
#68257=CARTESIAN_POINT('Ctrl Pts',(40.1864892037369,5.00887088845912,4.21731718038291));
#68258=CARTESIAN_POINT('Ctrl Pts',(40.2870591136947,2.38869975483763,6.09661096499068));
#68259=CARTESIAN_POINT('Ctrl Pts',(40.3876290236525,-0.810729013070725,
6.49748183872578));
#68260=CARTESIAN_POINT('Ctrl Pts',(40.4881989336103,-3.81355669320821,5.32271895978858));
#68261=CARTESIAN_POINT('Ctrl Pts',(40.588768843568,-5.89160015806168,2.85720131505177));
#68262=CARTESIAN_POINT('Ctrl Pts',(40.6893387535259,-6.54093565624356,-0.301185189024252));
#68263=CARTESIAN_POINT('Ctrl Pts',(40.7899086634837,-5.60409988841139,-3.38653454403075));
#68264=CARTESIAN_POINT('Ctrl Pts',(40.8904785734415,-3.30827472180933,-5.65065218733584));
#68265=CARTESIAN_POINT('Ctrl Pts',(40.9910484833993,-0.210195783026292,
-6.54449153945545));
#68266=CARTESIAN_POINT('Ctrl Pts',(41.0916183933571,2.93885545219809,-5.85129732694312));
#68267=CARTESIAN_POINT('Ctrl Pts',(41.1921883033149,5.37523677011546,-3.73916854961161));
#68268=CARTESIAN_POINT('Ctrl Pts',(41.2927582132727,6.50812779843782,-0.720294617782823));
#68269=CARTESIAN_POINT('Ctrl Pts',(41.3933281232305,6.06280343802205,2.47325013880805));
#68270=CARTESIAN_POINT('Ctrl Pts',(41.4938980331883,4.147254462921,5.0670338657826));
#68271=CARTESIAN_POINT('Ctrl Pts',(41.5944679431461,1.22599985063719,6.43206624215296));
#68272=CARTESIAN_POINT('Ctrl Pts',(41.6950378531039,-1.99255867005031,6.23732809170829));
#68273=CARTESIAN_POINT('Ctrl Pts',(41.7956077630617,-4.72792342850226,4.53004324829526));
#68274=CARTESIAN_POINT('Ctrl Pts',(41.8961776730195,-6.31677082547448,1.72422681676178));
#68275=CARTESIAN_POINT('Ctrl Pts',(41.9967475829772,-6.37380673492663,-1.49971313357255));
#68276=CARTESIAN_POINT('Ctrl Pts',(42.0973174929351,-4.88519999791469,-4.3599739400116));
#68277=CARTESIAN_POINT('Ctrl Pts',(42.1978874028929,-2.2119364667287,-6.16294481918845));
#68278=CARTESIAN_POINT('Ctrl Pts',(42.2984573128507,0.99771975354065,-6.47140688495174));
#68279=CARTESIAN_POINT('Ctrl Pts',(42.3990272228085,3.96542979244218,-5.21055835188687));
#68280=CARTESIAN_POINT('Ctrl Pts',(42.4995971327663,5.97152652023215,-2.68615390388749));
#68281=CARTESIAN_POINT('Ctrl Pts',(42.6001670427241,6.52953320732713,0.489640553486283));
#68282=CARTESIAN_POINT('Ctrl Pts',(42.7007369526819,5.5041337124547,3.54669759813628));
#68283=CARTESIAN_POINT('Ctrl Pts',(42.8013068626397,3.14398653042817,5.74368352833721));
#68284=CARTESIAN_POINT('Ctrl Pts',(42.9018767725975,0.0214253212065685,
6.5478311472439));
#68285=CARTESIAN_POINT('Ctrl Pts',(43.0024466825553,-3.10633150996409,5.76413534950475));
#68286=CARTESIAN_POINT('Ctrl Pts',(43.1030165925131,-5.48080562398773,3.5826416914437));
#68287=CARTESIAN_POINT('Ctrl Pts',(43.2035865024709,-6.52618909222896,0.532360507248275));
#68288=CARTESIAN_POINT('Ctrl Pts',(43.3041564124287,-5.98897732353542,-2.64701764168366));
#68289=CARTESIAN_POINT('Ctrl Pts',(43.4047263223865,-3.99944370936796,-5.18449629113601));
#68290=CARTESIAN_POINT('Ctrl Pts',(43.5052962323443,-1.04004843851462,-6.46473905295097));
#68291=CARTESIAN_POINT('Ctrl Pts',(43.6058661423021,2.171557683375,-6.17728815945807));
#68292=CARTESIAN_POINT('Ctrl Pts',(43.7064360522599,4.85656293638531,-4.39185020488342));
#68293=CARTESIAN_POINT('Ctrl Pts',(43.8070059622177,6.36385585799084,-1.54139235625514));
#68294=CARTESIAN_POINT('Ctrl Pts',(43.9075758721756,6.3279192122232,1.68285181189028));
#68295=CARTESIAN_POINT('Ctrl Pts',(44.0081457821333,4.7574676047458,4.4990058642994));
#68296=CARTESIAN_POINT('Ctrl Pts',(44.1087156920912,2.03333419848207,6.22415486748919));
#68297=CARTESIAN_POINT('Ctrl Pts',(44.2092856020489,-1.18388100056117,6.43995167324384));
#68298=CARTESIAN_POINT('Ctrl Pts',(44.3098555120068,-4.11400607608704,5.09406574193198));
#68299=CARTESIAN_POINT('Ctrl Pts',(44.4104254219644,-6.04648821961621,2.51287325331947));
#68300=CARTESIAN_POINT('Ctrl Pts',(44.5109953319224,-6.51270217487891,-0.677688836069641));
#68301=CARTESIAN_POINT('Ctrl Pts',(44.6115652418801,-5.39959145905429,-3.70391196608585));
#68302=CARTESIAN_POINT('Ctrl Pts',(44.712135151838,-2.97708446253219,-5.83193963275989));
#68303=CARTESIAN_POINT('Ctrl Pts',(44.8127050617957,0.167362953394307,-6.54572695879052));
#68304=CARTESIAN_POINT('Ctrl Pts',(44.9132749717535,3.27122499719343,-5.67218113206398));
#68305=CARTESIAN_POINT('Ctrl Pts',(45.0138448817114,5.58181779513749,-3.42313626358817));
#68306=CARTESIAN_POINT('Ctrl Pts',(45.1144147916691,6.5388245827496,-0.343983797926061));
#68307=CARTESIAN_POINT('Ctrl Pts',(45.214984701627,5.91017203785263,2.81858444262207));
#68308=CARTESIAN_POINT('Ctrl Pts',(45.3155546115847,3.8483078614219,5.29764838215264));
#68309=CARTESIAN_POINT('Ctrl Pts',(45.4161245215426,0.853232341330176,6.49203714937878));
#68310=CARTESIAN_POINT('Ctrl Pts',(45.5166944315003,-2.34875128704718,6.11211249641235));
#68311=CARTESIAN_POINT('Ctrl Pts',(45.6172643414582,-4.98116475018809,4.25000582454772));
#68312=CARTESIAN_POINT('Ctrl Pts',(45.7178342514159,-6.40565004933793,1.35727639875713));
#68313=CARTESIAN_POINT('Ctrl Pts',(45.8184041613738,-6.27677072569056,-1.86459138534968));
#68314=CARTESIAN_POINT('Ctrl Pts',(45.9189740713315,-4.62577990428741,-4.63429736360291));
#68315=CARTESIAN_POINT('Ctrl Pts',(46.0195439812894,-1.85304143809858,-6.28019022051844));
#68316=CARTESIAN_POINT('Ctrl Pts',(46.1201138912471,1.36905798167786,-6.4031423551261));
#68317=CARTESIAN_POINT('Ctrl Pts',(46.220683801205,4.25916201942181,-4.97333798062435));
#68318=CARTESIAN_POINT('Ctrl Pts',(46.3212537111627,6.11642293386486,-2.33750342701311));
#68319=CARTESIAN_POINT('Ctrl Pts',(46.4218236211206,6.49045655203795,0.86517369545888));
#68320=CARTESIAN_POINT('Ctrl Pts',(46.5223935310784,5.29056004351288,3.85804694154842));
#68321=CARTESIAN_POINT('Ctrl Pts',(46.6229634410362,2.80770727870176,5.91534712542984));
#68322=CARTESIAN_POINT('Ctrl Pts',(46.723533350994,-0.356012084239504,6.53818072349498));
#68323=CARTESIAN_POINT('Ctrl Pts',(46.8241032609518,-3.43339882321811,5.57551112436612));
#68324=CARTESIAN_POINT('Ctrl Pts',(46.9246731709096,-5.67818930313457,3.26078487713835));
#68325=CARTESIAN_POINT('Ctrl Pts',(47.0252430808674,-6.5460237649891,0.155321104181599));
#68326=CARTESIAN_POINT('Ctrl Pts',(47.1258129908252,-5.82645309883866,-2.98780790283434));
#68327=CARTESIAN_POINT('Ctrl Pts',(47.226382900783,-3.69397257179779,-5.4063960654036));
#68328=CARTESIAN_POINT('Ctrl Pts',(47.3269528107408,-0.665706875973545,
-6.51393783609326));
#68329=CARTESIAN_POINT('Ctrl Pts',(47.4275227206986,2.5239921642147,-6.04185528891488));
#68330=CARTESIAN_POINT('Ctrl Pts',(47.5280926306564,5.1016252773058,-4.10462803517695));
#68331=CARTESIAN_POINT('Ctrl Pts',(47.6286625406142,6.44211865227558,-1.17203201629012));
#68332=CARTESIAN_POINT('Ctrl Pts',(47.729232450572,6.22040379962901,2.04478075762829));
#68333=CARTESIAN_POINT('Ctrl Pts',(47.8298023605298,4.4902463802744,4.76573595802775));
#68334=CARTESIAN_POINT('Ctrl Pts',(47.9303722704876,1.6712080790361,6.33100429108768));
#68335=CARTESIAN_POINT('Ctrl Pts',(48.0309421804453,-1.55309674274462,6.36100953346888));
#68336=CARTESIAN_POINT('Ctrl Pts',(48.1315120904032,-4.40077694135999,4.84847543972333));
#68337=CARTESIAN_POINT('Ctrl Pts',(48.232082000361,-6.18127252001054,2.16019022555157));
#68338=CARTESIAN_POINT('Ctrl Pts',(48.3326519103188,-6.4628148335752,-1.05193925876276));
#68339=CARTESIAN_POINT('Ctrl Pts',(48.4332218202766,-5.17713011337423,-4.00897437836659));
#68340=CARTESIAN_POINT('Ctrl Pts',(48.5337917302344,-2.63599579730208,-5.99383666225665));
#68341=CARTESIAN_POINT('Ctrl Pts',(48.6343616401922,0.544365230475053,-6.52519871521594));
#68342=CARTESIAN_POINT('Ctrl Pts',(48.7349315501501,3.59271815846718,-5.47420569681358));
#68343=CARTESIAN_POINT('Ctrl Pts',(48.8355014601077,5.76984002574585,-3.09572250928716));
#68344=CARTESIAN_POINT('Ctrl Pts',(48.9360713700657,6.5477806536249,0.0334707218546678));
#68345=CARTESIAN_POINT('Ctrl Pts',(49.0366412800234,5.73789010951729,3.1545473317593));
#68346=CARTESIAN_POINT('Ctrl Pts',(49.1372111899813,3.53656615319209,5.51064892923712));
#68347=CARTESIAN_POINT('Ctrl Pts',(49.237781099939,0.47762794909537,6.53042290509955));
#68348=CARTESIAN_POINT('Ctrl Pts',(49.3383510098969,-2.69713462150112,5.96657494805069));
#68349=CARTESIAN_POINT('Ctrl Pts',(49.4389209198545,-5.21784436815445,3.95583770229834));
#68350=CARTESIAN_POINT('Ctrl Pts',(49.5394908298125,-6.47323134720036,0.985813219037189));
#68351=CARTESIAN_POINT('Ctrl Pts',(49.6400607397701,-6.1588652968934,-2.22327012122418));
#68352=CARTESIAN_POINT('Ctrl Pts',(49.7406306497281,-4.35097971381765,-4.89321237094338));
#68353=CARTESIAN_POINT('Ctrl Pts',(49.8412005596858,-1.48798529558923,-6.37655483292632));
#68354=CARTESIAN_POINT('Ctrl Pts',(49.9417704696437,1.73584427591915,-6.31358823704594));
#68355=CARTESIAN_POINT('Ctrl Pts',(50.0423403796014,4.53873310478168,-4.7195819285997));
#68356=CARTESIAN_POINT('Ctrl Pts',(50.1429102895593,6.24098306280626,-1.98108106521952));
#68357=CARTESIAN_POINT('Ctrl Pts',(50.243480199517,6.42980000051754,1.237830251105));
#68358=CARTESIAN_POINT('Ctrl Pts',(50.3440501094749,5.05939597305955,4.15656879709634));
#68359=CARTESIAN_POINT('Ctrl Pts',(50.4446200194327,2.46209277740775,6.06734298788543));
#68360=CARTESIAN_POINT('Ctrl Pts',(50.5451899293904,-0.732265797325339,
6.50679172705517));
#68361=CARTESIAN_POINT('Ctrl Pts',(50.6457598393482,-3.74905054656244,5.36834907364693));
#68362=CARTESIAN_POINT('Ctrl Pts',(50.7463297493061,-5.85669376554837,2.92808639110816));
#68363=CARTESIAN_POINT('Ctrl Pts',(50.8468996592638,-6.54409378799878,-0.222234720693599));
#68364=CARTESIAN_POINT('Ctrl Pts',(50.9474695692217,-5.6445567002031,-3.31866410403319));
#68365=CARTESIAN_POINT('Ctrl Pts',(51.0480394791794,-3.37621947160443,-5.61032029894595));
#68366=CARTESIAN_POINT('Ctrl Pts',(51.1486093891373,-0.289151927488252,
-6.54147865088895));
#68367=CARTESIAN_POINT('Ctrl Pts',(51.249179299095,2.86803471013357,-5.88633406108379));
#68368=CARTESIAN_POINT('Ctrl Pts',(51.3497492090529,5.32972539943451,-3.80375852859097));
#68369=CARTESIAN_POINT('Ctrl Pts',(51.4503191190106,6.49896226735308,-0.798774827299281));
#68370=CARTESIAN_POINT('Ctrl Pts',(51.5508890289685,6.09220637993161,2.39991108200422));
#68371=CARTESIAN_POINT('Ctrl Pts',(51.6514589389262,4.20809568972269,5.01662061983395));
#68372=CARTESIAN_POINT('Ctrl Pts',(51.7520288488841,1.30352541720547,6.41680397580489));
#68373=CARTESIAN_POINT('Ctrl Pts',(51.8525987588419,-1.91714864687201,6.26091789141199));
#68374=CARTESIAN_POINT('Ctrl Pts',(51.9531686687997,-4.67291581441957,4.58676460792938));
#68375=CARTESIAN_POINT('Ctrl Pts',(52.0537385787574,-6.2955049195503,1.80032485544239));
#68376=CARTESIAN_POINT('Ctrl Pts',(52.1543084887153,-6.39143950104136,-1.42269212471807));
#68377=CARTESIAN_POINT('Ctrl Pts',(52.254878398673,-4.9374555054641,-4.30070748932868));
#68378=CARTESIAN_POINT('Ctrl Pts',(52.3554483086309,-2.28614280011545,-6.13580498994922));
#68379=CARTESIAN_POINT('Ctrl Pts',(52.4560182185886,0.919557566284525,-6.4829750623844));
#68380=CARTESIAN_POINT('Ctrl Pts',(52.5565881285465,3.90226601444088,-5.25802926292137));
#68381=CARTESIAN_POINT('Ctrl Pts',(52.6571580385042,5.93867831328004,-2.75801589346395));
#68382=CARTESIAN_POINT('Ctrl Pts',(52.7577279484621,6.53496623332907,0.410813955982539));
#68383=CARTESIAN_POINT('Ctrl Pts',(52.8582978584198,5.54653046729059,3.48002177473738));
#68384=CARTESIAN_POINT('Ctrl Pts',(52.9588677683777,3.21306583753008,5.70532730883329));
#68385=CARTESIAN_POINT('Ctrl Pts',(53.0594376783355,0.100435508100187,6.54709588182237));
#68386=CARTESIAN_POINT('Ctrl Pts',(53.1600075882933,-3.03655034564976,5.80119933944462));
#68387=CARTESIAN_POINT('Ctrl Pts',(53.260577498251,-5.43717535440492,3.6485169509979));
#68388=CARTESIAN_POINT('Ctrl Pts',(53.3611474082089,-6.51929002043674,0.611072342863134));
#68389=CARTESIAN_POINT('Ctrl Pts',(53.4617173181666,-6.02048246802809,-2.57455678274148));
#68390=CARTESIAN_POINT('Ctrl Pts',(53.5622872281245,-4.06171310065894,-5.13585810409048));
#68391=CARTESIAN_POINT('Ctrl Pts',(53.6628571380823,-1.11798180099441,-6.45171825764804));
#68392=CARTESIAN_POINT('Ctrl Pts',(53.7634270480401,2.09685911944926,-6.20304228489504));
#68393=CARTESIAN_POINT('Ctrl Pts',(53.8639969579979,4.80321351545239,-4.45013390300796));
#68394=CARTESIAN_POINT('Ctrl Pts',(53.9645668679557,6.34479275502275,-1.61807187027439));
#68395=CARTESIAN_POINT('Ctrl Pts',(54.0651367779135,6.34776524005276,1.60637117821377));
#68396=CARTESIAN_POINT('Ctrl Pts',(54.1657066878713,4.81141006630882,4.4412706377515));
#68397=CARTESIAN_POINT('Ctrl Pts',(54.266276597829,2.10829219583951,6.19916571456412));
#68398=CARTESIAN_POINT('Ctrl Pts',(54.3668465077869,-1.10608491795948,6.45376859123593));
#68399=CARTESIAN_POINT('Ctrl Pts',(54.4674164177447,-4.05223699846591,5.14333784807076));
#68400=CARTESIAN_POINT('Ctrl Pts',(54.5679863277025,-6.01572586397445,2.58565267587491));
#68401=CARTESIAN_POINT('Ctrl Pts',(54.6685562376603,-6.5204048812128,-0.599052163122007));
#68402=CARTESIAN_POINT('Ctrl Pts',(54.7691261476181,-5.44389427278895,-3.63848517874789));
#68403=CARTESIAN_POINT('Ctrl Pts',(54.8696960575759,-3.04723822545406,-5.79559295585254));
#68404=CARTESIAN_POINT('Ctrl Pts',(54.9702659675337,0.0883591872305582,
-6.54726604327576));
#68405=CARTESIAN_POINT('Ctrl Pts',(55.0708358774915,3.20255165237907,-5.71124916602977));
#68406=CARTESIAN_POINT('Ctrl Pts',(55.1714057874493,5.54008488415577,-3.4902271541179));
#68407=CARTESIAN_POINT('Ctrl Pts',(55.2719756974071,6.53423689591918,-0.422890962602382));
#68408=CARTESIAN_POINT('Ctrl Pts',(55.3725456073649,5.94367633180412,2.74711924961637));
#68409=CARTESIAN_POINT('Ctrl Pts',(55.4731155173227,3.91210579221266,5.2507116736487));
#68410=CARTESIAN_POINT('Ctrl Pts',(55.5736854272806,0.931192408451803,6.48151355909809));
#68411=CARTESIAN_POINT('Ctrl Pts',(55.6407320339191,-1.20560277749141,6.25335781087259));
#68412=CARTESIAN_POINT('Ctrl Pts',(55.6742553372383,-2.18270012582081,5.89135076165406));
#68413=CARTESIAN_POINT('Ctrl Pts',(54.6500381542954,-6.28284206479216,-0.000151303447314885));
#68414=CARTESIAN_POINT('Ctrl Pts',(54.6562108487504,-6.28303579177905,-0.191999457349239));
#68415=CARTESIAN_POINT('Ctrl Pts',(54.6623835432053,-6.2744219736263,-0.383830271012445));
#68416=CARTESIAN_POINT('Ctrl Pts',(54.6685562376603,-6.25687327693577,-0.574840192560178));
#68417=CARTESIAN_POINT('Ctrl Pts',(54.7020795409796,-6.16156801173819,-1.61219650166392));
#68418=CARTESIAN_POINT('Ctrl Pts',(54.7356028442988,-5.80273114226353,-2.62534084020598));
#68419=CARTESIAN_POINT('Ctrl Pts',(54.7691261476181,-5.22387003297044,-3.49143097232768));
#68420=CARTESIAN_POINT('Ctrl Pts',(54.8026494509374,-4.64500892367729,-4.35752110444949));
#68421=CARTESIAN_POINT('Ctrl Pts',(54.8361727542566,-3.84612357456576,-5.07655703015095));
#68422=CARTESIAN_POINT('Ctrl Pts',(54.8696960575759,-2.92408133122912,-5.56135384090563));
#68423=CARTESIAN_POINT('Ctrl Pts',(54.9032193608952,-2.00203908789258,-6.04615065166025));
#68424=CARTESIAN_POINT('Ctrl Pts',(54.9367426642144,-0.956839950330982,
-6.29670834746801));
#68425=CARTESIAN_POINT('Ctrl Pts',(54.9702659675337,0.0847916959744696,
-6.28265104916422));
#68426=CARTESIAN_POINT('Ctrl Pts',(55.003789270853,1.1264233422801,-6.26859375086043));
#68427=CARTESIAN_POINT('Ctrl Pts',(55.0373125741723,2.16448749732965,-5.98992145844508));
#68428=CARTESIAN_POINT('Ctrl Pts',(55.0708358774915,3.07310844681725,-5.48041497691869));
#68429=CARTESIAN_POINT('Ctrl Pts',(55.1043591808108,3.98172939630475,-4.97090849539237));
#68430=CARTESIAN_POINT('Ctrl Pts',(55.1378824841301,4.76090714023026,-4.23056782475512));
#68431=CARTESIAN_POINT('Ctrl Pts',(55.1714057874493,5.31618801415359,-3.34917479085056));
#68432=CARTESIAN_POINT('Ctrl Pts',(55.2033738582996,5.84570797673908,-2.50867185215095));
#68433=CARTESIAN_POINT('Ctrl Pts',(55.2353419291498,6.17162348859082,-1.53990053280162));
#68434=CARTESIAN_POINT('Ctrl Pts',(55.26731,6.25905495981401,-0.550339049542188));
#68435=CARTESIAN_POINT('',(18.8656682926829,-3.45323752142241,-4.38092825610446));
#68436=CARTESIAN_POINT('Ctrl Pts',(18.8656682926829,-3.45323752142232,-4.38092825610453));
#68437=CARTESIAN_POINT('Ctrl Pts',(18.8656682926829,-3.48865003681434,-4.35647151778965));
#68438=CARTESIAN_POINT('Ctrl Pts',(18.8656682926829,-3.5237620968794,-4.33160624123511));
#68439=CARTESIAN_POINT('Ctrl Pts',(18.8656682926829,-3.5585659267768,-4.30633657109999));
#68440=CARTESIAN_POINT('Ctrl Pts',(18.8656682926829,-3.68740336288153,-4.21279285705991));
#68441=CARTESIAN_POINT('Ctrl Pts',(18.8656682926829,-3.81201866337803,-4.11371135394565));
#68442=CARTESIAN_POINT('Ctrl Pts',(18.8656682926829,-3.93218904012421,-4.00949381605839));
#68443=CARTESIAN_POINT('Ctrl Pts',(18.8656682926829,-4.05370504575145,-3.90410928400258));
#68444=CARTESIAN_POINT('Ctrl Pts',(18.8656682926829,-4.17067657834504,-3.79347260745858));
#68445=CARTESIAN_POINT('Ctrl Pts',(18.8656682926829,-4.28284675048816,-3.67795294690854));
#68446=CARTESIAN_POINT('Ctrl Pts',(18.8656682926829,-4.3285937966682,-3.63083985842061));
#68447=CARTESIAN_POINT('Ctrl Pts',(18.8656682926829,-4.37354187975475,-3.58291408948346));
#68448=CARTESIAN_POINT('Ctrl Pts',(18.8656682926829,-4.41767199555344,-3.53419877631017));
#68449=CARTESIAN_POINT('Ctrl Pts',(18.8656682926829,-4.43553589143567,-3.51447878993244));
#68450=CARTESIAN_POINT('Ctrl Pts',(18.8656682926829,-4.45326188525846,-3.49463361845393));
#68451=CARTESIAN_POINT('Ctrl Pts',(18.8656682926829,-4.47084393932776,-3.47467064156079));
#68452=CARTESIAN_POINT('Ctrl Pts',(18.8656682926829,-4.57861483771785,-3.35230564678634));
#68453=CARTESIAN_POINT('Ctrl Pts',(18.8656682926829,-4.68103827851746,-3.22545389454906));
#68454=CARTESIAN_POINT('Ctrl Pts',(18.8656682926829,-4.77786631372815,-3.09451187441685));
#68455=CARTESIAN_POINT('Ctrl Pts',(18.8656682926829,-4.87490927228197,-2.96327921018901));
#68456=CARTESIAN_POINT('Ctrl Pts',(18.8656682926829,-4.96633249885538,-2.8279375517774));
#68457=CARTESIAN_POINT('Ctrl Pts',(18.8656682926829,-5.05185193133021,-2.68884672257815));
#68458=CARTESIAN_POINT('Ctrl Pts',(18.8656682926829,-5.08003907019056,-2.64300249275363));
#68459=CARTESIAN_POINT('Ctrl Pts',(18.8656682926829,-5.10758453375029,-2.59675068825047));
#68460=CARTESIAN_POINT('Ctrl Pts',(18.8656682926829,-5.1344771770417,-2.55010341702788));
#68461=CARTESIAN_POINT('Ctrl Pts',(18.8656682926829,-5.15017525977826,-2.52287393589613));
#68462=CARTESIAN_POINT('Ctrl Pts',(18.8656682926829,-5.16565088937481,-2.49550969580718));
#68463=CARTESIAN_POINT('Ctrl Pts',(18.8656682926829,-5.18090176556707,-2.46801305218364));
#68464=CARTESIAN_POINT('Ctrl Pts',(18.8656682926829,-5.19227387157726,-2.44750965668889));
#68465=CARTESIAN_POINT('Ctrl Pts',(18.8656682926829,-5.20351883698298,-2.42693647585482));
#68466=CARTESIAN_POINT('Ctrl Pts',(18.8656682926829,-5.21463146845408,-2.40630289334088));
#68467=CARTESIAN_POINT('Ctrl Pts',(18.8656682926829,-5.25995705387755,-2.32214378041977));
#68468=CARTESIAN_POINT('Ctrl Pts',(18.8656682926829,-5.30310402907468,-2.23693950757812));
#68469=CARTESIAN_POINT('Ctrl Pts',(18.8656682926829,-5.34402670803788,-2.15076859179026));
#68470=CARTESIAN_POINT('Ctrl Pts',(18.8656682926829,-5.41360113147134,-2.00426567618043));
#68471=CARTESIAN_POINT('Ctrl Pts',(18.8656682926829,-5.4767487513006,-1.85497050694108));
#68472=CARTESIAN_POINT('Ctrl Pts',(18.8656682926829,-5.53348127395234,-1.70334548898074));
#68473=CARTESIAN_POINT('Ctrl Pts',(18.8656682926829,-5.59097936210052,-1.54967439803224));
#68474=CARTESIAN_POINT('Ctrl Pts',(18.8656682926829,-5.64188832664486,-1.39360953369602));
#68475=CARTESIAN_POINT('Ctrl Pts',(18.8656682926829,-5.6861761332453,-1.23560191172807));
#68476=CARTESIAN_POINT('Ctrl Pts',(18.8656682926829,-5.72963766859383,-1.08054221528722));
#68477=CARTESIAN_POINT('Ctrl Pts',(18.8656682926829,-5.76672284284825,-0.923610856409404));
#68478=CARTESIAN_POINT('Ctrl Pts',(18.8656682926829,-5.79735709018424,-0.765215240674514));
#68479=CARTESIAN_POINT('Ctrl Pts',(18.8656682926829,-5.82033277568623,-0.646418528873346));
#68480=CARTESIAN_POINT('Ctrl Pts',(18.8656682926829,-5.83967893411615,-0.526797729632665));
#68481=CARTESIAN_POINT('Ctrl Pts',(18.8656682926829,-5.85534696996504,-0.406521158123589));
#68482=CARTESIAN_POINT('Ctrl Pts',(18.8656682926829,-5.8588777922724,-0.379416599145501));
#68483=CARTESIAN_POINT('Ctrl Pts',(18.8656682926829,-5.86222176578814,-0.352278731796697));
#68484=CARTESIAN_POINT('Ctrl Pts',(18.8656682926829,-5.86537822718048,-0.325109475094044));
#68485=CARTESIAN_POINT('Ctrl Pts',(18.8656682926829,-5.86791752154436,-0.303252486574072));
#68486=CARTESIAN_POINT('Ctrl Pts',(18.8656682926829,-5.87033448129072,-0.281383433945046));
#68487=CARTESIAN_POINT('Ctrl Pts',(18.8656682926829,-5.87262849180244,-0.259508980115285));
#68488=CARTESIAN_POINT('Ctrl Pts',(18.8656682926829,-5.89018289996684,-0.0921195593006232));
#68489=CARTESIAN_POINT('Ctrl Pts',(18.8656682926829,-5.9005537142749,0.0756879104303696));
#68490=CARTESIAN_POINT('Ctrl Pts',(18.8656682926829,-5.90373035404805,0.243439431795315));
#68491=CARTESIAN_POINT('Ctrl Pts',(18.8656682926829,-5.90649206425808,0.389279414414141));
#68492=CARTESIAN_POINT('Ctrl Pts',(18.8656682926829,-5.90381560822746,0.535077850343277));
#68493=CARTESIAN_POINT('Ctrl Pts',(18.8656682926829,-5.89566406821674,0.680534476662218));
#68494=CARTESIAN_POINT('Ctrl Pts',(18.8656682926829,-5.88633282846231,0.847041744278821));
#68495=CARTESIAN_POINT('Ctrl Pts',(18.8656682926829,-5.86982839107916,1.01310157460892));
#68496=CARTESIAN_POINT('Ctrl Pts',(18.8656682926829,-5.84633900059541,1.1783009017161));
#68497=CARTESIAN_POINT('Ctrl Pts',(18.8656682926829,-5.82271391797959,1.34445454259855));
#68498=CARTESIAN_POINT('Ctrl Pts',(18.8656682926829,-5.79202283543017,1.50973842898197));
#68499=CARTESIAN_POINT('Ctrl Pts',(18.8656682926829,-5.75440471333326,1.67372929806714));
#68500=CARTESIAN_POINT('Ctrl Pts',(18.8656682926829,-5.73578643671118,1.75489303495586));
#68501=CARTESIAN_POINT('Ctrl Pts',(18.8656682926829,-5.71547055624302,1.83573992830929));
#68502=CARTESIAN_POINT('Ctrl Pts',(18.8656682926829,-5.69346932747585,1.91621755238797));
#68503=CARTESIAN_POINT('Ctrl Pts',(18.8656682926829,-5.68781994444017,1.93688225839293));
#68504=CARTESIAN_POINT('Ctrl Pts',(18.8656682926829,-5.68205868413308,1.95752520127841));
#68505=CARTESIAN_POINT('Ctrl Pts',(18.8656682926829,-5.67618817005215,1.97813692025152));
#68506=CARTESIAN_POINT('Ctrl Pts',(18.8656682926829,-5.62959721149286,2.14172050616481));
#68507=CARTESIAN_POINT('Ctrl Pts',(18.8656682926829,-5.57621803009231,2.3030318060249));
#68508=CARTESIAN_POINT('Ctrl Pts',(18.8656682926829,-5.51628649487988,2.46165162563508));
#68509=CARTESIAN_POINT('Ctrl Pts',(18.8656682926829,-5.45587730439769,2.62153564767983));
#68510=CARTESIAN_POINT('Ctrl Pts',(18.8656682926829,-5.38881077087805,2.77868584241825));
#68511=CARTESIAN_POINT('Ctrl Pts',(18.8656682926829,-5.31527537851503,2.93267169117675));
#68512=CARTESIAN_POINT('Ctrl Pts',(18.8656682926829,-5.24179519018865,3.08654194062772));
#68513=CARTESIAN_POINT('Ctrl Pts',(18.8656682926829,-5.16185565593192,3.23725332913277));
#68514=CARTESIAN_POINT('Ctrl Pts',(18.8656682926829,-5.07559460954087,3.38436410593989));
#68515=CARTESIAN_POINT('Ctrl Pts',(18.8656682926829,-5.05043690689858,3.4272683985868));
#68516=CARTESIAN_POINT('Ctrl Pts',(18.8656682926829,-5.02474119684349,3.46986631351909));
#68517=CARTESIAN_POINT('Ctrl Pts',(18.8656682926829,-4.99851012946874,3.51214655673337));
#68518=CARTESIAN_POINT('Ctrl Pts',(18.8656682926829,-4.93079775741929,3.62128796215033));
#68519=CARTESIAN_POINT('Ctrl Pts',(18.8656682926829,-4.85951900835881,3.72831322166999));
#68520=CARTESIAN_POINT('Ctrl Pts',(18.8656682926829,-4.78481237253093,3.83309766072526));
#68521=CARTESIAN_POINT('Ctrl Pts',(18.8656682926829,-4.75212821935624,3.87894085281194));
#68522=CARTESIAN_POINT('Ctrl Pts',(18.8656682926829,-4.7187877661218,3.92435501713608));
#68523=CARTESIAN_POINT('Ctrl Pts',(18.8656682926829,-4.6848018029294,3.96932910582263));
#68524=CARTESIAN_POINT('Ctrl Pts',(18.8656682926829,-4.66369258750289,3.99726321854209));
#68525=CARTESIAN_POINT('Ctrl Pts',(18.8656682926829,-4.64233433481401,4.02502754913883));
#68526=CARTESIAN_POINT('Ctrl Pts',(18.8656682926829,-4.62072954176209,4.05261937053978));
#68527=CARTESIAN_POINT('Ctrl Pts',(18.8656682926829,-4.60757582916439,4.06941818401988));
#68528=CARTESIAN_POINT('Ctrl Pts',(18.8656682926829,-4.59433336696083,4.0861496280533));
#68529=CARTESIAN_POINT('Ctrl Pts',(18.8656682926829,-4.58100877205513,4.10280586710038));
#68530=CARTESIAN_POINT('Ctrl Pts',(18.8656682926829,-4.47422348374094,4.23629144782243));
#68531=CARTESIAN_POINT('Ctrl Pts',(18.8656682926829,-4.36205657963184,4.36508990258962));
#68532=CARTESIAN_POINT('Ctrl Pts',(18.8656682926829,-4.24491373451659,4.48896255029951));
#68533=CARTESIAN_POINT('Ctrl Pts',(18.8656682926829,-4.12562038138394,4.6151092517237));
#68534=CARTESIAN_POINT('Ctrl Pts',(18.8656682926829,-4.0011663610317,4.73614821512326));
#68535=CARTESIAN_POINT('Ctrl Pts',(18.8656682926829,-3.87193135828886,4.85180438829313));
#68536=CARTESIAN_POINT('Ctrl Pts',(18.8656682926829,-3.74243680935971,4.96769283691494));
#68537=CARTESIAN_POINT('Ctrl Pts',(18.8656682926829,-3.60814155977152,5.078177406693));
#68538=CARTESIAN_POINT('Ctrl Pts',(18.8656682926829,-3.46938570366927,5.18294999428408));
#68539=CARTESIAN_POINT('Ctrl Pts',(18.8656682926829,-3.33204959495397,5.28665055067132));
#68540=CARTESIAN_POINT('Ctrl Pts',(18.8656682926829,-3.19034314609964,5.3847558922719));
#68541=CARTESIAN_POINT('Ctrl Pts',(18.8656682926829,-3.04456302413475,5.4769289961042));
#68542=CARTESIAN_POINT('Ctrl Pts',(18.8656682926829,-2.96213372136761,5.52904697062894));
#68543=CARTESIAN_POINT('Ctrl Pts',(18.8656682926829,-2.87840143703307,5.57926756973073));
#68544=CARTESIAN_POINT('Ctrl Pts',(18.8656682926829,-2.79341604200811,5.62752347417154));
#68545=CARTESIAN_POINT('Ctrl Pts',(18.8656682926829,-3.45323752142241,-4.38092825610446));
#68546=CARTESIAN_POINT('Ctrl Pts',(18.8976363635332,-2.76035226152897,-4.92661473406192));
#68547=CARTESIAN_POINT('Ctrl Pts',(18.9631277377027,-1.07108282839872,-5.70279110802667));
#68548=CARTESIAN_POINT('Ctrl Pts',(19.0621424151914,1.74296490233074,-5.54583252750879));
#68549=CARTESIAN_POINT('Ctrl Pts',(19.1627123251492,4.17855117605108,-4.04150148361096));
#68550=CARTESIAN_POINT('Ctrl Pts',(19.263282235107,5.60083956100377,-1.55713407092352));
#68551=CARTESIAN_POINT('Ctrl Pts',(19.3638521450648,5.66493061750189,1.30484940988588));
#68552=CARTESIAN_POINT('Ctrl Pts',(19.4644220550226,4.35528013812923,3.85040169824184));
#68553=CARTESIAN_POINT('Ctrl Pts',(19.5649919649805,1.98947835131264,5.4622381255191));
#68554=CARTESIAN_POINT('Ctrl Pts',(19.6655618749382,-0.858770415672562,
5.74948485589373));
#68555=CARTESIAN_POINT('Ctrl Pts',(19.766131784896,-3.49876799771652,4.64248730288639));
#68556=CARTESIAN_POINT('Ctrl Pts',(19.861975432269,-5.20612390037616,2.51461999470827));
#68557=CARTESIAN_POINT('Ctrl Pts',(19.9242957763227,-5.57736077906089,0.794440147261595));
#68558=CARTESIAN_POINT('Ctrl Pts',(19.9530928170571,-5.57809442763664,-0.000115493386879852));
#68559=CARTESIAN_POINT('Origin',(18.8656682926829,-1.21203632162606E-15,
2.67744564496562E-16));
#68560=CARTESIAN_POINT('',(18.8656682926829,-6.28269,-7.69407619853508E-16));
#68561=CARTESIAN_POINT('Origin',(18.8656682926829,0.,0.));
#68562=CARTESIAN_POINT('Origin',(18.8656682926829,0.,0.));
#68563=CARTESIAN_POINT('',(18.8656682926829,3.45292578700092,-4.38059386100379));
#68564=CARTESIAN_POINT('Ctrl Pts',(18.8656682926829,2.79368235183429,5.62796419942309));
#68565=CARTESIAN_POINT('Ctrl Pts',(18.8656682926829,2.83576950574192,5.60408862809779));
#68566=CARTESIAN_POINT('Ctrl Pts',(18.8656682926829,2.87756131190663,5.57972664274282));
#68567=CARTESIAN_POINT('Ctrl Pts',(18.8656682926829,2.91904845943543,5.55488054600549));
#68568=CARTESIAN_POINT('Ctrl Pts',(18.8656682926829,3.06884955249153,5.46516667867235));
#68569=CARTESIAN_POINT('Ctrl Pts',(18.8656682926829,3.21468106272101,5.36914430082019));
#68570=CARTESIAN_POINT('Ctrl Pts',(18.8656682926829,3.35622549203696,5.26716183191894));
#68571=CARTESIAN_POINT('Ctrl Pts',(18.8656682926829,3.49796073607223,5.16504188140662));
#68572=CARTESIAN_POINT('Ctrl Pts',(18.8656682926829,3.6353978454227,5.05694519678979));
#68573=CARTESIAN_POINT('Ctrl Pts',(18.8656682926829,3.76818146341041,4.94318453571594));
#68574=CARTESIAN_POINT('Ctrl Pts',(18.8656682926829,3.80445178328906,4.91211040451447));
#68575=CARTESIAN_POINT('Ctrl Pts',(18.8656682926829,3.84037465782938,4.8806134817403));
#68576=CARTESIAN_POINT('Ctrl Pts',(18.8656682926829,3.87594229270048,4.84869974661354));
#68577=CARTESIAN_POINT('Ctrl Pts',(18.8656682926829,3.90190760479151,4.82540187776282));
#68578=CARTESIAN_POINT('Ctrl Pts',(18.8656682926829,3.92768359091741,4.80188187019607));
#68579=CARTESIAN_POINT('Ctrl Pts',(18.8656682926829,3.9532671322017,4.77814200052023));
#68580=CARTESIAN_POINT('Ctrl Pts',(18.8656682926829,3.97302840818941,4.7598048160248));
#68581=CARTESIAN_POINT('Ctrl Pts',(18.8656682926829,3.99266782739885,4.74134297711141));
#68582=CARTESIAN_POINT('Ctrl Pts',(18.8656682926829,4.01218355661887,4.72275839410534));
#68583=CARTESIAN_POINT('Ctrl Pts',(18.8656682926829,4.13756687421348,4.60335744079516));
#68584=CARTESIAN_POINT('Ctrl Pts',(18.8656682926829,4.25785698662503,4.47888420345246));
#68585=CARTESIAN_POINT('Ctrl Pts',(18.8656682926829,4.37272354223849,4.34965993119528));
#68586=CARTESIAN_POINT('Ctrl Pts',(18.8656682926829,4.48679275701944,4.2213326631903));
#68587=CARTESIAN_POINT('Ctrl Pts',(18.8656682926829,4.59551387493921,4.08831950882343));
#68588=CARTESIAN_POINT('Ctrl Pts',(18.8656682926829,4.69852069627652,3.95090699223527));
#68589=CARTESIAN_POINT('Ctrl Pts',(18.8656682926829,4.73486744777379,3.90241992576527));
#68590=CARTESIAN_POINT('Ctrl Pts',(18.8656682926829,4.77050230029976,3.85338488547739));
#68591=CARTESIAN_POINT('Ctrl Pts',(18.8656682926829,4.80540773103432,3.80381382155591));
#68592=CARTESIAN_POINT('Ctrl Pts',(18.8656682926829,4.82578390156854,3.7748765349856));
#68593=CARTESIAN_POINT('Ctrl Pts',(18.8656682926829,4.84591149370507,3.74575658302111));
#68594=CARTESIAN_POINT('Ctrl Pts',(18.8656682926829,4.86578689507932,3.71645630022115));
#68595=CARTESIAN_POINT('Ctrl Pts',(18.8656682926829,4.87882532276676,3.69723507236691));
#68596=CARTESIAN_POINT('Ctrl Pts',(18.8656682926829,4.8917549419235,3.67793655455239));
#68597=CARTESIAN_POINT('Ctrl Pts',(18.8656682926829,4.90456734688091,3.65857283768931));
#68598=CARTESIAN_POINT('Ctrl Pts',(18.8656682926829,4.96261329803569,3.57084650005438));
#68599=CARTESIAN_POINT('Ctrl Pts',(18.8656682926829,5.01829450643616,3.48172290231582));
#68600=CARTESIAN_POINT('Ctrl Pts',(18.8656682926829,5.07154077855382,3.3912753413832));
#68601=CARTESIAN_POINT('Ctrl Pts',(18.8656682926829,5.15772293769219,3.24488075299308));
#68602=CARTESIAN_POINT('Ctrl Pts',(18.8656682926829,5.23752878987822,3.09501884953656));
#68603=CARTESIAN_POINT('Ctrl Pts',(18.8656682926829,5.31086851293914,2.94214018851873));
#68604=CARTESIAN_POINT('Ctrl Pts',(18.8656682926829,5.38457302915425,2.78850110618168));
#68605=CARTESIAN_POINT('Ctrl Pts',(18.8656682926829,5.45174713407391,2.63181444742355));
#68606=CARTESIAN_POINT('Ctrl Pts',(18.8656682926829,5.51225047381773,2.47251913208819));
#68607=CARTESIAN_POINT('Ctrl Pts',(18.8656682926829,5.57066005449078,2.31873633908343));
#68608=CARTESIAN_POINT('Ctrl Pts',(18.8656682926829,5.62285245369036,2.1625216197253));
#68609=CARTESIAN_POINT('Ctrl Pts',(18.8656682926829,5.66865558800209,2.00426337214573));
#68610=CARTESIAN_POINT('Ctrl Pts',(18.8656682926829,5.70300793873588,1.88556968646105));
#68611=CARTESIAN_POINT('Ctrl Pts',(18.8656682926829,5.73376542007911,1.76572633040402));
#68612=CARTESIAN_POINT('Ctrl Pts',(18.8656682926829,5.76083805161128,1.6448980065652));
#68613=CARTESIAN_POINT('Ctrl Pts',(18.8656682926829,5.76715184157729,1.61671882281072));
#68614=CARTESIAN_POINT('Ctrl Pts',(18.8656682926829,5.77326514699577,1.58848607606894));
#68615=CARTESIAN_POINT('Ctrl Pts',(18.8656682926829,5.77917670617993,1.5602018761831));
#68616=CARTESIAN_POINT('Ctrl Pts',(18.8656682926829,5.78340953605446,1.53994965464149));
#68617=CARTESIAN_POINT('Ctrl Pts',(18.8656682926829,5.78753871869447,1.51967184833655));
#68618=CARTESIAN_POINT('Ctrl Pts',(18.8656682926829,5.79156137635828,1.49938216970943));
#68619=CARTESIAN_POINT('Ctrl Pts',(18.8656682926829,5.82418927474855,1.3348119706163));
#68620=CARTESIAN_POINT('Ctrl Pts',(18.8656682926829,5.84986051383317,1.16923824915711));
#68621=CARTESIAN_POINT('Ctrl Pts',(18.8656682926829,5.86846654733547,1.00308241347301));
#68622=CARTESIAN_POINT('Ctrl Pts',(18.8656682926829,5.88557367486975,0.850312126820536));
#68623=CARTESIAN_POINT('Ctrl Pts',(18.8656682926829,5.89670763199262,0.697049144108283));
#68624=CARTESIAN_POINT('Ctrl Pts',(18.8656682926829,5.90174533861939,0.543617239147347));
#68625=CARTESIAN_POINT('Ctrl Pts',(18.8656682926829,5.90723869521276,0.376307741156566));
#68626=CARTESIAN_POINT('Ctrl Pts',(18.8656682926829,5.90548366105168,0.208796643477492));
#68627=CARTESIAN_POINT('Ctrl Pts',(18.8656682926829,5.89656614992036,0.041539681498394));
#68628=CARTESIAN_POINT('Ctrl Pts',(18.8656682926829,5.88769080065284,-0.124926491980615));
#68629=CARTESIAN_POINT('Ctrl Pts',(18.8656682926829,5.87172030576114,-0.291141651826502));
#68630=CARTESIAN_POINT('Ctrl Pts',(18.8656682926829,5.84869066007965,-0.4566401983567));
#68631=CARTESIAN_POINT('Ctrl Pts',(18.8656682926829,5.83770118329379,-0.535614163494544));
#68632=CARTESIAN_POINT('Ctrl Pts',(18.8656682926829,5.82510358325441,-0.614424642607473));
#68633=CARTESIAN_POINT('Ctrl Pts',(18.8656682926829,5.81089806702808,-0.693018993923835));
#68634=CARTESIAN_POINT('Ctrl Pts',(18.8656682926829,5.80729284562518,-0.712965473375758));
#68635=CARTESIAN_POINT('Ctrl Pts',(18.8656682926829,5.80358357016803,-0.732900503194119));
#68636=CARTESIAN_POINT('Ctrl Pts',(18.8656682926829,5.79977180301852,-0.75281498132816));
#68637=CARTESIAN_POINT('Ctrl Pts',(18.8656682926829,5.7687219432075,-0.915034164719276));
#68638=CARTESIAN_POINT('Ctrl Pts',(18.8656682926829,5.73093354192466,-1.07559795340867));
#68639=CARTESIAN_POINT('Ctrl Pts',(18.8656682926829,5.68653260689291,-1.23408041710266));
#68640=CARTESIAN_POINT('Ctrl Pts',(18.8656682926829,5.64217918661081,-1.39239328403969));
#68641=CARTESIAN_POINT('Ctrl Pts',(18.8656682926829,5.59122714042856,-1.54862999865536));
#68642=CARTESIAN_POINT('Ctrl Pts',(18.8656682926829,5.53375236356643,-1.70235124610643));
#68643=CARTESIAN_POINT('Ctrl Pts',(18.8656682926829,5.4770089713036,-1.85411634237068));
#68644=CARTESIAN_POINT('Ctrl Pts',(18.8656682926829,5.41390750143894,-2.00343021336511));
#68645=CARTESIAN_POINT('Ctrl Pts',(18.8656682926829,5.34447662605786,-2.14984576322425));
#68646=CARTESIAN_POINT('Ctrl Pts',(18.8656682926829,5.32531108420779,-2.19026198054724));
#68647=CARTESIAN_POINT('Ctrl Pts',(18.8656682926829,5.30566301286859,-2.2304571801222));
#68648=CARTESIAN_POINT('Ctrl Pts',(18.8656682926829,5.28553245444563,-2.27042152789026));
#68649=CARTESIAN_POINT('Ctrl Pts',(18.8656682926829,5.232647265755,-2.37541226029837));
#68650=CARTESIAN_POINT('Ctrl Pts',(18.8656682926829,5.17643271285519,-2.4788104498093));
#68651=CARTESIAN_POINT('Ctrl Pts',(18.8656682926829,5.11698334956708,-2.58047663726544));
#68652=CARTESIAN_POINT('Ctrl Pts',(18.8656682926829,5.09097425312854,-2.6249555942775));
#68653=CARTESIAN_POINT('Ctrl Pts',(18.8656682926829,5.06434587802933,-2.66910290268612));
#68654=CARTESIAN_POINT('Ctrl Pts',(18.8656682926829,5.03710563512655,-2.71290623030739));
#68655=CARTESIAN_POINT('Ctrl Pts',(18.8656682926829,5.01908597407371,-2.74188251805709));
#68656=CARTESIAN_POINT('Ctrl Pts',(18.8656682926829,5.00079855728729,-2.7707082734982));
#68657=CARTESIAN_POINT('Ctrl Pts',(18.8656682926829,4.98224546314655,-2.79937982321383));
#68658=CARTESIAN_POINT('Ctrl Pts',(18.8656682926829,4.97113612836914,-2.81654794848511));
#68659=CARTESIAN_POINT('Ctrl Pts',(18.8656682926829,4.9599316556517,-2.8336605039157));
#68660=CARTESIAN_POINT('Ctrl Pts',(18.8656682926829,4.94864037660227,-2.8507050608972));
#68661=CARTESIAN_POINT('Ctrl Pts',(18.8656682926829,4.85950934438235,-2.98525128465474));
#68662=CARTESIAN_POINT('Ctrl Pts',(18.8656682926829,4.76485187654229,-3.11575104860376));
#68663=CARTESIAN_POINT('Ctrl Pts',(18.8656682926829,4.66498905339689,-3.24190539502472));
#68664=CARTESIAN_POINT('Ctrl Pts',(18.8656682926829,4.56466269505643,-3.36864531451214));
#68665=CARTESIAN_POINT('Ctrl Pts',(18.8656682926829,4.45908202239174,-3.49099993670225));
#68666=CARTESIAN_POINT('Ctrl Pts',(18.8656682926829,4.34853253898482,-3.60863276114994));
#68667=CARTESIAN_POINT('Ctrl Pts',(18.8656682926829,4.23874440681553,-3.72545545158598));
#68668=CARTESIAN_POINT('Ctrl Pts',(18.8656682926829,4.12405510639962,-3.83762162938683));
#68669=CARTESIAN_POINT('Ctrl Pts',(18.8656682926829,4.00471307570633,-3.94476131146243));
#68670=CARTESIAN_POINT('Ctrl Pts',(18.8656682926829,3.88777618067956,-4.04974177545567));
#68671=CARTESIAN_POINT('Ctrl Pts',(18.8656682926829,3.76637165277503,-4.14989663134919));
#68672=CARTESIAN_POINT('Ctrl Pts',(18.8656682926829,3.64071140247854,-4.24483318001998));
#68673=CARTESIAN_POINT('Ctrl Pts',(18.8656682926829,3.57913066675992,-4.29135753835876));
#68674=CARTESIAN_POINT('Ctrl Pts',(18.8656682926829,3.51652760821553,-4.33662797130161));
#68675=CARTESIAN_POINT('Ctrl Pts',(18.8656682926829,3.45292578700089,-4.38059386100381));
#68676=CARTESIAN_POINT('Origin',(18.8656682926829,0.,0.));
#68677=CARTESIAN_POINT('Origin',(16.5082437683087,0.,0.));
#68678=CARTESIAN_POINT('Ctrl Pts',(18.8656682926829,3.45292578700087,-4.38059386100382));
#68679=CARTESIAN_POINT('Ctrl Pts',(18.8991915960022,4.17945978894053,-3.8079162583704));
#68680=CARTESIAN_POINT('Ctrl Pts',(18.9662382026407,5.34139059168272,-2.29470092783305));
#68681=CARTESIAN_POINT('Ctrl Pts',(19.0668081125985,5.78874853530519,0.533337577335307));
#68682=CARTESIAN_POINT('Ctrl Pts',(19.1673780225563,4.83241525876795,3.23130860481921));
#68683=CARTESIAN_POINT('Ctrl Pts',(19.2679479325141,2.70419169563657,5.14605048923388));
#68684=CARTESIAN_POINT('Ctrl Pts',(19.3685178424719,-0.0797792217301073,
5.81269672472357));
#68685=CARTESIAN_POINT('Ctrl Pts',(19.4690877524298,-2.84441229285594,5.06986231595082));
#68686=CARTESIAN_POINT('Ctrl Pts',(19.5696576623875,-4.91927346795933,3.09754298939177));
#68687=CARTESIAN_POINT('Ctrl Pts',(19.6410430010139,-5.54528435432487,1.16441856903096));
#68688=CARTESIAN_POINT('Ctrl Pts',(19.678905036321,-5.57823027330273,0.119820339136794));
#68689=CARTESIAN_POINT('Ctrl Pts',(19.6832437683088,-5.57812419168581,0.000109767319341463));
#68690=CARTESIAN_POINT('Ctrl Pts',(18.4587229554446,3.88925862210691,-4.93415251147216));
#68691=CARTESIAN_POINT('Ctrl Pts',(18.4922462587639,4.70760190707855,-4.28910786205787));
#68692=CARTESIAN_POINT('Ctrl Pts',(18.5592928654024,6.01636139732571,-2.58467338114522));
#68693=CARTESIAN_POINT('Ctrl Pts',(18.6598627753602,6.52025022863267,0.600733377750014));
#68694=CARTESIAN_POINT('Ctrl Pts',(18.760432685318,5.44306882630348,3.63963653643918));
#68695=CARTESIAN_POINT('Ctrl Pts',(18.8610025952758,3.0459099085414,5.79633692400731));
#68696=CARTESIAN_POINT('Ctrl Pts',(18.9615725052336,-0.0898606124542653,
6.54722465783414));
#68697=CARTESIAN_POINT('Ctrl Pts',(19.0621424151914,-3.20384963860623,5.71052114685986));
#68698=CARTESIAN_POINT('Ctrl Pts',(19.1627123251492,-5.54090297039958,3.48896747917141));
#68699=CARTESIAN_POINT('Ctrl Pts',(19.263282235107,-6.53429461288024,0.421369638803437));
#68700=CARTESIAN_POINT('Ctrl Pts',(19.3638521450648,-5.94312415339177,-2.74842399726426));
#68701=CARTESIAN_POINT('Ctrl Pts',(19.4644220550226,-3.91075185848052,-5.25172001492936));
#68702=CARTESIAN_POINT('Ctrl Pts',(19.5649919649804,-0.930025269268408,
-6.48148211124559));
#68703=CARTESIAN_POINT('Ctrl Pts',(19.6655618749382,2.27623147590318,-6.13948850396696));
#68704=CARTESIAN_POINT('Ctrl Pts',(19.7661317848961,4.9305041351233,-4.30867517567208));
#68705=CARTESIAN_POINT('Ctrl Pts',(19.8667016948538,6.38913374117629,-1.43301133769862));
#68706=CARTESIAN_POINT('Ctrl Pts',(19.9672716048117,6.29840393779587,1.79015626640114));
#68707=CARTESIAN_POINT('Ctrl Pts',(20.0678415147694,4.68031658966875,4.57921264451185));
#68708=CARTESIAN_POINT('Ctrl Pts',(20.1684114247272,1.92725650346534,6.2578138330424));
#68709=CARTESIAN_POINT('Ctrl Pts',(20.2689813346851,-1.29316162884032,6.41890058728604));
#68710=CARTESIAN_POINT('Ctrl Pts',(20.3695512446428,-4.19998917778443,5.02340945765924));
#68711=CARTESIAN_POINT('Ctrl Pts',(20.4701211546007,-6.08832296738331,2.40974586754627));
#68712=CARTESIAN_POINT('Ctrl Pts',(20.5706910645584,-6.5002436779878,-0.788279025514826));
#68713=CARTESIAN_POINT('Ctrl Pts',(20.6712609745163,-5.33586089248439,-3.79514693118953));
#68714=CARTESIAN_POINT('Ctrl Pts',(20.771830884474,-2.87753643370932,-5.88169497418324));
#68715=CARTESIAN_POINT('Ctrl Pts',(20.8724007944319,0.278588133120066,-6.54193704847586));
#68716=CARTESIAN_POINT('Ctrl Pts',(20.9729707043896,3.36715531751224,-5.61576502030334));
#68717=CARTESIAN_POINT('Ctrl Pts',(21.0735406143475,5.63919023593738,-3.32777480876387));
#68718=CARTESIAN_POINT('Ctrl Pts',(21.1741105243053,6.54372637653163,-0.232802070822349));
#68719=CARTESIAN_POINT('Ctrl Pts',(21.2746804342631,5.86141450384058,2.91862496893136));
#68720=CARTESIAN_POINT('Ctrl Pts',(21.3752503442209,3.75771465964378,5.36228796613461));
#68721=CARTESIAN_POINT('Ctrl Pts',(21.4758202541787,0.74277224523095,6.50560074757205));
#68722=CARTESIAN_POINT('Ctrl Pts',(21.5763901641365,-2.45229179925024,6.07131094792556));
#68723=CARTESIAN_POINT('Ctrl Pts',(21.6769600740943,-5.05267719341661,4.16473346976847));
#68724=CARTESIAN_POINT('Ctrl Pts',(21.7775299840521,-6.42779271766877,1.24821171031312));
#68725=CARTESIAN_POINT('Ctrl Pts',(21.8780998940099,-6.24417404111461,-1.97100031439601));
#68726=CARTESIAN_POINT('Ctrl Pts',(21.9786698039676,-4.54634853475423,-4.71224645955806));
#68727=CARTESIAN_POINT('Ctrl Pts',(22.0792397139255,-1.74603742234317,-6.31077689471399));
#68728=CARTESIAN_POINT('Ctrl Pts',(22.1798096238833,1.47768626194704,-6.37894936539961));
#68729=CARTESIAN_POINT('Ctrl Pts',(22.2803795338411,4.34307229974981,-4.90023210615833));
#68730=CARTESIAN_POINT('Ctrl Pts',(22.3809494437989,6.15526704350443,-2.233212779434));
#68731=CARTESIAN_POINT('Ctrl Pts',(22.4815193537567,6.47481482783961,0.975358723889488));
#68732=CARTESIAN_POINT('Ctrl Pts',(22.5820892637145,5.22422559012998,3.94740657628651));
#68733=CARTESIAN_POINT('Ctrl Pts',(22.6826591736723,2.70676614397705,5.96221173197486));
#68734=CARTESIAN_POINT('Ctrl Pts',(22.7832290836301,-0.467081762028401,
6.53118567510214));
#68735=CARTESIAN_POINT('Ctrl Pts',(22.8837989935879,-3.52766274281934,5.51635271424909));
#68736=CARTESIAN_POINT('Ctrl Pts',(22.9843689035457,-5.73278854518983,3.16380896882526));
#68737=CARTESIAN_POINT('Ctrl Pts',(23.0849388135035,-6.5477180603006,0.0440442719588136));
#68738=CARTESIAN_POINT('Ctrl Pts',(23.1855087234613,-5.77483158225196,-3.08640112294309));
#68739=CARTESIAN_POINT('Ctrl Pts',(23.2860786334191,-3.60155341664784,-5.46839690239391));
#68740=CARTESIAN_POINT('Ctrl Pts',(23.3866485433769,-0.554901647827081,
-6.52431114036706));
#68741=CARTESIAN_POINT('Ctrl Pts',(23.4872184533347,2.62631329291648,-5.99808554311534));
#68742=CARTESIAN_POINT('Ctrl Pts',(23.5877883632925,5.17064952093358,-4.0173293649822));
#68743=CARTESIAN_POINT('Ctrl Pts',(23.6883582732503,6.46110769116769,-1.06237427407322));
#68744=CARTESIAN_POINT('Ctrl Pts',(23.7889281832081,6.18475280820045,2.15020566377629));
#68745=CARTESIAN_POINT('Ctrl Pts',(23.8894980931659,4.40860069325718,4.84136257911875));
#68746=CARTESIAN_POINT('Ctrl Pts',(23.9900680031237,1.56336670524895,6.35849323660865));
#68747=CARTESIAN_POINT('Ctrl Pts',(24.0906379130815,-1.66098236299125,6.33369475779431));
#68748=CARTESIAN_POINT('Ctrl Pts',(24.1912078230393,-4.48254463802734,4.77298075244091));
#68749=CARTESIAN_POINT('Ctrl Pts',(24.2917777329971,-6.21709369704475,2.05482302333931));
#68750=CARTESIAN_POINT('Ctrl Pts',(24.392347642955,-6.44400288638139,-1.16162752007148));
#68751=CARTESIAN_POINT('Ctrl Pts',(24.4929175529127,-5.108246922953,-4.09638438982722));
#68752=CARTESIAN_POINT('Ctrl Pts',(24.5934874628705,-2.53374547803398,-6.03777157133502));
#68753=CARTESIAN_POINT('Ctrl Pts',(24.6940573728283,0.655187064187529,-6.51500434428101));
#68754=CARTESIAN_POINT('Ctrl Pts',(24.7946272827861,3.68523730734736,-5.41235417204141));
#68755=CARTESIAN_POINT('Ctrl Pts',(24.8951971927439,5.82162067583343,-2.99721277219148));
#68756=CARTESIAN_POINT('Ctrl Pts',(24.9957671027017,6.54626604184792,0.144750144828189));
#68757=CARTESIAN_POINT('Ctrl Pts',(25.0963370126595,5.68344752792784,3.25161127633209));
#68758=CARTESIAN_POINT('Ctrl Pts',(25.1969069226173,3.44239788095986,5.5699594724057));
#68759=CARTESIAN_POINT('Ctrl Pts',(25.2974768325752,0.366569711173962,6.53759729120178));
#68760=CARTESIAN_POINT('Ctrl Pts',(25.3980467425329,-2.79815129801792,5.91987339463266));
#68761=CARTESIAN_POINT('Ctrl Pts',(25.4986166524908,-5.28432302616933,3.86658529586191));
#68762=CARTESIAN_POINT('Ctrl Pts',(25.5991865624485,-6.48905096937149,0.875653591312175));
#68763=CARTESIAN_POINT('Ctrl Pts',(25.6997564724063,-6.12018963846224,-2.32762335534304));
#68764=CARTESIAN_POINT('Ctrl Pts',(25.8003263823641,-4.26718758866067,-4.96645364201252));
#68765=CARTESIAN_POINT('Ctrl Pts',(25.9008962923219,-1.37939622192631,-6.40092319575969));
#68766=CARTESIAN_POINT('Ctrl Pts',(26.0014662022797,1.84289754120135,-6.28317438463338));
#68767=CARTESIAN_POINT('Ctrl Pts',(26.1020361122376,4.61829023700673,-4.64176119397017));
#68768=CARTESIAN_POINT('Ctrl Pts',(26.2026060221954,6.27375152589464,-1.87472490953036));
#68769=CARTESIAN_POINT('Ctrl Pts',(26.3031759321531,6.40783347037835,1.34693055165358));
#68770=CARTESIAN_POINT('Ctrl Pts',(26.403745842111,4.98802131434215,4.241956513538));
#68771=CARTESIAN_POINT('Ctrl Pts',(26.5043157520688,2.35861828340975,6.10831167248727));
#68772=CARTESIAN_POINT('Ctrl Pts',(26.6048856620265,-0.842747650883239,
6.49340650906823));
#68773=CARTESIAN_POINT('Ctrl Pts',(26.7054555719844,-3.8397480052984,5.30385585691071));
#68774=CARTESIAN_POINT('Ctrl Pts',(26.8060254819422,-5.90561277379389,2.82812472516355));
#68775=CARTESIAN_POINT('Ctrl Pts',(26.9065953918999,-6.5393715283652,-0.333424217904892));
#68776=CARTESIAN_POINT('Ctrl Pts',(27.0071653018578,-5.58733831658651,-3.41411807515254));
#68777=CARTESIAN_POINT('Ctrl Pts',(27.1077352118155,-3.28038037277664,-5.66689123814643));
#68778=CARTESIAN_POINT('Ctrl Pts',(27.2083051217734,-0.177933012413939,
-6.54544815411231));
#68779=CARTESIAN_POINT('Ctrl Pts',(27.3088750317312,2.96766295028931,-5.83673952721545));
#68780=CARTESIAN_POINT('Ctrl Pts',(27.4094449416889,5.39360320219676,-3.7126265894016));
#68781=CARTESIAN_POINT('Ctrl Pts',(27.5100148516468,6.51159932053983,-0.68820489959331));
#68782=CARTESIAN_POINT('Ctrl Pts',(27.6105847616046,6.05053820902341,2.50310588593983));
#68783=CARTESIAN_POINT('Ctrl Pts',(27.7111546715624,4.12222679029566,5.0874156488779));
#68784=CARTESIAN_POINT('Ctrl Pts',(27.8117245815202,1.19427892345224,6.43803149635638));
#68785=CARTESIAN_POINT('Ctrl Pts',(27.912294491478,-2.02328055425881,6.22743024801059));
#68786=CARTESIAN_POINT('Ctrl Pts',(28.0128644014358,-4.75019623926001,4.50668252527276));
#68787=CARTESIAN_POINT('Ctrl Pts',(28.1134343113936,-6.32519342534584,1.69306816963788));
#68788=CARTESIAN_POINT('Ctrl Pts',(28.2140042213514,-6.36633665069315,-1.53111375969258));
#68789=CARTESIAN_POINT('Ctrl Pts',(28.3145741313092,-4.86364871857258,-4.3840019203242));
#68790=CARTESIAN_POINT('Ctrl Pts',(28.415144041267,-2.18153015896644,-6.1737733891518));
#68791=CARTESIAN_POINT('Ctrl Pts',(28.5157139512248,1.02960758626534,-6.46641012567126));
#68792=CARTESIAN_POINT('Ctrl Pts',(28.6162838611825,3.99106637814351,-5.19094797318673));
#68793=CARTESIAN_POINT('Ctrl Pts',(28.7168537711404,5.98469500894628,-2.6566854057213));
#68794=CARTESIAN_POINT('Ctrl Pts',(28.8174236810982,6.52704025187666,0.521821085680566));
#68795=CARTESIAN_POINT('Ctrl Pts',(28.917993591056,5.48658385239039,3.57378641300344));
#68796=CARTESIAN_POINT('Ctrl Pts',(29.0185635010138,3.1156355917082,5.7591116115908));
#68797=CARTESIAN_POINT('Ctrl Pts',(29.1191334109716,-0.0108516179347542,
6.54785720197586));
#68798=CARTESIAN_POINT('Ctrl Pts',(29.2197033209294,-3.13470731956994,5.74875305746505));
#68799=CARTESIAN_POINT('Ctrl Pts',(29.3202732308872,-5.49839919465536,3.55558124521044));
#68800=CARTESIAN_POINT('Ctrl Pts',(29.420843140845,-6.52873399821658,0.500184041738617));
#68801=CARTESIAN_POINT('Ctrl Pts',(29.5214130508028,-5.97585642733173,-2.67650736128206));
#68802=CARTESIAN_POINT('Ctrl Pts',(29.6219829607606,-3.97383881700753,-5.20414803320613));
#68803=CARTESIAN_POINT('Ctrl Pts',(29.7225528707184,-1.00816871435342,-6.46978728695758));
#68804=CARTESIAN_POINT('Ctrl Pts',(29.8231227806762,2.20198143367085,-6.16650869300027));
#68805=CARTESIAN_POINT('Ctrl Pts',(29.923692690634,4.87815297955871,-4.36785704929791));
#68806=CARTESIAN_POINT('Ctrl Pts',(30.0242626005918,6.37137662715756,-1.51000383111742));
#68807=CARTESIAN_POINT('Ctrl Pts',(30.1248325105496,6.31954692733444,1.71402401625443));
#68808=CARTESIAN_POINT('Ctrl Pts',(30.2254024205074,4.73523253767991,4.52240251516562));
#68809=CARTESIAN_POINT('Ctrl Pts',(30.3259723304652,2.00262833386201,6.23410229716292));
#68810=CARTESIAN_POINT('Ctrl Pts',(30.426542240423,-1.21561151699755,6.43403763859227));
#68811=CARTESIAN_POINT('Ctrl Pts',(30.5271121503808,-4.13906662141845,5.07372439126708));
#68812=CARTESIAN_POINT('Ctrl Pts',(30.6276820603386,-6.05880163317263,2.48303734666711));
#68813=CARTESIAN_POINT('Ctrl Pts',(30.7282519702964,-6.50928246447265,-0.709784117029887));
#68814=CARTESIAN_POINT('Ctrl Pts',(30.8288218802542,-5.38126790151506,-3.73048354334966));
#68815=CARTESIAN_POINT('Ctrl Pts',(30.929391790212,-2.94830050478984,-5.84654392171433));
#68816=CARTESIAN_POINT('Ctrl Pts',(31.0299617001698,0.199627226365273,-6.54482243193601));
#68817=CARTESIAN_POINT('Ctrl Pts',(31.1305316101276,3.29914552697168,-5.65598713638404));
#68818=CARTESIAN_POINT('Ctrl Pts',(31.2311015200854,5.59862387728656,-3.39557982909486));
#68819=CARTESIAN_POINT('Ctrl Pts',(31.3316714300432,6.54044075681541,-0.31174733626264));
#68820=CARTESIAN_POINT('Ctrl Pts',(31.432241340001,5.89620638301548,2.84768361725218));
#68821=CARTESIAN_POINT('Ctrl Pts',(31.5328112499588,3.82214703695784,5.31655374495108));
#68822=CARTESIAN_POINT('Ctrl Pts',(31.6333811599166,0.821220324651722,6.49616416614127));
#68823=CARTESIAN_POINT('Ctrl Pts',(31.7339510698744,-2.37885160945245,6.10046036912662));
#68824=CARTESIAN_POINT('Ctrl Pts',(31.8345209798322,-5.00205407604808,4.22540018405));
#68825=CARTESIAN_POINT('Ctrl Pts',(31.9350908897901,-6.41226273511366,1.32568409168691));
#68826=CARTESIAN_POINT('Ctrl Pts',(32.0356607997479,-6.26750320077382,-1.89550925172337));
#68827=CARTESIAN_POINT('Ctrl Pts',(32.1362307097056,-4.60287953549285,-4.65704323329943));
#68828=CARTESIAN_POINT('Ctrl Pts',(32.2368006196634,-1.8220615451456,-6.28924823971678));
#68829=CARTESIAN_POINT('Ctrl Pts',(32.3373705296213,1.40060480141665,-6.39631596196808));
#68830=CARTESIAN_POINT('Ctrl Pts',(32.4379404395791,4.28362568931618,-4.95228256957432));
#68831=CARTESIAN_POINT('Ctrl Pts',(32.5385103495368,6.12787103502435,-2.30732491712561));
#68832=CARTESIAN_POINT('Ctrl Pts',(32.6390802594947,6.48611292978621,0.897157041514567));
#68833=CARTESIAN_POINT('Ctrl Pts',(32.7396501694525,5.27147802250694,3.88407918988595));
#68834=CARTESIAN_POINT('Ctrl Pts',(32.8402200794102,2.77851423260925,5.92911547823676));
#68835=CARTESIAN_POINT('Ctrl Pts',(32.9407899893681,-0.388236866871482,
6.53634636706784));
#68836=CARTESIAN_POINT('Ctrl Pts',(33.0413598993259,-3.46084086034133,5.55851888855933));
#68837=CARTESIAN_POINT('Ctrl Pts',(33.1419298092837,-5.69419392436947,3.23275536450764));
#68838=CARTESIAN_POINT('Ctrl Pts',(33.2424997192415,-6.5467098634634,0.123051447411384));
#68839=CARTESIAN_POINT('Ctrl Pts',(33.3430696291993,-5.81165429626306,-3.01649233975588));
#68840=CARTESIAN_POINT('Ctrl Pts',(33.4436395391571,-3.66727756505767,-5.42453933121548));
#68841=CARTESIAN_POINT('Ctrl Pts',(33.5442094491149,-0.63358918122346,-6.51714020445437));
#68842=CARTESIAN_POINT('Ctrl Pts',(33.6447793590727,2.55374403364572,-6.02934018825426));
#68843=CARTESIAN_POINT('Ctrl Pts',(33.7453492690305,5.12179651869192,-4.0794303666314));
#68844=CARTESIAN_POINT('Ctrl Pts',(33.8459191789882,6.4478177569446,-1.14026219279109));
#68845=CARTESIAN_POINT('Ctrl Pts',(33.9464890889461,6.21024873960468,2.07541858123063));
#68846=CARTESIAN_POINT('Ctrl Pts',(34.0470589989039,4.46669974887087,4.78781213588376));
#68847=CARTESIAN_POINT('Ctrl Pts',(34.1476289088617,1.6399799140991,6.33916536907113));
#68848=CARTESIAN_POINT('Ctrl Pts',(34.2481988188195,-1.58443363809996,6.35327645719405));
#68849=CARTESIAN_POINT('Ctrl Pts',(34.3487687287773,-4.4246233969857,4.82672347353003));
#68850=CARTESIAN_POINT('Ctrl Pts',(34.4493386387351,-6.19184579094511,2.12969420251694));
#68851=CARTESIAN_POINT('Ctrl Pts',(34.5499085486929,-6.45755091071877,-1.08378407930465));
#68852=CARTESIAN_POINT('Ctrl Pts',(34.6504784586507,-5.15730549348813,-4.03444565484728));
#68853=CARTESIAN_POINT('Ctrl Pts',(34.7510483686085,-2.60641793364311,-6.00675763205597));
#68854=CARTESIAN_POINT('Ctrl Pts',(34.8516182785662,0.576523731431076,-6.52243605428032));
#68855=CARTESIAN_POINT('Ctrl Pts',(34.9521881885241,3.61965888792138,-5.45642934804169));
#68856=CARTESIAN_POINT('Ctrl Pts',(35.0527580984819,5.78502987999693,-3.06724322195383));
#68857=CARTESIAN_POINT('Ctrl Pts',(35.1533280084397,6.54753610609284,0.0657467450869154));
#68858=CARTESIAN_POINT('Ctrl Pts',(35.2538979183975,5.72227046276811,3.18279318304076));
#68859=CARTESIAN_POINT('Ctrl Pts',(35.3544678283553,3.50935915811661,5.52801501394688));
#68860=CARTESIAN_POINT('Ctrl Pts',(35.4550377383131,0.445431278578845,6.53269796264472));
#68861=CARTESIAN_POINT('Ctrl Pts',(35.5556076482709,-2.72651330257426,5.953207278935));
#68862=CARTESIAN_POINT('Ctrl Pts',(35.6561775582287,-5.23728075491397,3.93006895477507));
#68863=CARTESIAN_POINT('Ctrl Pts',(35.7567474681865,-6.47801213258849,0.953892292198258));
#68864=CARTESIAN_POINT('Ctrl Pts',(35.8573173781443,-6.14783114456894,-2.25360243009879));
#68865=CARTESIAN_POINT('Ctrl Pts',(35.9578872881021,-4.32680639622078,-4.91460050306248));
#68866=CARTESIAN_POINT('Ctrl Pts',(36.0584571980599,-1.4565348214281,-6.38381218466258));
#68867=CARTESIAN_POINT('Ctrl Pts',(36.1590271080177,1.76694519373391,-6.3049549068506));
#68868=CARTESIAN_POINT('Ctrl Pts',(36.2595970179755,4.56194252045255,-4.6971514916134));
#68869=CARTESIAN_POINT('Ctrl Pts',(36.3601669279333,6.25067271301243,-1.95029288310264));
#68870=CARTESIAN_POINT('Ctrl Pts',(36.4607368378911,6.42362015342513,1.26951007069249));
#68871=CARTESIAN_POINT('Ctrl Pts',(36.5613067478489,5.03884523626863,4.18145792517538));
#68872=CARTESIAN_POINT('Ctrl Pts',(36.6618766578068,2.4321546868995,6.07940583232208));
#68873=CARTESIAN_POINT('Ctrl Pts',(36.7624465677644,-0.764331280374237,
6.50310305845758));
#68874=CARTESIAN_POINT('Ctrl Pts',(36.8630164777223,-3.7754675701155,5.34980339097476));
#68875=CARTESIAN_POINT('Ctrl Pts',(36.9635863876801,-5.87105622413455,2.89918100644475));
#68876=CARTESIAN_POINT('Ctrl Pts',(37.0641562976379,-6.54291879777455,-0.254490276450008));
#68877=CARTESIAN_POINT('Ctrl Pts',(37.1647262075958,-5.62812919528632,-3.34644788637817));
#68878=CARTESIAN_POINT('Ctrl Pts',(37.2652961175535,-3.34852310779617,-5.62689476457788));
#68879=CARTESIAN_POINT('Ctrl Pts',(37.3658660275114,-0.256903049170209,
-6.54282450615985));
#68880=CARTESIAN_POINT('Ctrl Pts',(37.4664359374691,2.89701577773001,-5.87212493724906));
#68881=CARTESIAN_POINT('Ctrl Pts',(37.567005847427,5.348410772365,-3.77744012594893));
#68882=CARTESIAN_POINT('Ctrl Pts',(37.6675757573847,6.50282075876685,-0.766729335834957));
#68883=CARTESIAN_POINT('Ctrl Pts',(37.7681456673425,6.08030230898233,2.42991265819638));
#68884=CARTESIAN_POINT('Ctrl Pts',(37.8687155773003,4.18331578336822,5.03730292435361));
#68885=CARTESIAN_POINT('Ctrl Pts',(37.9692854872581,1.27187878140549,6.4231515676099));
#68886=CARTESIAN_POINT('Ctrl Pts',(38.0698553972159,-1.94798773017833,6.25139148495386));
#68887=CARTESIAN_POINT('Ctrl Pts',(38.1704253071738,-4.69546889407762,4.56367434857359));
#68888=CARTESIAN_POINT('Ctrl Pts',(38.2709952171315,-6.30430289315735,1.76927011120597));
#68889=CARTESIAN_POINT('Ctrl Pts',(38.3715651270894,-6.38434886757117,-1.45418060509064));
#68890=CARTESIAN_POINT('Ctrl Pts',(38.4721350370471,-4.91619573742957,-4.32499377645314));
#68891=CARTESIAN_POINT('Ctrl Pts',(38.572704947005,-2.25586937296357,-6.14699968010442));
#68892=CARTESIAN_POINT('Ctrl Pts',(38.6732748569627,0.95150337252903,-6.47836345284401));
#68893=CARTESIAN_POINT('Ctrl Pts',(38.7738447669205,3.92813736926474,-5.23872966502996));
#68894=CARTESIAN_POINT('Ctrl Pts',(38.8744146768784,5.95220143540704,-2.72870844309488));
#68895=CARTESIAN_POINT('Ctrl Pts',(38.9749845868361,6.53286177728884,0.44302222734022));
#68896=CARTESIAN_POINT('Ctrl Pts',(39.075554496794,5.52930876185287,3.50732038901156));
#68897=CARTESIAN_POINT('Ctrl Pts',(39.1761244067517,3.18490313145511,5.72109637554957));
#68898=CARTESIAN_POINT('Ctrl Pts',(39.2766943167096,0.068161233335458,6.54751141590063));
#68899=CARTESIAN_POINT('Ctrl Pts',(39.3772642266674,-3.06510970519291,5.78616057418141));
#68900=CARTESIAN_POINT('Ctrl Pts',(39.4778341366252,-5.45509417874633,3.62167077411613));
#68901=CARTESIAN_POINT('Ctrl Pts',(39.5784040465829,-6.52222300985525,0.578928928965803));
#68902=CARTESIAN_POINT('Ctrl Pts',(39.6789739565408,-6.00771837559096,-2.6042026831001));
#68903=CARTESIAN_POINT('Ctrl Pts',(39.7795438664985,-4.0363472068621,-5.15581738628664));
#68904=CARTESIAN_POINT('Ctrl Pts',(39.8801137764564,-1.0861653150726,-6.45715081157412));
#68905=CARTESIAN_POINT('Ctrl Pts',(39.9806836864142,2.12741073061978,-6.19263072355546));
#68906=CARTESIAN_POINT('Ctrl Pts',(40.081253596372,4.82509150547297,-4.42640301586869));
#68907=CARTESIAN_POINT('Ctrl Pts',(40.1818235063298,6.35269174382611,-1.58677638720847));
#68908=CARTESIAN_POINT('Ctrl Pts',(40.2823934162875,6.3397697028807,1.63764214940717));
#68909=CARTESIAN_POINT('Ctrl Pts',(40.3829633262454,4.78945896644229,4.46493387452094));
#68910=CARTESIAN_POINT('Ctrl Pts',(40.4835332362032,2.07770855354523,6.20948297860651));
#68911=CARTESIAN_POINT('Ctrl Pts',(40.584103146161,-1.13788439503546,6.44823780568102));
#68912=CARTESIAN_POINT('Ctrl Pts',(40.6846730561188,-4.07754135734353,5.12330051570587));
#68913=CARTESIAN_POINT('Ctrl Pts',(40.7852429660766,-6.02839805056031,2.5559672609561));
#68914=CARTESIAN_POINT('Ctrl Pts',(40.8858128760344,-6.51737340593419,-0.631185854325582));
#68915=CARTESIAN_POINT('Ctrl Pts',(40.9863827859922,-5.42589132071097,-3.66527694327624));
#68916=CARTESIAN_POINT('Ctrl Pts',(41.08695269595,-3.01863526097817,-5.81054152865792));
#68917=CARTESIAN_POINT('Ctrl Pts',(41.1875226059078,0.12063725101407,-6.54675479522083));
#68918=CARTESIAN_POINT('Ctrl Pts',(41.2880925158656,3.23065533348335,-5.69538565957693));
#68919=CARTESIAN_POINT('Ctrl Pts',(41.3886624258234,5.55724227862367,-3.46289040423696));
#68920=CARTESIAN_POINT('Ctrl Pts',(41.4892323357812,6.5362027550313,-0.39064720682494));
#68921=CARTESIAN_POINT('Ctrl Pts',(41.589802245739,5.93013968989465,2.77632760196186));
#68922=CARTESIAN_POINT('Ctrl Pts',(41.6903721556968,3.88602285479283,5.27004535721532));
#68923=CARTESIAN_POINT('Ctrl Pts',(41.7909420656546,0.899548822603686,6.48578164995024));
#68924=CARTESIAN_POINT('Ctrl Pts',(41.8915119756124,-2.30506502470944,6.12872147571909));
#68925=CARTESIAN_POINT('Ctrl Pts',(41.9920818855702,-4.9507025877966,4.28545161940524));
#68926=CARTESIAN_POINT('Ctrl Pts',(42.092651795528,-6.39579903504983,1.40296343442533));
#68927=CARTESIAN_POINT('Ctrl Pts',(42.1932217054858,-6.28991972199076,-1.81974217569154));
#68928=CARTESIAN_POINT('Ctrl Pts',(42.2937916154436,-4.65874029089223,-4.60116187468952));
#68929=CARTESIAN_POINT('Ctrl Pts',(42.3943615254014,-1.89782034962951,-6.26680377988744));
#68930=CARTESIAN_POINT('Ctrl Pts',(42.4949314353592,1.3233193927202,-6.41275116310696));
#68931=CARTESIAN_POINT('Ctrl Pts',(42.595501345317,4.22355532148648,-5.00361190955315));
#68932=CARTESIAN_POINT('Ctrl Pts',(42.6960712552748,6.09958272054981,-2.3811010751854));
#68933=CARTESIAN_POINT('Ctrl Pts',(42.7966411652326,6.4964665605756,0.818824720194698));
#68934=CARTESIAN_POINT('Ctrl Pts',(42.8972110751904,5.31796285200656,3.82018622579545));
#68935=CARTESIAN_POINT('Ctrl Pts',(42.9977809851482,2.84985772968081,5.8951558601667));
#68936=CARTESIAN_POINT('Ctrl Pts',(43.098350895106,-0.309335438853322,6.54055527316669));
#68937=CARTESIAN_POINT('Ctrl Pts',(43.1989208050639,-3.39351502975027,5.59987566272126));
#68938=CARTESIAN_POINT('Ctrl Pts',(43.2994907150216,-5.65477014716779,3.30123102459958));
#68939=CARTESIAN_POINT('Ctrl Pts',(43.4000606249794,-6.5447483716855,0.202040704806857));
#68940=CARTESIAN_POINT('Ctrl Pts',(43.5006305349372,-5.84763074997661,-2.94614431197915));
#68941=CARTESIAN_POINT('Ctrl Pts',(43.601200444895,-3.73246770520662,-5.37989186923573));
#68942=CARTESIAN_POINT('Ctrl Pts',(43.7017703548528,-0.712184454939265,
-6.50902027936784));
#68943=CARTESIAN_POINT('Ctrl Pts',(43.8023402648106,2.48080291258205,-6.05971687490459));
#68944=CARTESIAN_POINT('Ctrl Pts',(43.9029101747684,5.07219770934852,-4.14093734465504));
#68945=CARTESIAN_POINT('Ctrl Pts',(44.0034800847263,6.4335889278912,-1.21798407296426));
#68946=CARTESIAN_POINT('Ctrl Pts',(44.104049994684,6.23484036963815,2.00032928794473));
#68947=CARTESIAN_POINT('Ctrl Pts',(44.2046199046419,4.5241483888772,4.73356451846799));
#68948=CARTESIAN_POINT('Ctrl Pts',(44.3051898145997,1.71635431833013,6.3189144280508));
#68949=CARTESIAN_POINT('Ctrl Pts',(44.4057597245574,-1.5076541969249,6.37193302833398));
#68950=CARTESIAN_POINT('Ctrl Pts',(44.5063296345153,-4.36605786725757,4.87976335438894));
#68951=CARTESIAN_POINT('Ctrl Pts',(44.606899544473,-6.16569626320814,2.20425526764484));
#68952=CARTESIAN_POINT('Ctrl Pts',(44.7074694544309,-6.47015862293896,-1.00578282401701));
#68953=CARTESIAN_POINT('Ctrl Pts',(44.8080393643886,-5.20561308630515,-3.97191944666151));
#68954=CARTESIAN_POINT('Ctrl Pts',(44.9086092743465,-2.67871085738329,-5.97486902263271));
#68955=CARTESIAN_POINT('Ctrl Pts',(45.0091791843042,0.497776448542833,-6.52891800395401));
#68956=CARTESIAN_POINT('Ctrl Pts',(45.1097490942621,3.5535533941975,-5.49970998959639));
#68957=CARTESIAN_POINT('Ctrl Pts',(45.2103190042198,5.74759670075998,-3.13682703706976));
#68958=CARTESIAN_POINT('Ctrl Pts',(45.3108889141777,6.5478527550843,-0.0132662283243582));
#68959=CARTESIAN_POINT('Ctrl Pts',(45.4114588241354,5.76026015288009,3.11351162936983));
#68960=CARTESIAN_POINT('Ctrl Pts',(45.5120287340933,3.5758094221995,5.48526559714188));
#68961=CARTESIAN_POINT('Ctrl Pts',(45.612598644051,0.524227984794888,6.5268473794809));
#68962=CARTESIAN_POINT('Ctrl Pts',(45.7131685540089,-2.65447828765195,5.98567429079325));
#68963=CARTESIAN_POINT('Ctrl Pts',(45.8137384639667,-5.18947586039424,3.99298033922837));
#68964=CARTESIAN_POINT('Ctrl Pts',(45.9143083739244,-6.46603000424065,1.03199209267258));
#68965=CARTESIAN_POINT('Ctrl Pts',(46.0148782838823,-6.17457743820275,-2.17925334798793));
#68966=CARTESIAN_POINT('Ctrl Pts',(46.1154481938401,-4.38579515865401,-4.86203172772514));
#68967=CARTESIAN_POINT('Ctrl Pts',(46.2160181037979,-1.53346132854994,-6.36577159886536));
#68968=CARTESIAN_POINT('Ctrl Pts',(46.3165880137557,1.69073555368001,-6.32581733711948));
#68969=CARTESIAN_POINT('Ctrl Pts',(46.4171579237134,4.5049305195762,-4.75185781656709));
#68970=CARTESIAN_POINT('Ctrl Pts',(46.5177278336713,6.22668371244857,-2.02557686603268));
#68971=CARTESIAN_POINT('Ctrl Pts',(46.618297743629,6.43847146516005,1.19190473084001));
#68972=CARTESIAN_POINT('Ctrl Pts',(46.7188676535869,5.0889354299911,4.12035045650976));
#68973=CARTESIAN_POINT('Ctrl Pts',(46.8194375635447,2.50533693375088,6.04961474339174));
#68974=CARTESIAN_POINT('Ctrl Pts',(46.9200074735025,-0.685803612258052,
6.51185266268309));
#68975=CARTESIAN_POINT('Ctrl Pts',(47.0205773834603,-3.71063737265382,5.3949719168633));
#68976=CARTESIAN_POINT('Ctrl Pts',(47.1211472934181,-5.83564476440411,2.96981512535072));
#68977=CARTESIAN_POINT('Ctrl Pts',(47.2217172033759,-6.54551332427677,-0.175519277557393));
#68978=CARTESIAN_POINT('Ctrl Pts',(47.3222871133337,-5.66810053757789,-3.27829040674986));
#68979=CARTESIAN_POINT('Ctrl Pts',(47.4228570232914,-3.41617824977988,-5.58607893435188));
#68980=CARTESIAN_POINT('Ctrl Pts',(47.5234269332493,-0.335835677154444,
-6.53924812903053));
#68981=CARTESIAN_POINT('Ctrl Pts',(47.6239968432071,2.82594675808396,-5.90665528159158));
#68982=CARTESIAN_POINT('Ctrl Pts',(47.724566753165,5.30243953714302,-3.84170361298495));
#68983=CARTESIAN_POINT('Ctrl Pts',(47.8251366631226,6.49309529293691,-0.8451421252781));
#68984=CARTESIAN_POINT('Ctrl Pts',(47.9257065730806,6.10918102963623,2.3563656002861));
#68985=CARTESIAN_POINT('Ctrl Pts',(48.0262764830382,4.24379562560702,4.98645669620802));
#68986=CARTESIAN_POINT('Ctrl Pts',(48.1268463929962,1.34929343554907,6.40733633578441));
#68987=CARTESIAN_POINT('Ctrl Pts',(48.2274163029538,-1.87241125111904,6.27444242955194));
#68988=CARTESIAN_POINT('Ctrl Pts',(48.3279862129117,-4.64005782121609,4.62000163537314));
#68989=CARTESIAN_POINT('Ctrl Pts',(48.4285561228695,-6.28249436396308,1.84521442164623));
#68990=CARTESIAN_POINT('Ctrl Pts',(48.5291260328273,-6.40143143160032,-1.3770357009164));
#68991=CARTESIAN_POINT('Ctrl Pts',(48.6296959427851,-4.96802688761027,-4.26535585139861));
#68992=CARTESIAN_POINT('Ctrl Pts',(48.7302658527429,-2.32988009999474,-6.11933087965732));
#68993=CARTESIAN_POINT('Ctrl Pts',(48.8308357627007,0.873260606241912,-6.4893734372946));
#68994=CARTESIAN_POINT('Ctrl Pts',(48.9314056726586,3.86463636719267,-5.28574852262676));
#68995=CARTESIAN_POINT('Ctrl Pts',(49.0319755826163,5.91884113588903,-2.80033414134579));
#68996=CARTESIAN_POINT('Ctrl Pts',(49.1325454925741,6.53773202424047,0.364158858603563));
#68997=CARTESIAN_POINT('Ctrl Pts',(49.2331154025319,5.57122852458084,3.44034364881996));
#68998=CARTESIAN_POINT('Ctrl Pts',(49.3336853124897,3.25370690358363,5.68224806574399));
#68999=CARTESIAN_POINT('Ctrl Pts',(49.4342552224475,0.147164159351603,6.54621221816718));
#69000=CARTESIAN_POINT('Ctrl Pts',(49.5348251324053,-2.99506576684006,5.82272554285206));
#69001=CARTESIAN_POINT('Ctrl Pts',(49.6353950423632,-5.41099482281151,3.68723293576444));
#69002=CARTESIAN_POINT('Ctrl Pts',(49.7359649523209,-6.51476229219069,0.657589515829798));
#69003=CARTESIAN_POINT('Ctrl Pts',(49.8365348622787,-6.03870551380784,-2.53151879562165));
#69004=CARTESIAN_POINT('Ctrl Pts',(49.9371047722365,-4.09826784661749,-5.10673597833884));
#69005=CARTESIAN_POINT('Ctrl Pts',(50.0376746821944,-1.16400375452887,-6.44357408233362));
#69006=CARTESIAN_POINT('Ctrl Pts',(50.1382445921521,2.05253024602511,-6.21785101817589));
#69007=CARTESIAN_POINT('Ctrl Pts',(50.23881450211,4.77132742879492,-4.48430443461504));
#69008=CARTESIAN_POINT('Ctrl Pts',(50.3393844120677,6.33308181737752,-1.66331788587789));
#69009=CARTESIAN_POINT('Ctrl Pts',(50.4399543220256,6.35906931694452,1.56102181835299));
#69010=CARTESIAN_POINT('Ctrl Pts',(50.5405242319833,4.84298798122161,4.4068150754056));
#69011=CARTESIAN_POINT('Ctrl Pts',(50.6410941419412,2.15248622903544,6.18395947018508));
#69012=CARTESIAN_POINT('Ctrl Pts',(50.7416640518989,-1.05999158076988,6.46149901677434));
#69013=CARTESIAN_POINT('Ctrl Pts',(50.8422339618568,-4.01542234470967,5.17213061403956));
#69014=CARTESIAN_POINT('Ctrl Pts',(50.9428038718145,-5.99711664664814,2.62852498971853));
#69015=CARTESIAN_POINT('Ctrl Pts',(51.0433737817724,-6.52451532426444,-0.552495681899622));
#69016=CARTESIAN_POINT('Ctrl Pts',(51.1439436917301,-5.46972465223643,-3.59953662626124));
#69017=CARTESIAN_POINT('Ctrl Pts',(51.244513601688,-3.08853046053694,-5.77369303733878));
#69018=CARTESIAN_POINT('Ctrl Pts',(51.3450835116457,0.0416297091470886,
-6.54773385702222));
#69019=CARTESIAN_POINT('Ctrl Pts',(51.4456534216036,3.16169471019899,-5.73395485285493));
#69020=CARTESIAN_POINT('Ctrl Pts',(51.5462233315613,5.51505146570521,-3.52969673282309));
#69021=CARTESIAN_POINT('Ctrl Pts',(51.6467932415192,6.53101298829235,-0.469490193545743));
#69022=CARTESIAN_POINT('Ctrl Pts',(51.7473631514769,5.96320948330187,2.7045673135158));
#69023=CARTESIAN_POINT('Ctrl Pts',(51.8479330614348,3.94933281191226,5.22276957521886));
#69024=CARTESIAN_POINT('Ctrl Pts',(51.9485029713926,0.977746333333282,6.47445471084103));
#69025=CARTESIAN_POINT('Ctrl Pts',(52.0490728813504,-2.23094278940758,6.15609015248089));
#69026=CARTESIAN_POINT('Ctrl Pts',(52.1496427913082,-4.89863020617543,4.34487903148253));
#69027=CARTESIAN_POINT('Ctrl Pts',(52.2502127012659,-6.37840401482964,1.4800384855472));
#69028=CARTESIAN_POINT('Ctrl Pts',(52.3507826112238,-6.31142034059575,-1.74371011907603));
#69029=CARTESIAN_POINT('Ctrl Pts',(52.4513525211815,-4.71392266682865,-4.54461052085449));
#69030=CARTESIAN_POINT('Ctrl Pts',(52.5519224311394,-1.97330280421664,-6.24344678346548));
#69031=CARTESIAN_POINT('Ctrl Pts',(52.6524923410972,1.24584128970535,-6.42825257560717));
#69032=CARTESIAN_POINT('Ctrl Pts',(52.7530622510549,4.16286994340196,-5.05421265182165));
#69033=CARTESIAN_POINT('Ctrl Pts',(52.8536321610128,6.07040621920021,-2.45453051071525));
#69034=CARTESIAN_POINT('Ctrl Pts',(52.9542020709706,6.50587421269849,0.740373166181634));
#69035=CARTESIAN_POINT('Ctrl Pts',(53.0547719809284,5.36367330951959,3.75573698786384));
#69036=CARTESIAN_POINT('Ctrl Pts',(53.1553418908862,2.92078624704449,5.86033782254595));
#69037=CARTESIAN_POINT('Ctrl Pts',(53.2559118008439,-0.230388968113506,
6.54381178096489));
#69038=CARTESIAN_POINT('Ctrl Pts',(53.3564817108019,-3.3256950527764,5.64041701372739));
#69039=CARTESIAN_POINT('Ctrl Pts',(53.4570516207595,-5.61452295792606,3.36922597975961));
#69040=CARTESIAN_POINT('Ctrl Pts',(53.5576215307174,-6.54183386340029,0.281000538852744));
#69041=CARTESIAN_POINT('Ctrl Pts',(53.6581914406752,-5.88275571877033,-2.87536727679449));
#69042=CARTESIAN_POINT('Ctrl Pts',(53.758761350633,-3.79711431694879,-5.3344610304885));
#69043=CARTESIAN_POINT('Ctrl Pts',(53.8593312605908,-0.790676078238258,
-6.49995252258906));
#69044=CARTESIAN_POINT('Ctrl Pts',(53.9599011705485,2.40750065640528,-6.08921122850316));
#69045=CARTESIAN_POINT('Ctrl Pts',(54.0604710805064,5.02186010893717,-4.20184124741766));
#69046=CARTESIAN_POINT('Ctrl Pts',(54.1610409904642,6.41842367956464,-1.29552878373208));
#69047=CARTESIAN_POINT('Ctrl Pts',(54.261610900422,6.25852332754194,1.92494908307514));
#69048=CARTESIAN_POINT('Ctrl Pts',(54.3621808103799,4.58093979359666,4.67862691169207));
#69049=CARTESIAN_POINT('Ctrl Pts',(54.4627507203375,1.79247577205141,6.2977447603908));
#69050=CARTESIAN_POINT('Ctrl Pts',(54.5633206302954,-1.43064930071301,6.38965901879497));
#69051=CARTESIAN_POINT('Ctrl Pts',(54.6638905402532,-4.30686815961765,4.93209802530353));
#69052=CARTESIAN_POINT('Ctrl Pts',(54.7644604502111,-6.13862625381269,2.27848488382594));
#69053=CARTESIAN_POINT('Ctrl Pts',(54.8650303601687,-6.48186856325177,-0.927614594694319));
#69054=CARTESIAN_POINT('Ctrl Pts',(54.9656002701267,-5.25307563387778,-3.90885517127706));
#69055=CARTESIAN_POINT('Ctrl Pts',(55.0661701800844,-2.7507861368141,-5.94202989429022));
#69056=CARTESIAN_POINT('Ctrl Pts',(55.1667400900422,0.419316711856036,-6.53462427730853));
#69057=CARTESIAN_POINT('Ctrl Pts',(55.2337866966808,2.46375373567196,-5.87263820593936));
#69058=CARTESIAN_POINT('Ctrl Pts',(55.26731,3.34571636511773,-5.31774159209371));
#69059=CARTESIAN_POINT('Ctrl Pts',(18.5943714011907,3.74381434373823,-4.74963296131605));
#69060=CARTESIAN_POINT('Ctrl Pts',(18.62789470451,4.53155453436587,-4.12871066082871));
#69061=CARTESIAN_POINT('Ctrl Pts',(18.6949413111485,5.79137112877805,-2.48801589670783));
#69062=CARTESIAN_POINT('Ctrl Pts',(18.7955112211063,6.27641633085685,0.578268110945115));
#69063=CARTESIAN_POINT('Ctrl Pts',(18.8960811310641,5.23951763712497,3.50352722589919));
#69064=CARTESIAN_POINT('Ctrl Pts',(18.9966510410219,2.93200383757313,5.57957477908284));
#69065=CARTESIAN_POINT('Ctrl Pts',(19.0972209509797,-0.0865001488795471,
6.30238201346393));
#69066=CARTESIAN_POINT('Ctrl Pts',(19.1977908609375,-3.0840371900228,5.49696820322353));
#69067=CARTESIAN_POINT('Ctrl Pts',(19.2983607708953,-5.33369313625283,3.35849264924486));
#69068=CARTESIAN_POINT('Ctrl Pts',(19.3989306808531,-6.28993550566722,0.405611930459287));
#69069=CARTESIAN_POINT('Ctrl Pts',(19.499500590811,-5.72087269424937,-2.64564282898167));
#69070=CARTESIAN_POINT('Ctrl Pts',(19.6000705007687,-3.76450381040718,-5.05532458279635));
#69071=CARTESIAN_POINT('Ctrl Pts',(19.7006404107266,-0.895245670559178,
-6.23909800156691));
#69072=CARTESIAN_POINT('Ctrl Pts',(19.8012103206843,2.19110860890456,-5.90989372465953));
#69073=CARTESIAN_POINT('Ctrl Pts',(19.9017802306422,4.74612102111524,-4.14754622731969));
#69074=CARTESIAN_POINT('Ctrl Pts',(20.0023501405999,6.1502031282558,-1.37942186984454));
#69075=CARTESIAN_POINT('Ctrl Pts',(20.1029200505578,6.06286629306327,1.7232108632711));
#69076=CARTESIAN_POINT('Ctrl Pts',(20.2034899605155,4.50528958965082,4.40796656825658));
#69077=CARTESIAN_POINT('Ctrl Pts',(20.3040598704734,1.85518404477503,6.02379411217868));
#69078=CARTESIAN_POINT('Ctrl Pts',(20.4046297804312,-1.24480203689863,6.17885680142634));
#69079=CARTESIAN_POINT('Ctrl Pts',(20.505199690389,-4.04292469468554,4.83555201887475));
#69080=CARTESIAN_POINT('Ctrl Pts',(20.6057696003468,-5.86064159504332,2.31963004270374));
#69081=CARTESIAN_POINT('Ctrl Pts',(20.7063395103045,-6.25715795321971,-0.758800226299075));
#69082=CARTESIAN_POINT('Ctrl Pts',(20.8069094202624,-5.13631889428152,-3.65322209143408));
#69083=CARTESIAN_POINT('Ctrl Pts',(20.9074793302201,-2.76992692486838,-5.66174074531242));
#69084=CARTESIAN_POINT('Ctrl Pts',(21.008049240178,0.268169939340544,-6.29729214167012));
#69085=CARTESIAN_POINT('Ctrl Pts',(21.1086191501357,3.24123582413446,-5.40575561485436));
#69086=CARTESIAN_POINT('Ctrl Pts',(21.2091890600936,5.42830481171089,-3.20332800471673));
#69087=CARTESIAN_POINT('Ctrl Pts',(21.3097589700514,6.29901455529484,-0.224096111028122));
#69088=CARTESIAN_POINT('Ctrl Pts',(21.4103288800092,5.64221869158862,2.8094788967154));
#69089=CARTESIAN_POINT('Ctrl Pts',(21.510898789967,3.61718965215762,5.16175769046553));
#69090=CARTESIAN_POINT('Ctrl Pts',(21.6114686999248,0.714995235858073,6.26231468767699));
#69091=CARTESIAN_POINT('Ctrl Pts',(21.7120386098826,-2.36058490964819,5.84426576390167));
#69092=CARTESIAN_POINT('Ctrl Pts',(21.8126085198403,-4.86372524662418,4.00898742329443));
#69093=CARTESIAN_POINT('Ctrl Pts',(21.9131784297982,-6.18741639812789,1.20153308358827));
#69094=CARTESIAN_POINT('Ctrl Pts',(22.0137483397559,-6.0106643993911,-1.89729199457321));
#69095=CARTESIAN_POINT('Ctrl Pts',(22.1143182497138,-4.37633145795426,-4.5360253972944));
#69096=CARTESIAN_POINT('Ctrl Pts',(22.2148881596715,-1.68074190523514,-6.07477654591226));
#69097=CARTESIAN_POINT('Ctrl Pts',(22.3154580696294,1.42242611267267,-6.14039961148838));
#69098=CARTESIAN_POINT('Ctrl Pts',(22.4160279795871,4.18065702272256,-4.71698105711057));
#69099=CARTESIAN_POINT('Ctrl Pts',(22.516597889545,5.92508220359168,-2.14969865689606));
#69100=CARTESIAN_POINT('Ctrl Pts',(22.6171677995028,6.23268005057049,0.938883817093518));
#69101=CARTESIAN_POINT('Ctrl Pts',(22.7177377094606,5.0288583505557,3.79978777365601));
#69102=CARTESIAN_POINT('Ctrl Pts',(22.8183076194184,2.60554282951664,5.73924646607323));
#69103=CARTESIAN_POINT('Ctrl Pts',(22.9188775293762,-0.449614584754226,
6.28694283097562));
#69104=CARTESIAN_POINT('Ctrl Pts',(23.019447439334,-3.39574084926331,5.31006097134712));
#69105=CARTESIAN_POINT('Ctrl Pts',(23.1200173492918,-5.51840288097714,3.04549389721973));
#69106=CARTESIAN_POINT('Ctrl Pts',(23.2205872592497,-6.30285696445349,0.0423971746650429));
#69107=CARTESIAN_POINT('Ctrl Pts',(23.3211571692074,-5.55887365972991,-2.97098082624923));
#69108=CARTESIAN_POINT('Ctrl Pts',(23.4217270791652,-3.46686827775967,-5.26389853430357));
#69109=CARTESIAN_POINT('Ctrl Pts',(23.522296989123,-0.53415032281234,-6.28032537910409));
#69110=CARTESIAN_POINT('Ctrl Pts',(23.6228668990808,2.52809862560505,-5.77377872575607));
#69111=CARTESIAN_POINT('Ctrl Pts',(23.7234368090386,4.97728583357301,-3.86709570164651));
#69112=CARTESIAN_POINT('Ctrl Pts',(23.8240067189964,6.2194855114899,-1.02264529879458));
#69113=CARTESIAN_POINT('Ctrl Pts',(23.9245766289542,5.95346530678201,2.06979570869266));
#69114=CARTESIAN_POINT('Ctrl Pts',(24.025146538912,4.24373489009314,4.66031303856144));
#69115=CARTESIAN_POINT('Ctrl Pts',(24.1257164488698,1.50490241568538,6.12070846831016));
#69116=CARTESIAN_POINT('Ctrl Pts',(24.2262863588276,-1.59886759906292,6.09683736337508));
#69117=CARTESIAN_POINT('Ctrl Pts',(24.3268562687854,-4.31491359738955,4.59448844615397));
#69118=CARTESIAN_POINT('Ctrl Pts',(24.4274261787432,-5.98459676275057,1.97798003580794));
#69119=CARTESIAN_POINT('Ctrl Pts',(24.5279960887011,-6.20302036485712,-1.11818683051956));
#69120=CARTESIAN_POINT('Ctrl Pts',(24.6285659986588,-4.91721686822363,-3.94319435301338));
#69121=CARTESIAN_POINT('Ctrl Pts',(24.7291359086166,-2.4389925139272,-5.81198063931621));
#69122=CARTESIAN_POINT('Ctrl Pts',(24.8297058185745,0.630685425441865,-6.27136662370451));
#69123=CARTESIAN_POINT('Ctrl Pts',(24.9302757285322,3.54742269205338,-5.20995160041667));
#69124=CARTESIAN_POINT('Ctrl Pts',(25.03084563849,5.60391300956513,-2.88512779890356));
#69125=CARTESIAN_POINT('Ctrl Pts',(25.1314155484478,6.30145924626639,0.139337010242921));
#69126=CARTESIAN_POINT('Ctrl Pts',(25.2319854584056,5.47090704022486,3.13001271435079));
#69127=CARTESIAN_POINT('Ctrl Pts',(25.3325553683634,3.31366458644248,5.36166302963329));
#69128=CARTESIAN_POINT('Ctrl Pts',(25.4331252783213,0.352861322945316,6.29311467570303));
#69129=CARTESIAN_POINT('Ctrl Pts',(25.533695188279,-2.69351050761294,5.69849143020836));
#69130=CARTESIAN_POINT('Ctrl Pts',(25.6342650982368,-5.08670835872616,3.72198891831302));
#69131=CARTESIAN_POINT('Ctrl Pts',(25.7348350081946,-6.24638381163271,0.842907297721581));
#69132=CARTESIAN_POINT('Ctrl Pts',(25.8354049181524,-5.89131656728466,-2.24057861696856));
#69133=CARTESIAN_POINT('Ctrl Pts',(25.9359748281103,-4.10761012678435,-4.78072614579817));
#69134=CARTESIAN_POINT('Ctrl Pts',(26.036544738068,-1.3278117664874,-6.1615516996579));
#69135=CARTESIAN_POINT('Ctrl Pts',(26.1371146480258,1.77397980416429,-6.04820627039098));
#69136=CARTESIAN_POINT('Ctrl Pts',(26.2376845579837,4.44558279939882,-4.46817602702365));
#69137=CARTESIAN_POINT('Ctrl Pts',(26.3382544679414,6.03913579266429,-1.80461694343717));
#69138=CARTESIAN_POINT('Ctrl Pts',(26.4388243778993,6.16820355486997,1.2965601954668));
#69139=CARTESIAN_POINT('Ctrl Pts',(26.539394287857,4.80148726478621,4.0833226030863));
#69140=CARTESIAN_POINT('Ctrl Pts',(26.6399641978149,2.27041444624971,5.87988279449855));
#69141=CARTESIAN_POINT('Ctrl Pts',(26.7405341077726,-0.811231921064463,
6.25057646981665));
#69142=CARTESIAN_POINT('Ctrl Pts',(26.8411040177305,-3.69615524585221,5.10551073187969));
#69143=CARTESIAN_POINT('Ctrl Pts',(26.9416739276882,-5.68476410527724,2.72236303643196));
#69144=CARTESIAN_POINT('Ctrl Pts',(27.0422438376461,-6.29482256278049,-0.320955351862344));
#69145=CARTESIAN_POINT('Ctrl Pts',(27.1428137476039,-5.37839196757329,-3.2864423436176));
#69146=CARTESIAN_POINT('Ctrl Pts',(27.2433836575617,-3.15770595010358,-5.45496989610942));
#69147=CARTESIAN_POINT('Ctrl Pts',(27.3439535675194,-0.171278957977622,
-6.3006719445892));
#69148=CARTESIAN_POINT('Ctrl Pts',(27.4445234774773,2.8566830340161,-5.61846647030524));
#69149=CARTESIAN_POINT('Ctrl Pts',(27.5450933874351,5.19190184937557,-3.57378771350929));
#69150=CARTESIAN_POINT('Ctrl Pts',(27.6456632973929,6.26808893559948,-0.662468512606323));
#69151=CARTESIAN_POINT('Ctrl Pts',(27.7462332073507,5.82426985069124,2.4094987323318));
#69152=CARTESIAN_POINT('Ctrl Pts',(27.8468031173085,3.9680703406889,4.89716460884505));
#69153=CARTESIAN_POINT('Ctrl Pts',(27.9473730272663,1.14961718889825,6.19727228333315));
#69154=CARTESIAN_POINT('Ctrl Pts',(28.0479429372241,-1.94761714157679,5.99454676390265));
#69155=CARTESIAN_POINT('Ctrl Pts',(28.1485128471819,-4.57255599178413,4.33814881450354));
#69156=CARTESIAN_POINT('Ctrl Pts',(28.2490827571397,-6.08865395017118,1.62975351199023));
#69157=CARTESIAN_POINT('Ctrl Pts',(28.3496526670975,-6.12825856692962,-1.47385561424216));
#69158=CARTESIAN_POINT('Ctrl Pts',(28.4502225770553,-4.68176575658838,-4.22005602275799));
#69159=CARTESIAN_POINT('Ctrl Pts',(28.5507924870131,-2.09994878047266,-5.94289647850027));
#69160=CARTESIAN_POINT('Ctrl Pts',(28.6513623969709,0.991103967211534,-6.22458965402194));
#69161=CARTESIAN_POINT('Ctrl Pts',(28.7519323069287,3.84181485601765,-4.99682519674859));
#69162=CARTESIAN_POINT('Ctrl Pts',(28.8525022168865,5.7608889493839,-2.55733493067413));
#69163=CARTESIAN_POINT('Ctrl Pts',(28.9530721268443,6.28295243166296,0.502306854661562));
#69164=CARTESIAN_POINT('Ctrl Pts',(29.0536420368021,5.2814053578094,3.44013966014196));
#69165=CARTESIAN_POINT('Ctrl Pts',(29.1542119467599,2.99912203107227,5.5437415594088));
#69166=CARTESIAN_POINT('Ctrl Pts',(29.2547818567177,-0.0104458064696189,
6.30299090273076));
#69167=CARTESIAN_POINT('Ctrl Pts',(29.3553517666755,-3.01748054493469,5.53377037793584));
#69168=CARTESIAN_POINT('Ctrl Pts',(29.4559216766333,-5.2927788487869,3.42261530011971));
#69169=CARTESIAN_POINT('Ctrl Pts',(29.5564915865911,-6.28458283798409,0.481478958309967));
#69170=CARTESIAN_POINT('Ctrl Pts',(29.6570614965489,-5.7523808989193,-2.57641561641906));
#69171=CARTESIAN_POINT('Ctrl Pts',(29.7576314065067,-3.825231543681,-5.00953162201891));
#69172=CARTESIAN_POINT('Ctrl Pts',(29.8582013164645,-0.970466831969092,
-6.22784052162765));
#69173=CARTESIAN_POINT('Ctrl Pts',(29.9587712264223,2.11963525108966,-5.93590345584543));
#69174=CARTESIAN_POINT('Ctrl Pts',(30.0593411363801,4.69572761040196,-4.2045149118166));
#69175=CARTESIAN_POINT('Ctrl Pts',(30.1599110463379,6.13311006640879,-1.45353512103927));
#69176=CARTESIAN_POINT('Ctrl Pts',(30.2604809562957,6.08321861086852,1.64992568534537));
#69177=CARTESIAN_POINT('Ctrl Pts',(30.3610508662535,4.55815187880167,4.3532809333371));
#69178=CARTESIAN_POINT('Ctrl Pts',(30.4616207762113,1.92773723991327,6.00096930242366));
#69179=CARTESIAN_POINT('Ctrl Pts',(30.5621906861691,-1.1701520202026,6.19342778147895));
#69180=CARTESIAN_POINT('Ctrl Pts',(30.6627605961269,-3.98428042271975,4.88398535500585));
#69181=CARTESIAN_POINT('Ctrl Pts',(30.7633305060847,-5.83222425251021,2.39018068421849));
#69182=CARTESIAN_POINT('Ctrl Pts',(30.8639004160425,-6.26585872161285,-0.683240744955771));
#69183=CARTESIAN_POINT('Ctrl Pts',(30.9644703260003,-5.18002784455525,-3.5909768816315));
#69184=CARTESIAN_POINT('Ctrl Pts',(31.0650402359581,-2.83804467430954,-5.62790421572743));
#69185=CARTESIAN_POINT('Ctrl Pts',(31.1656101459159,0.192161886385956,-6.30006962217086));
#69186=CARTESIAN_POINT('Ctrl Pts',(31.2661800558737,3.17576935505136,-5.44447356851846));
#69187=CARTESIAN_POINT('Ctrl Pts',(31.3667499658315,5.38925548891016,-3.26859736125931));
#69188=CARTESIAN_POINT('Ctrl Pts',(31.4673198757894,6.2958518059339,-0.300089107597089));
#69189=CARTESIAN_POINT('Ctrl Pts',(31.5678897857471,5.67570947966844,2.74119049633208));
#69190=CARTESIAN_POINT('Ctrl Pts',(31.668459695705,3.67921249039688,5.11773376459612));
#69191=CARTESIAN_POINT('Ctrl Pts',(31.7690296056627,0.790509639375698,6.25323100043758));
#69192=CARTESIAN_POINT('Ctrl Pts',(31.8695995156205,-2.28989111870072,5.87232510163352));
#69193=CARTESIAN_POINT('Ctrl Pts',(31.9701694255784,-4.81499525169616,4.06738542074917));
#69194=CARTESIAN_POINT('Ctrl Pts',(32.0707393355361,-6.17246718104128,1.27610827665518));
#69195=CARTESIAN_POINT('Ctrl Pts',(32.171309245494,-6.03312113242065,-1.8246240260171));
#69196=CARTESIAN_POINT('Ctrl Pts',(32.2718791554517,-4.43074840267172,-4.48288657306889));
#69197=CARTESIAN_POINT('Ctrl Pts',(32.3724490654096,-1.75392299939023,-6.05405298514883));
#69198=CARTESIAN_POINT('Ctrl Pts',(32.4730189753674,1.34822722141622,-6.15711675983263));
#69199=CARTESIAN_POINT('Ctrl Pts',(32.5735888853251,4.12343350162191,-4.76708502047968));
#69200=CARTESIAN_POINT('Ctrl Pts',(32.674158795283,5.89871070725407,-2.22103926730387));
#69201=CARTESIAN_POINT('Ctrl Pts',(32.7747287052407,6.24355564415645,0.863606596258802));
#69202=CARTESIAN_POINT('Ctrl Pts',(32.8752986151986,5.07434371198264,3.73882860364601));
#69203=CARTESIAN_POINT('Ctrl Pts',(32.9758685251564,2.67460779779369,5.70738789313997));
#69204=CARTESIAN_POINT('Ctrl Pts',(33.0764384351141,-0.37371820498118,6.2919105316307));
#69205=CARTESIAN_POINT('Ctrl Pts',(33.177008345072,-3.33141786475548,5.35065028245797));
#69206=CARTESIAN_POINT('Ctrl Pts',(33.2775782550298,-5.4812515601066,3.11186194578239));
#69207=CARTESIAN_POINT('Ctrl Pts',(33.3781481649876,-6.30188647055037,0.118449766034587));
#69208=CARTESIAN_POINT('Ctrl Pts',(33.4787180749453,-5.59431933673029,-2.9036863800116));
#69209=CARTESIAN_POINT('Ctrl Pts',(33.5792879849032,-3.53013457950368,-5.22168107848151));
#69210=CARTESIAN_POINT('Ctrl Pts',(33.679857894861,-0.609895225588482,-6.2734226103925));
#69211=CARTESIAN_POINT('Ctrl Pts',(33.7804278048187,2.45824319551665,-5.8038645596254));
#69212=CARTESIAN_POINT('Ctrl Pts',(33.8809977147766,4.93025975783522,-3.92687434928215));
#69213=CARTESIAN_POINT('Ctrl Pts',(33.9815676247343,6.20669257298772,-1.09762048960406));
#69214=CARTESIAN_POINT('Ctrl Pts',(34.0821375346922,5.97800778208965,1.99780539393979));
#69215=CARTESIAN_POINT('Ctrl Pts',(34.1827074446499,4.29966125007543,4.60876518922143));
#69216=CARTESIAN_POINT('Ctrl Pts',(34.2832773546078,1.57865056618961,6.10210339347416));
#69217=CARTESIAN_POINT('Ctrl Pts',(34.3838472645656,-1.52518152104951,6.11568677767498));
#69218=CARTESIAN_POINT('Ctrl Pts',(34.4844171745234,-4.25915840235411,4.64622138284819));
#69219=CARTESIAN_POINT('Ctrl Pts',(34.5849870844812,-5.96029303749356,2.05005130228134));
#69220=CARTESIAN_POINT('Ctrl Pts',(34.685556994439,-6.21606174183198,-1.04325445434579));
#69221=CARTESIAN_POINT('Ctrl Pts',(34.7861269043968,-4.96444082474036,-3.88357190385742));
#69222=CARTESIAN_POINT('Ctrl Pts',(34.8866968143546,-2.50894728118225,-5.7821265097737));
#69223=CARTESIAN_POINT('Ctrl Pts',(34.9872667243123,0.554963818288801,-6.27852041449017));
#69224=CARTESIAN_POINT('Ctrl Pts',(35.0878366342702,3.48429666955357,-5.25237852342321));
#69225=CARTESIAN_POINT('Ctrl Pts',(35.188406544228,5.56869057783411,-2.95253936182418));
#69226=CARTESIAN_POINT('Ctrl Pts',(35.2889764541858,6.30268181467842,0.0632880533866562));
#69227=CARTESIAN_POINT('Ctrl Pts',(35.3895463641436,5.50827813699247,3.06376817013139));
#69228=CARTESIAN_POINT('Ctrl Pts',(35.4901162741014,3.37812175276964,5.32128714299879));
#69229=CARTESIAN_POINT('Ctrl Pts',(35.5906861840592,0.428773751484242,6.28839856440554));
#69230=CARTESIAN_POINT('Ctrl Pts',(35.691256094017,-2.62455151543532,5.73057874717778));
#69231=CARTESIAN_POINT('Ctrl Pts',(35.7918260039748,-5.04142529915106,3.78309851680594));
#69232=CARTESIAN_POINT('Ctrl Pts',(35.8923959139326,-6.23575778762611,0.918220152708348));
#69233=CARTESIAN_POINT('Ctrl Pts',(35.9929658238904,-5.91792438052098,-2.16932580799077));
#69234=CARTESIAN_POINT('Ctrl Pts',(36.0935357338482,-4.16499940545854,-4.73081212767));
#69235=CARTESIAN_POINT('Ctrl Pts',(36.194105643806,-1.40206565992333,-6.145080578808));
#69236=CARTESIAN_POINT('Ctrl Pts',(36.2946755537638,1.70086780120493,-6.06917227944665));
#69237=CARTESIAN_POINT('Ctrl Pts',(36.3952454637217,4.39134228469678,-4.52149492683709));
#69238=CARTESIAN_POINT('Ctrl Pts',(36.4958153736794,6.01692004434307,-1.87735894670202));
#69239=CARTESIAN_POINT('Ctrl Pts',(36.5963852836372,6.18339987277349,1.2220349619239));
#69240=CARTESIAN_POINT('Ctrl Pts',(36.696955193595,4.85041055490425,4.02508644424602));
#69241=CARTESIAN_POINT('Ctrl Pts',(36.7975251035529,2.34120085284323,5.85205792874828));
#69242=CARTESIAN_POINT('Ctrl Pts',(36.8980950135106,-0.735748040659395,
6.25991040314837));
#69243=CARTESIAN_POINT('Ctrl Pts',(36.9986649234685,-3.63427866765513,5.14973999349544));
#69244=CARTESIAN_POINT('Ctrl Pts',(37.0992348334262,-5.65149984623585,2.79076206846371));
#69245=CARTESIAN_POINT('Ctrl Pts',(37.199804743384,-6.29823717707749,-0.244973255802475));
#69246=CARTESIAN_POINT('Ctrl Pts',(37.3003746533419,-5.41765741418102,-3.22130277641656));
#69247=CARTESIAN_POINT('Ctrl Pts',(37.4009445632996,-3.2233003920205,-5.41646914673941));
#69248=CARTESIAN_POINT('Ctrl Pts',(37.5015144732574,-0.247295799504477,
-6.29814641162992));
#69249=CARTESIAN_POINT('Ctrl Pts',(37.6020843832152,2.78867781151207,-5.65252859332527));
#69250=CARTESIAN_POINT('Ctrl Pts',(37.7026542931731,5.14839945381081,-3.63617745699796));
#69251=CARTESIAN_POINT('Ctrl Pts',(37.8032242031308,6.25963866045032,-0.738056417474464));
#69252=CARTESIAN_POINT('Ctrl Pts',(37.9037941130887,5.8529208804071,2.33904266794645));
#69253=CARTESIAN_POINT('Ctrl Pts',(38.0043640230464,4.02687482522731,4.84892591990536));
#69254=CARTESIAN_POINT('Ctrl Pts',(38.1049339330043,1.22431509137923,6.18294881038171));
#69255=CARTESIAN_POINT('Ctrl Pts',(38.205503842962,-1.87513999820277,6.01761193680014));
#69256=CARTESIAN_POINT('Ctrl Pts',(38.3060737529198,-4.51987525239489,4.39300934867749));
#69257=CARTESIAN_POINT('Ctrl Pts',(38.4066436628776,-6.06854464871948,1.70310577512895));
#69258=CARTESIAN_POINT('Ctrl Pts',(38.5072135728354,-6.14559719170687,-1.39979948280604));
#69259=CARTESIAN_POINT('Ctrl Pts',(38.6077834827933,-4.73234770601166,-4.16325457114813));
#69260=CARTESIAN_POINT('Ctrl Pts',(38.7083533927511,-2.17150797534923,-5.9171240098357));
#69261=CARTESIAN_POINT('Ctrl Pts',(38.8089233027088,0.915920570039041,-6.23609596976817));
#69262=CARTESIAN_POINT('Ctrl Pts',(38.9094932126667,3.78123916564354,-5.04282002524212));
#69263=CARTESIAN_POINT('Ctrl Pts',(39.0100631226244,5.72961051857859,-2.62666456559893));
#69264=CARTESIAN_POINT('Ctrl Pts',(39.1106330325823,6.28855625297138,0.426454790093798));
#69265=CARTESIAN_POINT('Ctrl Pts',(39.21120294254,5.3225325093882,3.3761592262933));
#69266=CARTESIAN_POINT('Ctrl Pts',(39.3117728524979,3.06579921406697,5.50714795641135));
#69267=CARTESIAN_POINT('Ctrl Pts',(39.4123427624557,0.0656122484624124,
6.30265804781056));
#69268=CARTESIAN_POINT('Ctrl Pts',(39.5129126724135,-2.95048563091339,5.5697789881245));
#69269=CARTESIAN_POINT('Ctrl Pts',(39.6134825823713,-5.25109328465533,3.48623331844373));
#69270=CARTESIAN_POINT('Ctrl Pts',(39.7140524923291,-6.27831533716003,0.557279070090006));
#69271=CARTESIAN_POINT('Ctrl Pts',(39.8146224022869,-5.78305132495739,-2.50681487303874));
#69272=CARTESIAN_POINT('Ctrl Pts',(39.9151923122446,-3.88540234466897,-4.96300836739375));
#69273=CARTESIAN_POINT('Ctrl Pts',(40.0157622222025,-1.04554664046408,-6.21567660495573));
#69274=CARTESIAN_POINT('Ctrl Pts',(40.1163321321602,2.04785322401683,-5.96104861644857));
#69275=CARTESIAN_POINT('Ctrl Pts',(40.2169020421181,4.64465044452441,-4.26087146989424));
#69276=CARTESIAN_POINT('Ctrl Pts',(40.3174719520758,6.1151239304831,-1.52743665977094));
#69277=CARTESIAN_POINT('Ctrl Pts',(40.4180418620337,6.10268512737375,1.57640022548551));
#69278=CARTESIAN_POINT('Ctrl Pts',(40.5186117719914,4.61035043424262,4.2979614130723));
#69279=CARTESIAN_POINT('Ctrl Pts',(40.6191816819493,2.00000972952951,5.97727065779749));
#69280=CARTESIAN_POINT('Ctrl Pts',(40.7197515919071,-1.0953316129288,6.20709691341278));
#69281=CARTESIAN_POINT('Ctrl Pts',(40.8203215018649,-3.9250559821447,4.93170751077247));
#69282=CARTESIAN_POINT('Ctrl Pts',(40.9208914118227,-5.80295765449124,2.46038328212514));
#69283=CARTESIAN_POINT('Ctrl Pts',(41.0214613217805,-6.27364709097608,-0.607581774469037));
#69284=CARTESIAN_POINT('Ctrl Pts',(41.1220312317383,-5.22298250843454,-3.52820877377832));
#69285=CARTESIAN_POINT('Ctrl Pts',(41.2226011416961,-2.90574916369074,-5.59324818262967));
#69286=CARTESIAN_POINT('Ctrl Pts',(41.323171051654,0.116125851895876,-6.30192972202175));
#69287=CARTESIAN_POINT('Ctrl Pts',(41.4237409616116,3.10984044836217,-5.48239872870535));
#69288=CARTESIAN_POINT('Ctrl Pts',(41.5243108715695,5.34942141314046,-3.333390763084));
#69289=CARTESIAN_POINT('Ctrl Pts',(41.6248807815273,6.29177229016759,-0.376038406893155));
#69290=CARTESIAN_POINT('Ctrl Pts',(41.7254506914851,5.70837380296712,2.67250293926466));
#69291=CARTESIAN_POINT('Ctrl Pts',(41.8260206014429,3.74069958247899,5.07296462321797));
#69292=CARTESIAN_POINT('Ctrl Pts',(41.9265905114007,0.865908933341185,6.24323675299435));
#69293=CARTESIAN_POINT('Ctrl Pts',(42.0271604213585,-2.21886388673261,5.89952934452685));
#69294=CARTESIAN_POINT('Ctrl Pts',(42.1277303313163,-4.76556412433542,4.12519114849563));
#69295=CARTESIAN_POINT('Ctrl Pts',(42.2283002412741,-6.15661916412113,1.35049765003709));
#69296=CARTESIAN_POINT('Ctrl Pts',(42.3288701512319,-6.05469935640187,-1.75169036600829));
#69297=CARTESIAN_POINT('Ctrl Pts',(42.4294400611897,-4.484520166814,-4.42909497620203));
#69298=CARTESIAN_POINT('Ctrl Pts',(42.5300099711475,-1.82684869717725,-6.03244786735878));
#69299=CARTESIAN_POINT('Ctrl Pts',(42.6305798811053,1.27383200892127,-6.17293734358508));
#69300=CARTESIAN_POINT('Ctrl Pts',(42.7311497910632,4.06560954940742,-4.81649482783347));
#69301=CARTESIAN_POINT('Ctrl Pts',(42.8317197010208,5.87148027395556,-2.29205646250919));
#69302=CARTESIAN_POINT('Ctrl Pts',(42.9322896109788,6.25352208640813,0.788203621905611));
#69303=CARTESIAN_POINT('Ctrl Pts',(43.0328595209364,5.11909017611791,3.67732500651664));
#69304=CARTESIAN_POINT('Ctrl Pts',(43.1334294308944,2.74328330477867,5.67469824259427));
#69305=CARTESIAN_POINT('Ctrl Pts',(43.2339993408521,-0.297767406472493,
6.29596203978567));
#69306=CARTESIAN_POINT('Ctrl Pts',(43.3345692508099,-3.26660977798073,5.39046046207373));
#69307=CARTESIAN_POINT('Ctrl Pts',(43.4351391607677,-5.44330209031999,3.17777686257191));
#69308=CARTESIAN_POINT('Ctrl Pts',(43.5357090707255,-6.29999833150725,0.1944851094179));
#69309=CARTESIAN_POINT('Ctrl Pts',(43.6362789806833,-5.62895040052328,-2.83596911535165));
#69310=CARTESIAN_POINT('Ctrl Pts',(43.7368488906411,-3.59288684297432,-5.17870327093198));
#69311=CARTESIAN_POINT('Ctrl Pts',(43.8374188005989,-0.685551318864139,
-6.26560634128757));
#69312=CARTESIAN_POINT('Ctrl Pts',(43.9379887105567,2.38802980992837,-5.83310526749458));
#69313=CARTESIAN_POINT('Ctrl Pts',(44.0385586205146,4.88251576549779,-3.98608118763844));
#69314=CARTESIAN_POINT('Ctrl Pts',(44.1391285304723,6.19299585094358,-1.17243585111297));
#69315=CARTESIAN_POINT('Ctrl Pts',(44.2396984404301,6.001679773644,1.92552417004097));
#69316=CARTESIAN_POINT('Ctrl Pts',(44.3402683503879,4.35496151765379,4.55654623750647));
#69317=CARTESIAN_POINT('Ctrl Pts',(44.4408382603457,1.65216884250822,6.08260976478227));
#69318=CARTESIAN_POINT('Ctrl Pts',(44.5414081703036,-1.4512733547112,6.13364566018324));
#69319=CARTESIAN_POINT('Ctrl Pts',(44.6419780802613,-4.20278301271083,4.69727776300792));
#69320=CARTESIAN_POINT('Ctrl Pts',(44.7425479902192,-5.93512140800427,2.12182405185462));
#69321=CARTESIAN_POINT('Ctrl Pts',(44.8431179001769,-6.22819797097945,-0.968170165346456));
#69322=CARTESIAN_POINT('Ctrl Pts',(44.9436878101347,-5.01094188740351,-3.82338395087974));
#69323=CARTESIAN_POINT('Ctrl Pts',(45.0442577200926,-2.57853670969462,-5.75143041960318));
#69324=CARTESIAN_POINT('Ctrl Pts',(45.1448276300503,0.479161400436802,-6.28475996256904));
#69325=CARTESIAN_POINT('Ctrl Pts',(45.2453975400082,3.42066328343813,-5.29404062471357));
#69326=CARTESIAN_POINT('Ctrl Pts',(45.3459674499659,5.53265726481079,-3.0195209926271));
#69327=CARTESIAN_POINT('Ctrl Pts',(45.4465373599238,6.30298662213694,-0.0127701191187959));
#69328=CARTESIAN_POINT('Ctrl Pts',(45.5471072698816,5.5448471493865,2.99707749728301));
#69329=CARTESIAN_POINT('Ctrl Pts',(45.6476771798394,3.4420870160732,5.28013640056389));
#69330=CARTESIAN_POINT('Ctrl Pts',(45.7482470897972,0.504623744409411,6.28276677200082));
#69331=CARTESIAN_POINT('Ctrl Pts',(45.8488169997549,-2.55521035087901,5.76183160961339));
#69332=CARTESIAN_POINT('Ctrl Pts',(45.9493869097128,-4.99540813567764,3.84365724184467));
#69333=CARTESIAN_POINT('Ctrl Pts',(46.0499568196706,-6.22422374776511,0.993399301658971));
#69334=CARTESIAN_POINT('Ctrl Pts',(46.1505267296283,-5.9436704590098,-2.09775711403243));
#69335=CARTESIAN_POINT('Ctrl Pts',(46.2510966395862,-4.22178220042662,-4.68020923538044));
#69336=CARTESIAN_POINT('Ctrl Pts',(46.3516665495439,-1.47611539247118,-6.12771464600704));
#69337=CARTESIAN_POINT('Ctrl Pts',(46.4522364595018,1.62750812747607,-6.08925452988943));
#69338=CARTESIAN_POINT('Ctrl Pts',(46.5528063694595,4.33646232751603,-4.57415543207854));
#69339=CARTESIAN_POINT('Ctrl Pts',(46.6533762794174,5.99382814608451,-1.94982757955281));
#69340=CARTESIAN_POINT('Ctrl Pts',(46.7539461893752,6.19769579888664,1.147331782547));
#69341=CARTESIAN_POINT('Ctrl Pts',(46.8545160993329,4.89862755561304,3.96626417503526));
#69342=CARTESIAN_POINT('Ctrl Pts',(46.9550860092908,2.41164634698237,5.82338091935141));
#69343=CARTESIAN_POINT('Ctrl Pts',(47.0556559192485,-0.660157024777184,
6.26833280365816));
#69344=CARTESIAN_POINT('Ctrl Pts',(47.1562258292064,-3.57187288631038,5.19321937903841));
#69345=CARTESIAN_POINT('Ctrl Pts',(47.2567957391642,-5.61741264768391,2.85875472547407));
#69346=CARTESIAN_POINT('Ctrl Pts',(47.357365649122,-6.30073467762402,-0.168955488119712));
#69347=CARTESIAN_POINT('Ctrl Pts',(47.4579355590798,-5.45613397209338,-3.15569414128618));
#69348=CARTESIAN_POINT('Ctrl Pts',(47.5585054690376,-3.28842547512672,-5.37717968170277));
#69349=CARTESIAN_POINT('Ctrl Pts',(47.6590753789954,-0.323276631212769,
-6.29470377813694));
#69350=CARTESIAN_POINT('Ctrl Pts',(47.7596452889532,2.72026651748448,-5.68576762703438));
#69351=CARTESIAN_POINT('Ctrl Pts',(47.8602151989109,5.10414737737517,-3.69803772084787));
#69352=CARTESIAN_POINT('Ctrl Pts',(47.9607851088689,6.25027689204883,-0.813536850732643));
#69353=CARTESIAN_POINT('Ctrl Pts',(48.0613550188265,5.88071964081822,2.26824600536938));
#69354=CARTESIAN_POINT('Ctrl Pts',(48.1619249287844,4.08509293898134,4.79998115774056));
#69355=CARTESIAN_POINT('Ctrl Pts',(48.2624948387422,1.29883471600662,6.16772501132107));
#69356=CARTESIAN_POINT('Ctrl Pts',(48.3630647487,-1.80238980752552,6.03980085901079));
#69357=CARTESIAN_POINT('Ctrl Pts',(48.4636346586578,-4.46653635428158,4.4472301976242));
#69358=CARTESIAN_POINT('Ctrl Pts',(48.5642045686156,-6.04755168004692,1.77621004161703));
#69359=CARTESIAN_POINT('Ctrl Pts',(48.6647744785734,-6.16204092930681,-1.32553952046974));
#69360=CARTESIAN_POINT('Ctrl Pts',(48.7653443885312,-4.78224055767135,-4.10584688990502));
#69361=CARTESIAN_POINT('Ctrl Pts',(48.8659142984891,-2.24275096749041,-5.89048992296909));
#69362=CARTESIAN_POINT('Ctrl Pts',(48.9664842084468,0.840603801682614,-6.2466942204158));
#69363=CARTESIAN_POINT('Ctrl Pts',(49.0670541184046,3.72011287256346,-5.08808054674523));
#69364=CARTESIAN_POINT('Ctrl Pts',(49.1676240283624,5.69749777422752,-2.69561172045457));
#69365=CARTESIAN_POINT('Ctrl Pts',(49.2681939383202,6.29324437021086,0.350540627586432));
#69366=CARTESIAN_POINT('Ctrl Pts',(49.3687638482779,5.36288462382333,3.31168717519316));
#69367=CARTESIAN_POINT('Ctrl Pts',(49.4693337582359,3.13202997268351,5.46975243361084));
#69368=CARTESIAN_POINT('Ctrl Pts',(49.5699036681935,0.141660749309164,6.30140743539763));
#69369=CARTESIAN_POINT('Ctrl Pts',(49.6704735781515,-2.88306108382702,5.60497655853276));
#69370=CARTESIAN_POINT('Ctrl Pts',(49.7710434881091,-5.20864308595681,3.54934369114824));
#69371=CARTESIAN_POINT('Ctrl Pts',(49.8716133980671,-6.27113362349142,0.632998034037112));
#69372=CARTESIAN_POINT('Ctrl Pts',(49.9721833080248,-5.81287965570103,-2.43684910142515));
#69373=CARTESIAN_POINT('Ctrl Pts',(50.0727532179827,-3.94500737529666,-4.91576242750141));
#69374=CARTESIAN_POINT('Ctrl Pts',(50.1733231279404,-1.12047420235831,-6.20260759653784));
#69375=CARTESIAN_POINT('Ctrl Pts',(50.2738930378982,1.97577300011552,-5.98532576279636));
#69376=CARTESIAN_POINT('Ctrl Pts',(50.374462947856,4.59289695086342,-4.3166075839169));
#69377=CARTESIAN_POINT('Ctrl Pts',(50.4750328578138,6.09624734472443,-1.60111578179717));
#69378=CARTESIAN_POINT('Ctrl Pts',(50.5756027677717,6.12126300531428,1.50264521912207));
#69379=CARTESIAN_POINT('Ctrl Pts',(50.6761726777294,4.66187765647411,4.24201604792428));
#69380=CARTESIAN_POINT('Ctrl Pts',(50.7767425876873,2.07199098901695,5.95270163675385));
#69381=CARTESIAN_POINT('Ctrl Pts',(50.877312497645,-1.02035170964748,6.21986220292691));
#69382=CARTESIAN_POINT('Ctrl Pts',(50.9778824076029,-3.86525999707042,4.97871153912603));
#69383=CARTESIAN_POINT('Ctrl Pts',(51.0784523175607,-5.77284606253051,2.53022761290473));
#69384=CARTESIAN_POINT('Ctrl Pts',(51.1790222275184,-6.28052192725839,-0.531834331353529));
#69385=CARTESIAN_POINT('Ctrl Pts',(51.2795921374763,-5.26517663107943,-3.4649269080768));
#69386=CARTESIAN_POINT('Ctrl Pts',(51.380162047434,-2.97303053427876,-5.55777769229983));
#69387=CARTESIAN_POINT('Ctrl Pts',(51.4807319573919,0.0400729078145031,
-6.30287217043457));
#69388=CARTESIAN_POINT('Ctrl Pts',(51.5813018673496,3.04345870425864,-5.51952557293213));
#69389=CARTESIAN_POINT('Ctrl Pts',(51.6818717773075,5.30880838481668,-3.39769877535954));
#69390=CARTESIAN_POINT('Ctrl Pts',(51.7824416872652,6.28677660203117,-0.451932949598734));
#69391=CARTESIAN_POINT('Ctrl Pts',(51.8830115972231,5.74020690509067,2.6034262274029));
#69392=CARTESIAN_POINT('Ctrl Pts',(51.9835815071808,3.80164197500026,5.02745678536328));
#69393=CARTESIAN_POINT('Ctrl Pts',(52.0841514171387,0.941182138535105,6.2323334006519));
#69394=CARTESIAN_POINT('Ctrl Pts',(52.1847213270964,-2.14751355632885,5.92587453125411));
#69395=CARTESIAN_POINT('Ctrl Pts',(52.2852912370543,-4.71543906242315,4.18239618918938));
#69396=CARTESIAN_POINT('Ctrl Pts',(52.3858611470121,-6.13987465506746,1.42469037157386));
#69397=CARTESIAN_POINT('Ctrl Pts',(52.4864310569698,-6.07539592923327,-1.6785016347362));
#69398=CARTESIAN_POINT('Ctrl Pts',(52.5870009669278,-4.53763892044433,-4.37465843952072));
#69399=CARTESIAN_POINT('Ctrl Pts',(52.6875708768854,-1.89950837955927,-6.00996433856127));
#69400=CARTESIAN_POINT('Ctrl Pts',(52.7881407868433,1.19925130818209,-6.18785905903403));
#69401=CARTESIAN_POINT('Ctrl Pts',(52.888710696801,4.00719358610876,-4.8652032844097));
#69402=CARTESIAN_POINT('Ctrl Pts',(52.9892806067589,5.84339486877529,-2.36273990135964));
#69403=CARTESIAN_POINT('Ctrl Pts',(53.0898505167167,6.26257792619167,0.712685873732938));
#69404=CARTESIAN_POINT('Ctrl Pts',(53.1904204266745,5.1630912269926,3.61528593818628));
#69405=CARTESIAN_POINT('Ctrl Pts',(53.2909903366323,2.81155935080371,5.64118227430033));
#69406=CARTESIAN_POINT('Ctrl Pts',(53.3915602465901,-0.221773249677871,
6.29909676590961));
#69407=CARTESIAN_POINT('Ctrl Pts',(53.4921301565479,-3.20132602411989,5.42948571242569));
#69408=CARTESIAN_POINT('Ctrl Pts',(53.5927000665056,-5.40456000114086,3.24322905106435));
#69409=CARTESIAN_POINT('Ctrl Pts',(53.6932699764635,-6.2971928153451,0.27049212977903));
#69410=CARTESIAN_POINT('Ctrl Pts',(53.7938398864213,-5.66276182186868,-2.76783888661719));
#69411=CARTESIAN_POINT('Ctrl Pts',(53.8944097963791,-3.65511590404492,-5.13497138208737));
#69412=CARTESIAN_POINT('Ctrl Pts',(53.9949797063369,-0.761107637875617,
-6.25687768598526));
#69413=CARTESIAN_POINT('Ctrl Pts',(54.0955496162947,2.31746879438081,-5.86149663839339));
#69414=CARTESIAN_POINT('Ctrl Pts',(54.1961195262525,4.83406061022007,-4.04470750357852));
#69415=CARTESIAN_POINT('Ctrl Pts',(54.2966894362103,6.17839772833774,-1.24708066871483));
#69416=CARTESIAN_POINT('Ctrl Pts',(54.3972593461681,6.0244770741368,1.85296291360496));
#69417=CARTESIAN_POINT('Ctrl Pts',(54.4978292561259,4.40962912818019,4.50366309955075));
#69418=CARTESIAN_POINT('Ctrl Pts',(54.5983991660837,1.725443627756,6.06223176652131));
#69419=CARTESIAN_POINT('Ctrl Pts',(54.6989690760415,-1.37714816454321,6.15070876238158));
#69420=CARTESIAN_POINT('Ctrl Pts',(54.7995389859993,-4.14580678716376,4.74765530553779));
#69421=CARTESIAN_POINT('Ctrl Pts',(54.9001088959571,-5.90906371955852,2.19327774747913));
#69422=CARTESIAN_POINT('Ctrl Pts',(55.0006788059149,-6.23947000165856,-0.892925146540183));
#69423=CARTESIAN_POINT('Ctrl Pts',(55.1012487158727,-5.05662950647384,-3.76267805248054));
#69424=CARTESIAN_POINT('Ctrl Pts',(55.2018186258305,-2.64791663301169,-5.71981935650092));
#69425=CARTESIAN_POINT('Ctrl Pts',(55.3023885357883,0.403635775592951,-6.29025284183206));
#69426=CARTESIAN_POINT('Ctrl Pts',(55.3694351424269,2.37161821088939,-5.65302266761336));
#69427=CARTESIAN_POINT('Ctrl Pts',(55.4029584457461,3.22059861141916,-5.11887719052968));
#69428=CARTESIAN_POINT('Ctrl Pts',(18.7300198469368,3.59837006536955,-4.56511341115994));
#69429=CARTESIAN_POINT('Ctrl Pts',(18.7635431502561,4.3555071616532,-3.96831345959956));
#69430=CARTESIAN_POINT('Ctrl Pts',(18.8305897568946,5.56638086023038,-2.39135841227044));
#69431=CARTESIAN_POINT('Ctrl Pts',(18.9311596668524,6.03258243308101,0.555802844140216));
#69432=CARTESIAN_POINT('Ctrl Pts',(19.0317295768102,5.03596644794646,3.36741791535919));
#69433=CARTESIAN_POINT('Ctrl Pts',(19.1322994867681,2.81809776660485,5.36281263415837));
#69434=CARTESIAN_POINT('Ctrl Pts',(19.2328693967258,-0.0831396853048251,
6.05753936909375));
#69435=CARTESIAN_POINT('Ctrl Pts',(19.3334393066836,-2.96422474143937,5.28341525958718));
#69436=CARTESIAN_POINT('Ctrl Pts',(19.4340092166414,-5.12648330210607,3.22801781931831));
#69437=CARTESIAN_POINT('Ctrl Pts',(19.5345791265992,-6.04557639845419,0.389854222115132));
#69438=CARTESIAN_POINT('Ctrl Pts',(19.635149036557,-5.49862123510697,-2.54286166069909));
#69439=CARTESIAN_POINT('Ctrl Pts',(19.7357189465149,-3.61825576233384,-4.85892915066333));
#69440=CARTESIAN_POINT('Ctrl Pts',(19.8362888564726,-0.860466071849947,
-5.99671389188823));
#69441=CARTESIAN_POINT('Ctrl Pts',(19.9368587664304,2.10598574190594,-5.68029894535209));
#69442=CARTESIAN_POINT('Ctrl Pts',(20.0374286763883,4.56173790710718,-3.98641727896731));
#69443=CARTESIAN_POINT('Ctrl Pts',(20.137998586346,5.91127251533532,-1.32583240199046));
#69444=CARTESIAN_POINT('Ctrl Pts',(20.2385684963039,5.82732864833066,1.65626546014106));
#69445=CARTESIAN_POINT('Ctrl Pts',(20.3391384062616,4.33026258963291,4.23672049200133));
#69446=CARTESIAN_POINT('Ctrl Pts',(20.4397083162195,1.7831115860847,5.78977439131494));
#69447=CARTESIAN_POINT('Ctrl Pts',(20.5402782261772,-1.19644244495693,5.93881301556665));
#69448=CARTESIAN_POINT('Ctrl Pts',(20.6408481361351,-3.88586021158666,4.64769458009025));
#69449=CARTESIAN_POINT('Ctrl Pts',(20.7414180460928,-5.63296022270332,2.22951421786122));
#69450=CARTESIAN_POINT('Ctrl Pts',(20.8419879560507,-6.01407222845162,-0.729321427083321));
#69451=CARTESIAN_POINT('Ctrl Pts',(20.9425578660084,-4.93677689607866,-3.51129725167865));
#69452=CARTESIAN_POINT('Ctrl Pts',(21.0431277759663,-2.66231741602744,-5.44178651644161));
#69453=CARTESIAN_POINT('Ctrl Pts',(21.1436976859241,0.257751745561017,-6.05264723486437));
#69454=CARTESIAN_POINT('Ctrl Pts',(21.2442675958819,3.11531633075669,-5.19574620940539));
#69455=CARTESIAN_POINT('Ctrl Pts',(21.3448375058397,5.2174193874844,-3.07888120066958));
#69456=CARTESIAN_POINT('Ctrl Pts',(21.4454074157975,6.05430273405806,-0.215390151233893));
#69457=CARTESIAN_POINT('Ctrl Pts',(21.5459773257553,5.42302287933666,2.70033282449942));
#69458=CARTESIAN_POINT('Ctrl Pts',(21.6465472357131,3.47666464467147,4.96122741479645));
#69459=CARTESIAN_POINT('Ctrl Pts',(21.7471171456709,0.687218226485192,6.01902862778194));
#69460=CARTESIAN_POINT('Ctrl Pts',(21.8476870556287,-2.26887802004612,5.61722057987778));
#69461=CARTESIAN_POINT('Ctrl Pts',(21.9482569655865,-4.67477329983176,3.85324137682038));
#69462=CARTESIAN_POINT('Ctrl Pts',(22.0488268755443,-5.947040078587,1.15485445686342));
#69463=CARTESIAN_POINT('Ctrl Pts',(22.1493967855021,-5.77715475766761,-1.82358367475042));
#69464=CARTESIAN_POINT('Ctrl Pts',(22.2499666954599,-4.20631438115428,-4.35980433503075));
#69465=CARTESIAN_POINT('Ctrl Pts',(22.3505366054177,-1.61544638812712,-5.83877619711054));
#69466=CARTESIAN_POINT('Ctrl Pts',(22.4511065153755,1.36716596339831,-5.90184985757714));
#69467=CARTESIAN_POINT('Ctrl Pts',(22.5516764253333,4.01824174569531,-4.53373000806282));
#69468=CARTESIAN_POINT('Ctrl Pts',(22.6522463352911,5.69489736367894,-2.06618453435812));
#69469=CARTESIAN_POINT('Ctrl Pts',(22.7528162452489,5.99054527330138,0.902408910297553));
#69470=CARTESIAN_POINT('Ctrl Pts',(22.8533861552067,4.83349111098141,3.65216897102551));
#69471=CARTESIAN_POINT('Ctrl Pts',(22.9539560651645,2.50431951505622,5.51628120017159));
#69472=CARTESIAN_POINT('Ctrl Pts',(23.0545259751223,-0.432147407480051,
6.0426999868491));
#69473=CARTESIAN_POINT('Ctrl Pts',(23.1550958850801,-3.26381895570729,5.10376922844516));
#69474=CARTESIAN_POINT('Ctrl Pts',(23.2556657950379,-5.30401721676446,2.92717882561419));
#69475=CARTESIAN_POINT('Ctrl Pts',(23.3562357049957,-6.05799586860639,0.0407500773712745));
#69476=CARTESIAN_POINT('Ctrl Pts',(23.4568056149535,-5.34291573720787,-2.85556052955536));
#69477=CARTESIAN_POINT('Ctrl Pts',(23.5573755249113,-3.3321831388715,-5.05940016621322));
#69478=CARTESIAN_POINT('Ctrl Pts',(23.6579454348691,-0.513398997797603,
-6.03633961784113));
#69479=CARTESIAN_POINT('Ctrl Pts',(23.7585153448269,2.42988395829362,-5.54947190839679));
#69480=CARTESIAN_POINT('Ctrl Pts',(23.8590852547847,4.78392214621243,-3.71686203831083));
#69481=CARTESIAN_POINT('Ctrl Pts',(23.9596551647425,5.9778633318121,-0.982916323515933));
#69482=CARTESIAN_POINT('Ctrl Pts',(24.0602250747003,5.72217780536357,1.98938575360903));
#69483=CARTESIAN_POINT('Ctrl Pts',(24.1607949846581,4.07886908692909,4.47926349800412));
#69484=CARTESIAN_POINT('Ctrl Pts',(24.2613648946159,1.44643812612182,5.88292370001167));
#69485=CARTESIAN_POINT('Ctrl Pts',(24.3619348045737,-1.53675283513459,5.85997996895585));
#69486=CARTESIAN_POINT('Ctrl Pts',(24.4625047145315,-4.14728255675176,4.41599613986702));
#69487=CARTESIAN_POINT('Ctrl Pts',(24.5630746244893,-5.7520998284564,1.90113704827657));
#69488=CARTESIAN_POINT('Ctrl Pts',(24.6636445344472,-5.96203784333286,-1.07474614096765));
#69489=CARTESIAN_POINT('Ctrl Pts',(24.7642144444049,-4.72618681349424,-3.79000431619953));
#69490=CARTESIAN_POINT('Ctrl Pts',(24.8647843543628,-2.34423954982043,-5.58618970729741));
#69491=CARTESIAN_POINT('Ctrl Pts',(24.9653542643205,0.606183786696204,-6.027728903128));
#69492=CARTESIAN_POINT('Ctrl Pts',(25.0659241742783,3.40960807675939,-5.00754902879192));
#69493=CARTESIAN_POINT('Ctrl Pts',(25.1664940842361,5.38620534329685,-2.77304282561564));
#69494=CARTESIAN_POINT('Ctrl Pts',(25.267063994194,6.05665245068485,0.133923875657654));
#69495=CARTESIAN_POINT('Ctrl Pts',(25.3676339041517,5.25836655252189,3.00841415236948));
#69496=CARTESIAN_POINT('Ctrl Pts',(25.4682038141095,3.1849312919251,5.15336658686088));
#69497=CARTESIAN_POINT('Ctrl Pts',(25.5687737240673,0.339152934716677,6.04863206020427));
#69498=CARTESIAN_POINT('Ctrl Pts',(25.6693436340251,-2.58886971720797,5.47710946578407));
#69499=CARTESIAN_POINT('Ctrl Pts',(25.7699135439829,-4.88909369128298,3.57739254076412));
#69500=CARTESIAN_POINT('Ctrl Pts',(25.8704834539407,-6.00371665389393,0.810161004130993));
#69501=CARTESIAN_POINT('Ctrl Pts',(25.9710533638985,-5.66244349610708,-2.15353387859408));
#69502=CARTESIAN_POINT('Ctrl Pts',(26.0716232738563,-3.94803266490803,-4.59499864958382));
#69503=CARTESIAN_POINT('Ctrl Pts',(26.1721931838141,-1.27622731104849,-5.92218020355611));
#69504=CARTESIAN_POINT('Ctrl Pts',(26.272763093772,1.70506206712723,-5.81323815614858));
#69505=CARTESIAN_POINT('Ctrl Pts',(26.3733330037297,4.27287536179091,-4.29459086007714));
#69506=CARTESIAN_POINT('Ctrl Pts',(26.4739029136876,5.80452005943394,-1.73450897734397));
#69507=CARTESIAN_POINT('Ctrl Pts',(26.5744728236454,5.92857363936159,1.24618983928002));
#69508=CARTESIAN_POINT('Ctrl Pts',(26.6750427336032,4.61495321523026,3.92468869263458));
#69509=CARTESIAN_POINT('Ctrl Pts',(26.775612643561,2.18221060908968,5.65145391650984));
#69510=CARTESIAN_POINT('Ctrl Pts',(26.8761825535188,-0.779716191245683,
6.00774643056506));
#69511=CARTESIAN_POINT('Ctrl Pts',(26.9767524634766,-3.55256248640603,4.90716560684868));
#69512=CARTESIAN_POINT('Ctrl Pts',(27.0773223734343,-5.46391543676058,2.61660134770037));
#69513=CARTESIAN_POINT('Ctrl Pts',(27.1778922833921,-6.05027359719579,-0.308486485819792));
#69514=CARTESIAN_POINT('Ctrl Pts',(27.27846219335,-5.16944561856005,-3.15876661208267));
#69515=CARTESIAN_POINT('Ctrl Pts',(27.3790321033077,-3.03503152743054,-5.24304855407239));
#69516=CARTESIAN_POINT('Ctrl Pts',(27.4796020132656,-0.164624903541294,
-6.05589573506611));
#69517=CARTESIAN_POINT('Ctrl Pts',(27.5801719232234,2.74570311774287,-5.40019341339503));
#69518=CARTESIAN_POINT('Ctrl Pts',(27.6807418331811,4.99020049655438,-3.434948837617));
#69519=CARTESIAN_POINT('Ctrl Pts',(27.781311743139,6.02457855065914,-0.636732125619322));
#69520=CARTESIAN_POINT('Ctrl Pts',(27.8818816530968,5.59800149235906,2.31589157872376));
#69521=CARTESIAN_POINT('Ctrl Pts',(27.9824515630546,3.81391389108215,4.7069135688122));
#69522=CARTESIAN_POINT('Ctrl Pts',(28.0830214730124,1.10495545434426,5.95651307030991));
#69523=CARTESIAN_POINT('Ctrl Pts',(28.1835913829702,-1.87195372889476,5.76166327979473));
#69524=CARTESIAN_POINT('Ctrl Pts',(28.284161292928,-4.39491574430826,4.16961510373431));
#69525=CARTESIAN_POINT('Ctrl Pts',(28.3847312028858,-5.85211447499653,1.56643885434258));
#69526=CARTESIAN_POINT('Ctrl Pts',(28.4853011128436,-5.89018048316609,-1.41659746879174));
#69527=CARTESIAN_POINT('Ctrl Pts',(28.5858710228014,-4.49988279460417,-4.05611012519177));
#69528=CARTESIAN_POINT('Ctrl Pts',(28.6864409327592,-2.01836740197889,-5.71201956784875));
#69529=CARTESIAN_POINT('Ctrl Pts',(28.787010842717,0.952600348157724,-5.98276918237263));
#69530=CARTESIAN_POINT('Ctrl Pts',(28.8875807526748,3.69256333389179,-4.80270242031044));
#69531=CARTESIAN_POINT('Ctrl Pts',(28.9881506626326,5.53708288982151,-2.45798445562696));
#69532=CARTESIAN_POINT('Ctrl Pts',(29.0887205725904,6.03886461144926,0.482792623642562));
#69533=CARTESIAN_POINT('Ctrl Pts',(29.1892904825482,5.07622686322841,3.30649290728049));
#69534=CARTESIAN_POINT('Ctrl Pts',(29.289860392506,2.88260847043635,5.32837150722681));
#69535=CARTESIAN_POINT('Ctrl Pts',(29.3904303024638,-0.0100399950044803,
6.05812460348565));
#69536=CARTESIAN_POINT('Ctrl Pts',(29.4910002124216,-2.90025377029946,5.31878769840664));
#69537=CARTESIAN_POINT('Ctrl Pts',(29.5915701223794,-5.08715850291843,3.28964935502898));
#69538=CARTESIAN_POINT('Ctrl Pts',(29.6921400323372,-6.04043167775162,0.462773874881315));
#69539=CARTESIAN_POINT('Ctrl Pts',(29.792709942295,-5.52890537050686,-2.47632387155606));
#69540=CARTESIAN_POINT('Ctrl Pts',(29.8932798522528,-3.67662427035448,-4.81491521083168));
#69541=CARTESIAN_POINT('Ctrl Pts',(29.9938497622106,-0.932764949584756,
-5.98589375629772));
#69542=CARTESIAN_POINT('Ctrl Pts',(30.0944196721684,2.03728906850845,-5.70529821869058));
#69543=CARTESIAN_POINT('Ctrl Pts',(30.1949895821262,4.51330224124522,-4.04117277433529));
#69544=CARTESIAN_POINT('Ctrl Pts',(30.295559492084,5.89484350566002,-1.39706641096112));
#69545=CARTESIAN_POINT('Ctrl Pts',(30.3961294020418,5.84689029440262,1.5858273544363));
#69546=CARTESIAN_POINT('Ctrl Pts',(30.4966993119996,4.38107121992341,4.18415935150857));
#69547=CARTESIAN_POINT('Ctrl Pts',(30.5972692219574,1.85284614596454,5.76783630768438));
#69548=CARTESIAN_POINT('Ctrl Pts',(30.6978391319152,-1.12469252340764,5.95281792436565));
#69549=CARTESIAN_POINT('Ctrl Pts',(30.798409041873,-3.82949422402105,4.69424631874461));
#69550=CARTESIAN_POINT('Ctrl Pts',(30.8989789518308,-5.6056468718478,2.29732402176987));
#69551=CARTESIAN_POINT('Ctrl Pts',(30.9995488617886,-6.02243497875305,-0.656697372881666));
#69552=CARTESIAN_POINT('Ctrl Pts',(31.1001187717465,-4.97878778759543,-3.45147021991332));
#69553=CARTESIAN_POINT('Ctrl Pts',(31.2006886817042,-2.72778884382925,-5.40926450974054));
#69554=CARTESIAN_POINT('Ctrl Pts',(31.301258591662,0.18469654640664,-6.05531681240572));
#69555=CARTESIAN_POINT('Ctrl Pts',(31.4018285016198,3.05239318313103,-5.2329600006529));
#69556=CARTESIAN_POINT('Ctrl Pts',(31.5023984115776,5.17988710053376,-3.14161489342376));
#69557=CARTESIAN_POINT('Ctrl Pts',(31.6029683215354,6.05126285505238,-0.288430878931537));
#69558=CARTESIAN_POINT('Ctrl Pts',(31.7035382314933,5.45521257632139,2.63469737541198));
#69559=CARTESIAN_POINT('Ctrl Pts',(31.804108141451,3.53627794383591,4.91891378424115));
#69560=CARTESIAN_POINT('Ctrl Pts',(31.9046780514089,0.759798954099677,6.0102978347339));
#69561=CARTESIAN_POINT('Ctrl Pts',(32.0052479613666,-2.20093062794899,5.64418983414041));
#69562=CARTESIAN_POINT('Ctrl Pts',(32.1058178713245,-4.62793642734424,3.90937065744835));
#69563=CARTESIAN_POINT('Ctrl Pts',(32.2063877812822,-5.9326716269689,1.22653246162345));
#69564=CARTESIAN_POINT('Ctrl Pts',(32.3069576912401,-5.79873906406749,-1.75373880031083));
#69565=CARTESIAN_POINT('Ctrl Pts',(32.4075276011978,-4.25861726985059,-4.30872991283835));
#69566=CARTESIAN_POINT('Ctrl Pts',(32.5080975111556,-1.68578445363485,-5.81885773058089));
#69567=CARTESIAN_POINT('Ctrl Pts',(32.6086674211135,1.29584964141577,-5.91791755769718));
#69568=CARTESIAN_POINT('Ctrl Pts',(32.7092373310713,3.96324131392763,-4.58188747138504));
#69569=CARTESIAN_POINT('Ctrl Pts',(32.809807241029,5.6695503794838,-2.13475361748213));
#69570=CARTESIAN_POINT('Ctrl Pts',(32.9103771509869,6.00099835852668,0.830056151003031));
#69571=CARTESIAN_POINT('Ctrl Pts',(33.0109470609446,4.87720940145834,3.59357801740607));
#69572=CARTESIAN_POINT('Ctrl Pts',(33.1115169709025,2.57070136297812,5.48566030804317));
#69573=CARTESIAN_POINT('Ctrl Pts',(33.2120868808602,-0.359199543090878,
6.04747469619355));
#69574=CARTESIAN_POINT('Ctrl Pts',(33.3126567908181,-3.20199486916962,5.14278167635662));
#69575=CARTESIAN_POINT('Ctrl Pts',(33.4132267007758,-5.26830919584373,2.99096852705713));
#69576=CARTESIAN_POINT('Ctrl Pts',(33.5137966107337,-6.05706307763735,0.113848084657791));
#69577=CARTESIAN_POINT('Ctrl Pts',(33.6143665206914,-5.37698437719752,-2.79088042026733));
#69578=CARTESIAN_POINT('Ctrl Pts',(33.7149364306493,-3.39299159394969,-5.01882282574756));
#69579=CARTESIAN_POINT('Ctrl Pts',(33.815506340607,-0.586201269953505,-6.02970501633063));
#69580=CARTESIAN_POINT('Ctrl Pts',(33.9160762505649,2.36274235738757,-5.57838893099654));
#69581=CARTESIAN_POINT('Ctrl Pts',(34.0166461605227,4.73872299697853,-3.7743183319329));
#69582=CARTESIAN_POINT('Ctrl Pts',(34.1172160704805,5.96556738903081,-1.05497878641703));
#69583=CARTESIAN_POINT('Ctrl Pts',(34.2177859804382,5.74576682457463,1.92019220664896));
#69584=CARTESIAN_POINT('Ctrl Pts',(34.3183558903961,4.13262275128,4.4297182425591));
#69585=CARTESIAN_POINT('Ctrl Pts',(34.4189258003539,1.51732121828013,5.86504141787719));
#69586=CARTESIAN_POINT('Ctrl Pts',(34.5194957103117,-1.46592940399906,5.8780970981559));
#69587=CARTESIAN_POINT('Ctrl Pts',(34.6200656202695,-4.09369340772253,4.46571929216637));
#69588=CARTESIAN_POINT('Ctrl Pts',(34.7206355302273,-5.72874028404199,1.97040840204573));
#69589=CARTESIAN_POINT('Ctrl Pts',(34.8212054401851,-5.97457257294518,-1.00272482938694));
#69590=CARTESIAN_POINT('Ctrl Pts',(34.9217753501429,-4.77157615599258,-3.73269815286756));
#69591=CARTESIAN_POINT('Ctrl Pts',(35.0223452601007,-2.41147662872138,-5.55749538749143));
#69592=CARTESIAN_POINT('Ctrl Pts',(35.1229151700585,0.533403905146523,-6.03460477470002));
#69593=CARTESIAN_POINT('Ctrl Pts',(35.2234850800163,3.34893445118577,-5.04832769880472));
#69594=CARTESIAN_POINT('Ctrl Pts',(35.3240549899741,5.35235127567129,-2.83783550169453));
#69595=CARTESIAN_POINT('Ctrl Pts',(35.4246248999319,6.05782752326399,0.0608293616863961));
#69596=CARTESIAN_POINT('Ctrl Pts',(35.5251948098897,5.29428581121683,2.94474315722203));
#69597=CARTESIAN_POINT('Ctrl Pts',(35.6257647198475,3.24688434742266,5.11455927205068));
#69598=CARTESIAN_POINT('Ctrl Pts',(35.7263346298053,0.412116224389641,6.04409916616635));
#69599=CARTESIAN_POINT('Ctrl Pts',(35.8269045397631,-2.52258972829639,5.50795021542056));
#69600=CARTESIAN_POINT('Ctrl Pts',(35.9274744497208,-4.84556984338814,3.63612807883681));
#69601=CARTESIAN_POINT('Ctrl Pts',(36.0280443596788,-5.99350344266373,0.882548013218436));
#69602=CARTESIAN_POINT('Ctrl Pts',(36.1286142696365,-5.68801761647303,-2.08504918588275));
#69603=CARTESIAN_POINT('Ctrl Pts',(36.2291841795943,-4.00319241469631,-4.54702375227752));
#69604=CARTESIAN_POINT('Ctrl Pts',(36.3297540895521,-1.34759649841855,-5.90634897295342));
#69605=CARTESIAN_POINT('Ctrl Pts',(36.4303239995099,1.63479040867594,-5.83338965204271));
#69606=CARTESIAN_POINT('Ctrl Pts',(36.5308939094677,4.22074204894102,-4.34583836206078));
#69607=CARTESIAN_POINT('Ctrl Pts',(36.6314638194255,5.78316737567371,-1.80442501030139));
#69608=CARTESIAN_POINT('Ctrl Pts',(36.7320337293833,5.94317959212186,1.17455985315532));
#69609=CARTESIAN_POINT('Ctrl Pts',(36.8326036393411,4.66197587353986,3.86871496331666));
#69610=CARTESIAN_POINT('Ctrl Pts',(36.9331735492989,2.25024701878697,5.62471002517447));
#69611=CARTESIAN_POINT('Ctrl Pts',(37.0337434592567,-0.707164800944547,
6.01671774783917));
#69612=CARTESIAN_POINT('Ctrl Pts',(37.1343133692145,-3.49308976519476,4.94967659601609));
#69613=CARTESIAN_POINT('Ctrl Pts',(37.2348832791723,-5.43194346833712,2.68234313048267));
#69614=CARTESIAN_POINT('Ctrl Pts',(37.3354531891302,-6.05355555638045,-0.235456235154939));
#69615=CARTESIAN_POINT('Ctrl Pts',(37.4360230990879,-5.20718563307572,-3.09615766645496));
#69616=CARTESIAN_POINT('Ctrl Pts',(37.5365930090458,-3.09807767624484,-5.20604352890092));
#69617=CARTESIAN_POINT('Ctrl Pts',(37.6371629190035,-0.237688549838743,
-6.05346831709999));
#69618=CARTESIAN_POINT('Ctrl Pts',(37.7377328289614,2.68033984529413,-5.43293224940147));
#69619=CARTESIAN_POINT('Ctrl Pts',(37.8383027389191,4.94838813525662,-3.49491478804698));
#69620=CARTESIAN_POINT('Ctrl Pts',(37.9388726488769,6.01645656213379,-0.709383499113968));
#69621=CARTESIAN_POINT('Ctrl Pts',(38.0394425588348,5.62553945183186,2.24817267769651));
#69622=CARTESIAN_POINT('Ctrl Pts',(38.1400124687925,3.87043386708642,4.66054891545712));
#69623=CARTESIAN_POINT('Ctrl Pts',(38.2405823787503,1.17675140135296,5.94274605315352));
#69624=CARTESIAN_POINT('Ctrl Pts',(38.3411522887081,-1.80229226622721,5.78383238864642));
#69625=CARTESIAN_POINT('Ctrl Pts',(38.441722198666,-4.34428161071217,4.22234434878138));
#69626=CARTESIAN_POINT('Ctrl Pts',(38.5422921086237,-5.83278640428161,1.63694143905193));
#69627=CARTESIAN_POINT('Ctrl Pts',(38.6428620185816,-5.90684551584258,-1.34541836052145));
#69628=CARTESIAN_POINT('Ctrl Pts',(38.7434319285394,-4.54849967459375,-4.00151536584311));
#69629=CARTESIAN_POINT('Ctrl Pts',(38.8440018384971,-2.08714657773488,-5.68724833956698));
#69630=CARTESIAN_POINT('Ctrl Pts',(38.944571748455,0.880337767549051,-5.99382848669234));
#69631=CARTESIAN_POINT('Ctrl Pts',(39.0451416584127,3.63434096202235,-4.84691038545427));
#69632=CARTESIAN_POINT('Ctrl Pts',(39.1457115683706,5.50701960175014,-2.52462068810298));
#69633=CARTESIAN_POINT('Ctrl Pts',(39.2462814783283,6.04425072865394,0.409887352847377));
#69634=CARTESIAN_POINT('Ctrl Pts',(39.3468513882862,5.11575625692352,3.24499806357505));
#69635=CARTESIAN_POINT('Ctrl Pts',(39.4474212982439,2.94669529667884,5.29319953727315));
#69636=CARTESIAN_POINT('Ctrl Pts',(39.5479912082018,0.0630632635893668,
6.05780467972048));
#69637=CARTESIAN_POINT('Ctrl Pts',(39.6485611181596,-2.83586155663387,5.35339740206759));
#69638=CARTESIAN_POINT('Ctrl Pts',(39.7491310281174,-5.04709239056434,3.35079586277132));
#69639=CARTESIAN_POINT('Ctrl Pts',(39.8497009380752,-6.03440766446482,0.535629211214205));
#69640=CARTESIAN_POINT('Ctrl Pts',(39.950270848033,-5.55838427432381,-2.40942706297736));
#69641=CARTESIAN_POINT('Ctrl Pts',(40.0508407579908,-3.73445748247584,-4.77019934850087));
#69642=CARTESIAN_POINT('Ctrl Pts',(40.1514106679486,-1.00492796585556,-5.97420239833732));
#69643=CARTESIAN_POINT('Ctrl Pts',(40.2519805779064,1.96829571741389,-5.7294665093417));
#69644=CARTESIAN_POINT('Ctrl Pts',(40.3525504878642,4.46420938357584,-4.09533992391978));
#69645=CARTESIAN_POINT('Ctrl Pts',(40.453120397822,5.8775561171401,-1.46809693233341));
#69646=CARTESIAN_POINT('Ctrl Pts',(40.5536903077798,5.86560055186679,1.51515830156386));
#69647=CARTESIAN_POINT('Ctrl Pts',(40.6542602177375,4.43124190204296,4.13098895162365));
#69648=CARTESIAN_POINT('Ctrl Pts',(40.7548301276954,1.92231090551379,5.74505833698848));
#69649=CARTESIAN_POINT('Ctrl Pts',(40.8554000376532,-1.05277883082213,5.96595602114453));
#69650=CARTESIAN_POINT('Ctrl Pts',(40.955969947611,-3.77257060694586,4.74011450583907));
#69651=CARTESIAN_POINT('Ctrl Pts',(41.0565398575688,-5.57751725842217,2.36479930329417));
#69652=CARTESIAN_POINT('Ctrl Pts',(41.1571097675266,-6.02992077601796,-0.583977694612491));
#69653=CARTESIAN_POINT('Ctrl Pts',(41.2576796774844,-5.02007369615812,-3.39114060428041));
#69654=CARTESIAN_POINT('Ctrl Pts',(41.3582495874422,-2.79286306640333,-5.37595483660142));
#69655=CARTESIAN_POINT('Ctrl Pts',(41.4588194974,0.111614452777684,-6.05710464882267));
#69656=CARTESIAN_POINT('Ctrl Pts',(41.5593894073578,2.98902556324098,-5.26941179783377));
#69657=CARTESIAN_POINT('Ctrl Pts',(41.6599593173156,5.14160054765725,-3.20389112193102));
#69658=CARTESIAN_POINT('Ctrl Pts',(41.7605292272734,6.04734182530387,-0.361429606961375));
#69659=CARTESIAN_POINT('Ctrl Pts',(41.8610991372312,5.4866079160396,2.56867827656746));
#69660=CARTESIAN_POINT('Ctrl Pts',(41.961669047189,3.59537631016514,4.87588388922062));
#69661=CARTESIAN_POINT('Ctrl Pts',(42.0622389571468,0.832269044078688,6.00069185603845));
#69662=CARTESIAN_POINT('Ctrl Pts',(42.1628088671046,-2.13266274875579,5.67033721333462));
#69663=CARTESIAN_POINT('Ctrl Pts',(42.2633787770624,-4.58042566087425,3.964930677586));
#69664=CARTESIAN_POINT('Ctrl Pts',(42.3639486870202,-5.91743929319244,1.29803186564886));
#69665=CARTESIAN_POINT('Ctrl Pts',(42.464518596978,-5.81947899081297,-1.68363855632504));
#69666=CARTESIAN_POINT('Ctrl Pts',(42.5650885069358,-4.31030004273577,-4.25702807771454));
#69667=CARTESIAN_POINT('Ctrl Pts',(42.6656584168936,-1.75587704472498,-5.79809195483013));
#69668=CARTESIAN_POINT('Ctrl Pts',(42.7662283268514,1.22434462512233,-5.9331235240632));
#69669=CARTESIAN_POINT('Ctrl Pts',(42.8667982368092,3.90766377732837,-4.62937774611378));
#69670=CARTESIAN_POINT('Ctrl Pts',(42.967368146767,5.64337782736131,-2.20301184983298));
#69671=CARTESIAN_POINT('Ctrl Pts',(43.0679380567248,6.01057761224065,0.757582523616525));
#69672=CARTESIAN_POINT('Ctrl Pts',(43.1685079666826,4.92021750022926,3.53446378723784));
#69673=CARTESIAN_POINT('Ctrl Pts',(43.2690778766404,2.63670887987654,5.45424062502182));
#69674=CARTESIAN_POINT('Ctrl Pts',(43.3696477865982,-0.286199374091665,
6.05136880640467));
#69675=CARTESIAN_POINT('Ctrl Pts',(43.470217696556,-3.1397045262112,5.18104526142618));
#69676=CARTESIAN_POINT('Ctrl Pts',(43.5707876065138,-5.23183403347219,3.05432270054425));
#69677=CARTESIAN_POINT('Ctrl Pts',(43.6713575164717,-6.05524829132899,0.186929514028943));
#69678=CARTESIAN_POINT('Ctrl Pts',(43.7719274264294,-5.41027005106995,-2.72579391872415));
#69679=CARTESIAN_POINT('Ctrl Pts',(43.8724973363873,-3.45330598074203,-4.97751467262823));
#69680=CARTESIAN_POINT('Ctrl Pts',(43.973067246345,-0.658918182789008,-6.0221924032073));
#69681=CARTESIAN_POINT('Ctrl Pts',(44.0736371563029,2.29525670727468,-5.60649366008458));
#69682=CARTESIAN_POINT('Ctrl Pts',(44.1742070662606,4.69283382164707,-3.83122503062184));
#69683=CARTESIAN_POINT('Ctrl Pts',(44.2747769762185,5.95240277399595,-1.1268876292617));
#69684=CARTESIAN_POINT('Ctrl Pts',(44.3753468861762,5.76851917764986,1.85071905213722));
#69685=CARTESIAN_POINT('Ctrl Pts',(44.4759167961341,4.18577464643037,4.37952795654495));
#69686=CARTESIAN_POINT('Ctrl Pts',(44.5764867060918,1.58798336668632,5.84630510151374));
#69687=CARTESIAN_POINT('Ctrl Pts',(44.6770566160497,-1.39489251249749,5.89535829203248));
#69688=CARTESIAN_POINT('Ctrl Pts',(44.7776265260074,-4.03950815816409,4.5147921716269));
#69689=CARTESIAN_POINT('Ctrl Pts',(44.8781964359653,-5.70454655280041,2.03939283606441));
#69690=CARTESIAN_POINT('Ctrl Pts',(44.978766345923,-5.98623731901994,-0.9305575066759));
#69691=CARTESIAN_POINT('Ctrl Pts',(45.0793362558809,-4.81627068850187,-3.67484845509796));
#69692=CARTESIAN_POINT('Ctrl Pts',(45.1799061658386,-2.47836256200596,-5.52799181657365));
#69693=CARTESIAN_POINT('Ctrl Pts',(45.2804760757965,0.460546352330777,-6.04060192118407));
#69694=CARTESIAN_POINT('Ctrl Pts',(45.3810459857542,3.28777317267875,-5.08837125983076));
#69695=CARTESIAN_POINT('Ctrl Pts',(45.481615895712,5.3177178288616,-2.90221494818445));
#69696=CARTESIAN_POINT('Ctrl Pts',(45.5821858056699,6.05812048918958,-0.0122740099132358));
#69697=CARTESIAN_POINT('Ctrl Pts',(45.6827557156276,5.32943414589292,2.88064336519618));
#69698=CARTESIAN_POINT('Ctrl Pts',(45.7833256255855,3.30836460994689,5.07500720398591));
#69699=CARTESIAN_POINT('Ctrl Pts',(45.8838955355433,0.485019504023933,6.03868616452074));
#69700=CARTESIAN_POINT('Ctrl Pts',(45.984465445501,-2.45594241410608,5.53798892843354));
#69701=CARTESIAN_POINT('Ctrl Pts',(46.0850353554589,-4.80134041096105,3.69433414446097));
#69702=CARTESIAN_POINT('Ctrl Pts',(46.1856052654166,-5.98241749128956,0.954806510645358));
#69703=CARTESIAN_POINT('Ctrl Pts',(46.2861751753745,-5.71276347981686,-2.01626088007693));
#69704=CARTESIAN_POINT('Ctrl Pts',(46.3867450853323,-4.05776924219922,-4.49838674303575));
#69705=CARTESIAN_POINT('Ctrl Pts',(46.4873149952901,-1.41876945639242,-5.88965769314871));
#69706=CARTESIAN_POINT('Ctrl Pts',(46.5878849052479,1.56428070127213,-5.85269172265938));
#69707=CARTESIAN_POINT('Ctrl Pts',(46.6884548152057,4.16799413545586,-4.39645304758999));
#69708=CARTESIAN_POINT('Ctrl Pts',(46.7890247251635,5.76097257972044,-1.87407829307293));
#69709=CARTESIAN_POINT('Ctrl Pts',(46.8895946351213,5.95692013261322,1.102758834254));
#69710=CARTESIAN_POINT('Ctrl Pts',(46.9901645450792,4.70831968123497,3.81217789356075));
#69711=CARTESIAN_POINT('Ctrl Pts',(47.0907344550368,2.31795576021386,5.59714709531108));
#69712=CARTESIAN_POINT('Ctrl Pts',(47.1913043649948,-0.634510437296323,
6.02481294463323));
#69713=CARTESIAN_POINT('Ctrl Pts',(47.2918742749524,-3.43310839996693,4.99146684121354));
#69714=CARTESIAN_POINT('Ctrl Pts',(47.3924441849103,-5.39918053096372,2.74769432559742));
#69715=CARTESIAN_POINT('Ctrl Pts',(47.493014094868,-6.05595603097126,-0.16239169868203));
#69716=CARTESIAN_POINT('Ctrl Pts',(47.593584004826,-5.24416740660887,-3.03309787582251));
#69717=CARTESIAN_POINT('Ctrl Pts',(47.6941539147836,-3.16067270047356,-5.16828042905366));
#69718=CARTESIAN_POINT('Ctrl Pts',(47.7947238247416,-0.310717585271087,
-6.05015942724333));
#69719=CARTESIAN_POINT('Ctrl Pts',(47.8952937346992,2.61458627688499,-5.4648799724772));
#69720=CARTESIAN_POINT('Ctrl Pts',(47.9958636446571,4.90585521760734,-3.55437182871079));
#69721=CARTESIAN_POINT('Ctrl Pts',(48.0964335546149,6.00745849116074,-0.781931576187193));
#69722=CARTESIAN_POINT('Ctrl Pts',(48.1970034645728,5.65225825200023,2.18012641045266));
#69723=CARTESIAN_POINT('Ctrl Pts',(48.2975733745305,3.92639025235566,4.61350561927309));
#69724=CARTESIAN_POINT('Ctrl Pts',(48.3981432844883,1.24837599646418,5.92811368685774));
#69725=CARTESIAN_POINT('Ctrl Pts',(48.4987131944461,-1.73236836393201,5.80515928846964));
#69726=CARTESIAN_POINT('Ctrl Pts',(48.599283104404,-4.29301488734706,4.27445875987527));
#69727=CARTESIAN_POINT('Ctrl Pts',(48.6998530143617,-5.81260899613078,1.70720566158783));
#69728=CARTESIAN_POINT('Ctrl Pts',(48.8004229243196,-5.92265042701329,-1.27404334002308));
#69729=CARTESIAN_POINT('Ctrl Pts',(48.9009928342773,-4.59645422773243,-3.94633792841142));
#69730=CARTESIAN_POINT('Ctrl Pts',(49.0015627442352,-2.15562183498608,-5.66164896628087));
#69731=CARTESIAN_POINT('Ctrl Pts',(49.1021326541929,0.807946997123318,-6.00401500353698));
#69732=CARTESIAN_POINT('Ctrl Pts',(49.2027025641508,3.57558937793424,-4.89041257086371));
#69733=CARTESIAN_POINT('Ctrl Pts',(49.3032724741085,5.47615441256601,-2.59088929956335));
#69734=CARTESIAN_POINT('Ctrl Pts',(49.4038423840664,6.04875671618125,0.336922396569298));
#69735=CARTESIAN_POINT('Ctrl Pts',(49.5044122940241,5.15454072306582,3.18303070156636));
#69736=CARTESIAN_POINT('Ctrl Pts',(49.6049822039819,3.0103530417834,5.25725680147769));
#69737=CARTESIAN_POINT('Ctrl Pts',(49.7055521139397,0.136157339266722,6.05660265262809));
#69738=CARTESIAN_POINT('Ctrl Pts',(49.8061220238975,-2.77105640081398,5.38722757421346));
#69739=CARTESIAN_POINT('Ctrl Pts',(49.9066919338553,-5.00629134910212,3.41145444653204));
#69740=CARTESIAN_POINT('Ctrl Pts',(50.0072618438131,-6.02750495479215,0.608406552244426));
#69741=CARTESIAN_POINT('Ctrl Pts',(50.1078317537709,-5.58705379759421,-2.34217940722865));
#69742=CARTESIAN_POINT('Ctrl Pts',(50.2084016637287,-3.79174690397582,-4.72478887666399));
#69743=CARTESIAN_POINT('Ctrl Pts',(50.3089715736866,-1.07694465018776,-5.96164111074206));
#69744=CARTESIAN_POINT('Ctrl Pts',(50.4095414836443,1.89901575420593,-5.75280050741684));
#69745=CARTESIAN_POINT('Ctrl Pts',(50.5101113936022,4.41446647293192,-4.14891073321875));
#69746=CARTESIAN_POINT('Ctrl Pts',(50.6106813035599,5.85941287207133,-1.53891367771645));
#69747=CARTESIAN_POINT('Ctrl Pts',(50.7112512135178,5.88345669368406,1.44426861989114));
#69748=CARTESIAN_POINT('Ctrl Pts',(50.8118211234755,4.4807673317266,4.07721702044296));
#69749=CARTESIAN_POINT('Ctrl Pts',(50.9123910334334,1.99149574899846,5.72144380332262));
#69750=CARTESIAN_POINT('Ctrl Pts',(51.0129609433911,-0.980711838525075,
5.97822538907948));
#69751=CARTESIAN_POINT('Ctrl Pts',(51.113530853349,-3.71509764943117,4.78529246421249));
#69752=CARTESIAN_POINT('Ctrl Pts',(51.2141007633067,-5.54857547841287,2.43193023609094));
#69753=CARTESIAN_POINT('Ctrl Pts',(51.3146706732646,-6.03652853025234,-0.511172980807434));
#69754=CARTESIAN_POINT('Ctrl Pts',(51.4152405832223,-5.06062860992243,-3.33031718989236));
#69755=CARTESIAN_POINT('Ctrl Pts',(51.5158104931802,-2.85753060802056,-5.34186234726087));
#69756=CARTESIAN_POINT('Ctrl Pts',(51.6163804031379,0.0385161064819134,
-6.05801048384692));
#69757=CARTESIAN_POINT('Ctrl Pts',(51.7169503130958,2.9252226983183,-5.30509629300932));
#69758=CARTESIAN_POINT('Ctrl Pts',(51.8175202230535,5.10256530392816,-3.26570081789599));
#69759=CARTESIAN_POINT('Ctrl Pts',(51.9180901330113,6.04254021576997,-0.43437570565172));
#69760=CARTESIAN_POINT('Ctrl Pts',(52.0186600429692,5.51720432687948,2.50228514129));
#69761=CARTESIAN_POINT('Ctrl Pts',(52.119229952927,3.65395113808825,4.8321439955077));
#69762=CARTESIAN_POINT('Ctrl Pts',(52.2197998628847,0.90461794373694,5.99021209046278));
#69763=CARTESIAN_POINT('Ctrl Pts',(52.3203697728426,-2.06408432325012,5.69565891002731));
#69764=CARTESIAN_POINT('Ctrl Pts',(52.4209396828003,-4.53224791867086,4.01991334689623));
#69765=CARTESIAN_POINT('Ctrl Pts',(52.5215095927582,-5.90134529530529,1.36934225760051));
#69766=CARTESIAN_POINT('Ctrl Pts',(52.6220795027159,-5.83937151787078,-1.61329315039637));
#69767=CARTESIAN_POINT('Ctrl Pts',(52.7226494126738,-4.36135517406001,-4.20470635818695));
#69768=CARTESIAN_POINT('Ctrl Pts',(52.8232193226315,-1.82571395490191,-5.77648189365705));
#69769=CARTESIAN_POINT('Ctrl Pts',(52.9237892325894,1.15266132665882,-5.94746554246089));
#69770=CARTESIAN_POINT('Ctrl Pts',(53.0243591425472,3.85151722881557,-4.67619391699774));
#69771=CARTESIAN_POINT('Ctrl Pts',(53.124929052505,5.61638351835037,-2.27094929200402));
#69772=CARTESIAN_POINT('Ctrl Pts',(53.2254989624628,6.01928163968487,0.68499858128424));
#69773=CARTESIAN_POINT('Ctrl Pts',(53.3260688724206,4.96250914446559,3.47483488850872));
#69774=CARTESIAN_POINT('Ctrl Pts',(53.4266387823784,2.70233245456293,5.42202672605472));
#69775=CARTESIAN_POINT('Ctrl Pts',(53.5272086923362,-0.213157531242237,
6.05438175085432));
#69776=CARTESIAN_POINT('Ctrl Pts',(53.627778602294,-3.07695699546339,5.21855441112398));
#69777=CARTESIAN_POINT('Ctrl Pts',(53.7283485122518,-5.19459704435567,3.11723212236909));
#69778=CARTESIAN_POINT('Ctrl Pts',(53.8289184222096,-6.05255176728989,0.259983720705316));
#69779=CARTESIAN_POINT('Ctrl Pts',(53.9294883321674,-5.44276792496704,-2.6603104964399));
#69780=CARTESIAN_POINT('Ctrl Pts',(54.0300582421252,-3.51311749114105,-4.93548173368623));
#69781=CARTESIAN_POINT('Ctrl Pts',(54.1306281520831,-0.731539197512978,
-6.01380284938146));
#69782=CARTESIAN_POINT('Ctrl Pts',(54.2311980620408,2.22743693235633,-5.63378204828362));
#69783=CARTESIAN_POINT('Ctrl Pts',(54.3317679719986,4.64626111150299,-3.88757375973938));
#69784=CARTESIAN_POINT('Ctrl Pts',(54.4323378819564,5.93837177711084,-1.19863255369758));
#69785=CARTESIAN_POINT('Ctrl Pts',(54.5329077919142,5.79043082073166,1.78097674413478));
#69786=CARTESIAN_POINT('Ctrl Pts',(54.633477701872,4.23831846276371,4.32869928740943));
#69787=CARTESIAN_POINT('Ctrl Pts',(54.7340476118298,1.65841148346058,5.82671877265184));
#69788=CARTESIAN_POINT('Ctrl Pts',(54.8346175217877,-1.32364702837341,5.91175850596819));
#69789=CARTESIAN_POINT('Ctrl Pts',(54.9351874317454,-3.98474541470989,4.56321258577206));
#69790=CARTESIAN_POINT('Ctrl Pts',(55.0357573417033,-5.67950118530435,2.10807061113231));
#69791=CARTESIAN_POINT('Ctrl Pts',(55.136327251661,-5.99707144006536,-0.858235698386034));
#69792=CARTESIAN_POINT('Ctrl Pts',(55.2368971616188,-4.86018337906989,-3.61650093368403));
#69793=CARTESIAN_POINT('Ctrl Pts',(55.3374670715766,-2.54504712920928,-5.4976088187116));
#69794=CARTESIAN_POINT('Ctrl Pts',(55.4380369815344,0.387954839329869,-6.04588140635559));
#69795=CARTESIAN_POINT('Ctrl Pts',(55.505083588173,2.27948268610681,-5.43340712928736));
#69796=CARTESIAN_POINT('Ctrl Pts',(55.5386068914922,3.09548085772058,-4.92001278896564));
#69797=CARTESIAN_POINT('Ctrl Pts',(18.8656682926829,3.45292578700087,-4.38059386100382));
#69798=CARTESIAN_POINT('Ctrl Pts',(18.8991915960022,4.17945978894053,-3.8079162583704));
#69799=CARTESIAN_POINT('Ctrl Pts',(18.9662382026407,5.34139059168272,-2.29470092783305));
#69800=CARTESIAN_POINT('Ctrl Pts',(19.0668081125985,5.78874853530519,0.533337577335307));
#69801=CARTESIAN_POINT('Ctrl Pts',(19.1673780225563,4.83241525876795,3.23130860481921));
#69802=CARTESIAN_POINT('Ctrl Pts',(19.2679479325141,2.70419169563657,5.14605048923388));
#69803=CARTESIAN_POINT('Ctrl Pts',(19.3685178424719,-0.0797792217301073,
5.81269672472357));
#69804=CARTESIAN_POINT('Ctrl Pts',(19.4690877524298,-2.84441229285594,5.06986231595082));
#69805=CARTESIAN_POINT('Ctrl Pts',(19.5696576623875,-4.91927346795933,3.09754298939177));
#69806=CARTESIAN_POINT('Ctrl Pts',(19.6702275723453,-5.80121729124116,0.374096513770974));
#69807=CARTESIAN_POINT('Ctrl Pts',(19.7707974823032,-5.27636977596458,-2.44008049241649));
#69808=CARTESIAN_POINT('Ctrl Pts',(19.8713673922609,-3.4720077142605,-4.66253371853033));
#69809=CARTESIAN_POINT('Ctrl Pts',(19.9719373022187,-0.825686473140719,
-5.75432978220954));
#69810=CARTESIAN_POINT('Ctrl Pts',(20.0725072121766,2.02086287490732,-5.45070416604466));
#69811=CARTESIAN_POINT('Ctrl Pts',(20.1730771221344,4.37735479309912,-3.82528833061492));
#69812=CARTESIAN_POINT('Ctrl Pts',(20.2736470320921,5.67234190241483,-1.27224293413637));
#69813=CARTESIAN_POINT('Ctrl Pts',(20.37421694205,5.59179100359806,1.58932005701102));
#69814=CARTESIAN_POINT('Ctrl Pts',(20.4747868520077,4.15523558961498,4.06547441574607));
#69815=CARTESIAN_POINT('Ctrl Pts',(20.5753567619656,1.71103912739439,5.55575467045122));
#69816=CARTESIAN_POINT('Ctrl Pts',(20.6759266719234,-1.14808285301524,5.69876922970695));
#69817=CARTESIAN_POINT('Ctrl Pts',(20.7764965818812,-3.72879572848776,4.45983714130576));
#69818=CARTESIAN_POINT('Ctrl Pts',(20.877066491839,-5.40527885036333,2.13939839301869));
#69819=CARTESIAN_POINT('Ctrl Pts',(20.9776364017968,-5.77098650368354,-0.699842627867562));
#69820=CARTESIAN_POINT('Ctrl Pts',(21.0782063117546,-4.7372348978758,-3.36937241192321));
#69821=CARTESIAN_POINT('Ctrl Pts',(21.1787762217124,-2.5547079071865,-5.22183228757078));
#69822=CARTESIAN_POINT('Ctrl Pts',(21.2793461316702,0.247333551781491,-5.80800232805862));
#69823=CARTESIAN_POINT('Ctrl Pts',(21.379916041628,2.98939683737892,-4.98573680395642));
#69824=CARTESIAN_POINT('Ctrl Pts',(21.4804859515858,5.0065339632579,-2.95443439662243));
#69825=CARTESIAN_POINT('Ctrl Pts',(21.5810558615436,5.80959091282129,-0.206684191439672));
#69826=CARTESIAN_POINT('Ctrl Pts',(21.6816257715014,5.20382706708468,2.59118675228346));
#69827=CARTESIAN_POINT('Ctrl Pts',(21.7821956814592,3.33613963718532,4.76069713912736));
#69828=CARTESIAN_POINT('Ctrl Pts',(21.882765591417,0.659441217112314,5.77574256788688));
#69829=CARTESIAN_POINT('Ctrl Pts',(21.9833355013748,-2.17717113044407,5.39017539585389));
#69830=CARTESIAN_POINT('Ctrl Pts',(22.0839054113326,-4.48582135303932,3.69749533034633));
#69831=CARTESIAN_POINT('Ctrl Pts',(22.1844753212904,-5.70666375904613,1.10817583013857));
#69832=CARTESIAN_POINT('Ctrl Pts',(22.2850452312482,-5.5436451159441,-1.74987535492763));
#69833=CARTESIAN_POINT('Ctrl Pts',(22.385615141206,-4.03629730435431,-4.18358327276709));
#69834=CARTESIAN_POINT('Ctrl Pts',(22.4861850511638,-1.5501508710191,-5.60277584830882));
#69835=CARTESIAN_POINT('Ctrl Pts',(22.5867549611216,1.31190581412394,-5.66330010366589));
#69836=CARTESIAN_POINT('Ctrl Pts',(22.6873248710794,3.85582646866807,-4.35047895901507));
#69837=CARTESIAN_POINT('Ctrl Pts',(22.7878947810372,5.46471252376619,-1.98267041182017));
#69838=CARTESIAN_POINT('Ctrl Pts',(22.888464690995,5.74841049603226,0.865934003501583));
#69839=CARTESIAN_POINT('Ctrl Pts',(22.9890346009528,4.63812387140712,3.50455016839501));
#69840=CARTESIAN_POINT('Ctrl Pts',(23.0896045109106,2.40309620059581,5.29331593426996));
#69841=CARTESIAN_POINT('Ctrl Pts',(23.1901744208684,-0.414680230205875,
5.79845714272258));
#69842=CARTESIAN_POINT('Ctrl Pts',(23.2907443308262,-3.13189706215126,4.89747748554319));
#69843=CARTESIAN_POINT('Ctrl Pts',(23.391314240784,-5.08963155255177,2.80886375400866));
#69844=CARTESIAN_POINT('Ctrl Pts',(23.4918841507418,-5.81313477275929,0.0391029800775002));
#69845=CARTESIAN_POINT('Ctrl Pts',(23.5924540606996,-5.12695781468582,-2.74014023286149));
#69846=CARTESIAN_POINT('Ctrl Pts',(23.6930239706574,-3.19749799998333,-4.85490179812288));
#69847=CARTESIAN_POINT('Ctrl Pts',(23.7935938806152,-0.492647672782865,
-5.79235385657815));
#69848=CARTESIAN_POINT('Ctrl Pts',(23.894163790573,2.33166929098219,-5.32516509103753));
#69849=CARTESIAN_POINT('Ctrl Pts',(23.9947337005308,4.59055845885185,-3.56662837497514));
#69850=CARTESIAN_POINT('Ctrl Pts',(24.0953036104886,5.73624115213431,-0.94318734823729));
#69851=CARTESIAN_POINT('Ctrl Pts',(24.1958735204464,5.49089030394512,1.90897579852541));
#69852=CARTESIAN_POINT('Ctrl Pts',(24.2964434304042,3.91400328376506,4.2982139574468));
#69853=CARTESIAN_POINT('Ctrl Pts',(24.397013340362,1.38797383655825,5.64513893171319));
#69854=CARTESIAN_POINT('Ctrl Pts',(24.4975832503198,-1.47463807120625,5.62312257453662));
#69855=CARTESIAN_POINT('Ctrl Pts',(24.5981531602776,-3.97965151611398,4.23750383358008));
#69856=CARTESIAN_POINT('Ctrl Pts',(24.6987230702354,-5.51960289416221,1.82429406074521));
#69857=CARTESIAN_POINT('Ctrl Pts',(24.7992929801933,-5.7210553218086,-1.03130545141574));
#69858=CARTESIAN_POINT('Ctrl Pts',(24.899862890151,-4.53515675876486,-3.63681427938567));
#69859=CARTESIAN_POINT('Ctrl Pts',(25.0004328001089,-2.24948658571366,-5.36039877527861));
#69860=CARTESIAN_POINT('Ctrl Pts',(25.1010027100666,0.581682147950543,-5.78409118255149));
#69861=CARTESIAN_POINT('Ctrl Pts',(25.2015726200244,3.27179346146541,-4.80514645716718));
#69862=CARTESIAN_POINT('Ctrl Pts',(25.3021425299822,5.16849767702856,-2.66095785232772));
#69863=CARTESIAN_POINT('Ctrl Pts',(25.40271243994,5.81184565510331,0.128510741072388));
#69864=CARTESIAN_POINT('Ctrl Pts',(25.5032823498978,5.04582606481892,2.88681559038817));
#69865=CARTESIAN_POINT('Ctrl Pts',(25.6038522598556,3.05619799740772,4.94507014408847));
#69866=CARTESIAN_POINT('Ctrl Pts',(25.7044221698135,0.325444546488037,5.80414944470552));
#69867=CARTESIAN_POINT('Ctrl Pts',(25.8049920797712,-2.484228926803,5.25572750135977));
#69868=CARTESIAN_POINT('Ctrl Pts',(25.9055619897291,-4.69147902383981,3.43279616321523));
#69869=CARTESIAN_POINT('Ctrl Pts',(26.0061318996869,-5.76104949615515,0.777414710540404));
#69870=CARTESIAN_POINT('Ctrl Pts',(26.1067018096446,-5.4335704249295,-2.0664891402196));
#69871=CARTESIAN_POINT('Ctrl Pts',(26.2072717196025,-3.78845520303171,-4.40927115336947));
#69872=CARTESIAN_POINT('Ctrl Pts',(26.3078416295602,-1.22464285560959,-5.68280870745432));
#69873=CARTESIAN_POINT('Ctrl Pts',(26.408411539518,1.63614433009017,-5.57827004190617));
#69874=CARTESIAN_POINT('Ctrl Pts',(26.5089814494759,4.100167924183,-4.12100569313063));
#69875=CARTESIAN_POINT('Ctrl Pts',(26.6095513594336,5.56990432620359,-1.66440101125078));
#69876=CARTESIAN_POINT('Ctrl Pts',(26.7101212693915,5.6889437238532,1.19581948309323));
#69877=CARTESIAN_POINT('Ctrl Pts',(26.8106911793493,4.42841916567433,3.76605478218288));
#69878=CARTESIAN_POINT('Ctrl Pts',(26.911261089307,2.09400677192963,5.42302503852111));
#69879=CARTESIAN_POINT('Ctrl Pts',(27.0118309992649,-0.748200461426902,
5.76491639131348));
#69880=CARTESIAN_POINT('Ctrl Pts',(27.1124009092227,-3.40896972695984,4.70882048181766));
#69881=CARTESIAN_POINT('Ctrl Pts',(27.2129708191805,-5.24306676824391,2.51083965896878));
#69882=CARTESIAN_POINT('Ctrl Pts',(27.3135407291383,-5.80572463161107,-0.29601761977724));
#69883=CARTESIAN_POINT('Ctrl Pts',(27.4141106390961,-4.96049926954682,-3.03109088054774));
#69884=CARTESIAN_POINT('Ctrl Pts',(27.5146805490538,-2.91235710475748,-5.03112721203537));
#69885=CARTESIAN_POINT('Ctrl Pts',(27.6152504590117,-0.157970849104978,
-5.81111952554301));
#69886=CARTESIAN_POINT('Ctrl Pts',(27.7158203689695,2.63472320146966,-5.18192035648482));
#69887=CARTESIAN_POINT('Ctrl Pts',(27.8163902789273,4.78849914373318,-3.2961099617247));
#69888=CARTESIAN_POINT('Ctrl Pts',(27.9169601888851,5.7810681657188,-0.610995738632328));
#69889=CARTESIAN_POINT('Ctrl Pts',(28.0175300988429,5.37173313402688,2.22228442511572));
#69890=CARTESIAN_POINT('Ctrl Pts',(28.1181000088007,3.65975744147539,4.51666252877937));
#69891=CARTESIAN_POINT('Ctrl Pts',(28.2186699187585,1.06029371979028,5.71575385728667));
#69892=CARTESIAN_POINT('Ctrl Pts',(28.3192398287163,-1.79629031621274,5.52877979568679));
#69893=CARTESIAN_POINT('Ctrl Pts',(28.4198097386741,-4.21727549683238,4.00108139296507));
#69894=CARTESIAN_POINT('Ctrl Pts',(28.5203796486319,-5.61557499982187,1.50312419669493));
#69895=CARTESIAN_POINT('Ctrl Pts',(28.6209495585897,-5.65210239940256,-1.35933932334132));
#69896=CARTESIAN_POINT('Ctrl Pts',(28.7215194685475,-4.31799983261996,-3.89216422762556));
#69897=CARTESIAN_POINT('Ctrl Pts',(28.8220893785053,-1.93678602348512,-5.48114265719722));
#69898=CARTESIAN_POINT('Ctrl Pts',(28.9226592884631,0.91409672910392,-5.74094871072331));
#69899=CARTESIAN_POINT('Ctrl Pts',(29.0232291984209,3.54331181176593,-4.60857964387231));
#69900=CARTESIAN_POINT('Ctrl Pts',(29.1237991083787,5.31327683025914,-2.35863398057979));
#69901=CARTESIAN_POINT('Ctrl Pts',(29.2243690183365,5.79477679123556,0.463278392623556));
#69902=CARTESIAN_POINT('Ctrl Pts',(29.3249389282943,4.87104836864741,3.17284615441902));
#69903=CARTESIAN_POINT('Ctrl Pts',(29.4255088382521,2.76609490980042,5.11300145504481));
#69904=CARTESIAN_POINT('Ctrl Pts',(29.5260787482099,-0.00963418353934693,
5.81325830424054));
#69905=CARTESIAN_POINT('Ctrl Pts',(29.6266486581677,-2.78302699566422,5.10380501887743));
#69906=CARTESIAN_POINT('Ctrl Pts',(29.7272185681255,-4.88153815704996,3.15668340993825));
#69907=CARTESIAN_POINT('Ctrl Pts',(29.8277884780833,-5.79628051751914,0.444068791452662));
#69908=CARTESIAN_POINT('Ctrl Pts',(29.9283583880411,-5.30542984209442,-2.37623212669306));
#69909=CARTESIAN_POINT('Ctrl Pts',(30.0289282979989,-3.52801699702796,-4.62029879964445));
#69910=CARTESIAN_POINT('Ctrl Pts',(30.1294982079567,-0.895063067200426,
-5.74394699096779));
#69911=CARTESIAN_POINT('Ctrl Pts',(30.2300681179145,1.95494288592725,-5.47469298153573));
#69912=CARTESIAN_POINT('Ctrl Pts',(30.3306380278723,4.33087687208847,-3.87783063685398));
#69913=CARTESIAN_POINT('Ctrl Pts',(30.4312079378301,5.65657694491125,-1.34059770088297));
#69914=CARTESIAN_POINT('Ctrl Pts',(30.5317778477879,5.61056197793671,1.52172902352723));
#69915=CARTESIAN_POINT('Ctrl Pts',(30.6323477577457,4.20399056104516,4.01503776968005));
#69916=CARTESIAN_POINT('Ctrl Pts',(30.7329176677035,1.77795505201581,5.53470331294511));
#69917=CARTESIAN_POINT('Ctrl Pts',(30.8334875776613,-1.07923302661269,5.71220806725234));
#69918=CARTESIAN_POINT('Ctrl Pts',(30.9340574876192,-3.67470802532234,4.50450728248337));
#69919=CARTESIAN_POINT('Ctrl Pts',(31.0346273975769,-5.37906949118538,2.20446735932125));
#69920=CARTESIAN_POINT('Ctrl Pts',(31.1351973075348,-5.77901123589326,-0.63015400080755));
#69921=CARTESIAN_POINT('Ctrl Pts',(31.2357672174925,-4.7775477306356,-3.31196355819516));
#69922=CARTESIAN_POINT('Ctrl Pts',(31.3363371274504,-2.61753301334895,-5.19062480375363));
#69923=CARTESIAN_POINT('Ctrl Pts',(31.4369070374081,0.177231206427325,-5.81056400264058));
#69924=CARTESIAN_POINT('Ctrl Pts',(31.537476947366,2.92901701121071,-5.02144643278732));
#69925=CARTESIAN_POINT('Ctrl Pts',(31.6380468573237,4.97051871215735,-3.01463242558821));
#69926=CARTESIAN_POINT('Ctrl Pts',(31.7386167672815,5.80667390417087,-0.276772650265986));
#69927=CARTESIAN_POINT('Ctrl Pts',(31.8391866772394,5.23471567297435,2.52820425449188));
#69928=CARTESIAN_POINT('Ctrl Pts',(31.9397565871971,3.39334339727493,4.72009380388618));
#69929=CARTESIAN_POINT('Ctrl Pts',(32.040326497155,0.729088268823663,5.76736466903021));
#69930=CARTESIAN_POINT('Ctrl Pts',(32.1408964071127,-2.11197013719727,5.4160545666473));
#69931=CARTESIAN_POINT('Ctrl Pts',(32.2414663170706,-4.44087760299231,3.75135589414753));
#69932=CARTESIAN_POINT('Ctrl Pts',(32.3420362270283,-5.69287607289654,1.17695664659171));
#69933=CARTESIAN_POINT('Ctrl Pts',(32.4426061369862,-5.5643569957143,-1.68285357460456));
#69934=CARTESIAN_POINT('Ctrl Pts',(32.5431760469439,-4.08648613702948,-4.13457325260782));
#69935=CARTESIAN_POINT('Ctrl Pts',(32.6437459569018,-1.61764590787947,-5.58366247601294));
#69936=CARTESIAN_POINT('Ctrl Pts',(32.7443158668595,1.24347206141533,-5.67871835556173));
#69937=CARTESIAN_POINT('Ctrl Pts',(32.8448857768174,3.80304912623336,-4.39668992229039));
#69938=CARTESIAN_POINT('Ctrl Pts',(32.9454556867751,5.44039005171353,-2.04846796766039));
#69939=CARTESIAN_POINT('Ctrl Pts',(33.046025596733,5.75844107289692,0.796505705747263));
#69940=CARTESIAN_POINT('Ctrl Pts',(33.1465955066908,4.68007509093404,3.44832743116613));
#69941=CARTESIAN_POINT('Ctrl Pts',(33.2471654166486,2.46679492816254,5.26393272294638));
#69942=CARTESIAN_POINT('Ctrl Pts',(33.3477353266064,-0.344680881200578,
5.80303886075641));
#69943=CARTESIAN_POINT('Ctrl Pts',(33.4483052365642,-3.07257187358376,4.93491307025526));
#69944=CARTESIAN_POINT('Ctrl Pts',(33.548875146522,-5.05536683158087,2.87007510833188));
#69945=CARTESIAN_POINT('Ctrl Pts',(33.6494450564798,-5.81223968472432,0.109246403280997));
#69946=CARTESIAN_POINT('Ctrl Pts',(33.7500149664376,-5.15964941766476,-2.67807446052305));
#69947=CARTESIAN_POINT('Ctrl Pts',(33.8505848763954,-3.2558486083957,-4.81596457301359));
#69948=CARTESIAN_POINT('Ctrl Pts',(33.9511547863532,-0.562507314318525,
-5.78598742226877));
#69949=CARTESIAN_POINT('Ctrl Pts',(34.051724696311,2.26724151925849,-5.35291330236766));
#69950=CARTESIAN_POINT('Ctrl Pts',(34.1522946062688,4.54718623612184,-3.62176231458366));
#69951=CARTESIAN_POINT('Ctrl Pts',(34.2528645162266,5.72444220507391,-1.01233708322999));
#69952=CARTESIAN_POINT('Ctrl Pts',(34.3534344261844,5.5135258670596,1.84257901935812));
#69953=CARTESIAN_POINT('Ctrl Pts',(34.4540043361422,3.96558425248456,4.25067129589676));
#69954=CARTESIAN_POINT('Ctrl Pts',(34.5545742461,1.45599187037064,5.62797944228023));
#69955=CARTESIAN_POINT('Ctrl Pts',(34.6551441560578,-1.40667728694861,5.64050741863682));
#69956=CARTESIAN_POINT('Ctrl Pts',(34.7557140660156,-3.92822841309095,4.28521720148455));
#69957=CARTESIAN_POINT('Ctrl Pts',(34.8562839759734,-5.49718753059043,1.89076550181013));
#69958=CARTESIAN_POINT('Ctrl Pts',(34.9568538859312,-5.73308340405839,-0.962195204428082));
#69959=CARTESIAN_POINT('Ctrl Pts',(35.057423795889,-4.57871148724481,-3.58182440187771));
#69960=CARTESIAN_POINT('Ctrl Pts',(35.1579937058468,-2.31400597626052,-5.33286426520916));
#69961=CARTESIAN_POINT('Ctrl Pts',(35.2585636158045,0.511843992004246,-5.79068913490987));
#69962=CARTESIAN_POINT('Ctrl Pts',(35.3591335257624,3.21357223281796,-4.84427687418623));
#69963=CARTESIAN_POINT('Ctrl Pts',(35.4597034357202,5.13601197350847,-2.72313164156489));
#69964=CARTESIAN_POINT('Ctrl Pts',(35.560273345678,5.81297323184956,0.0583706699861391));
#69965=CARTESIAN_POINT('Ctrl Pts',(35.6608432556358,5.08029348544121,2.82571814431267));
#69966=CARTESIAN_POINT('Ctrl Pts',(35.7614131655936,3.11564694207568,4.9078314011026));
#69967=CARTESIAN_POINT('Ctrl Pts',(35.8619830755514,0.395458697295045,5.79979976792715));
#69968=CARTESIAN_POINT('Ctrl Pts',(35.9625529855092,-2.42062794115745,5.28532168366335));
#69969=CARTESIAN_POINT('Ctrl Pts',(36.063122895467,-4.64971438762522,3.48915764086767));
#69970=CARTESIAN_POINT('Ctrl Pts',(36.1636928054248,-5.75124909770136,0.846875873728528));
#69971=CARTESIAN_POINT('Ctrl Pts',(36.2642627153826,-5.45811085242508,-2.00077256377473));
#69972=CARTESIAN_POINT('Ctrl Pts',(36.3648326253404,-3.84138542393408,-4.36323537688503));
#69973=CARTESIAN_POINT('Ctrl Pts',(36.4654025352982,-1.29312733691379,-5.66761736709884));
#69974=CARTESIAN_POINT('Ctrl Pts',(36.565972445256,1.56871301614697,-5.59760702463875));
#69975=CARTESIAN_POINT('Ctrl Pts',(36.6665423552138,4.05014181318524,-4.17018179728447));
#69976=CARTESIAN_POINT('Ctrl Pts',(36.7671122651716,5.54941470700435,-1.73149107390076));
#69977=CARTESIAN_POINT('Ctrl Pts',(36.8676821751295,5.70295931147022,1.12708474438672));
#69978=CARTESIAN_POINT('Ctrl Pts',(36.9682520850872,4.47354119217547,3.71234348238731));
#69979=CARTESIAN_POINT('Ctrl Pts',(37.068821995045,2.15929318473071,5.39736212160066));
#69980=CARTESIAN_POINT('Ctrl Pts',(37.1693919050028,-0.678581561229704,
5.77352509252997));
#69981=CARTESIAN_POINT('Ctrl Pts',(37.2699618149606,-3.35190086273439,4.74961319853676));
#69982=CARTESIAN_POINT('Ctrl Pts',(37.3705317249185,-5.21238709043842,2.57392419250163));
#69983=CARTESIAN_POINT('Ctrl Pts',(37.4711016348762,-5.8088739356834,-0.225939214507409));
#69984=CARTESIAN_POINT('Ctrl Pts',(37.5716715448341,-4.99671385197042,-2.97101255649336));
#69985=CARTESIAN_POINT('Ctrl Pts',(37.6722414547918,-2.97285496046918,-4.99561791106246));
#69986=CARTESIAN_POINT('Ctrl Pts',(37.7728113647497,-0.228081300173006,
-5.80879022257005));
#69987=CARTESIAN_POINT('Ctrl Pts',(37.8733812747074,2.57200187907619,-5.21333590547767));
#69988=CARTESIAN_POINT('Ctrl Pts',(37.9739511846653,4.74837681670243,-3.35365211909601));
#69989=CARTESIAN_POINT('Ctrl Pts',(38.074521094623,5.77327446381726,-0.680710580753474));
#69990=CARTESIAN_POINT('Ctrl Pts',(38.1750910045808,5.39815802325663,2.15730268744658));
#69991=CARTESIAN_POINT('Ctrl Pts',(38.2756609145386,3.71399290894551,4.47217191100887));
#69992=CARTESIAN_POINT('Ctrl Pts',(38.3762308244964,1.1291877113267,5.70254329592533));
#69993=CARTESIAN_POINT('Ctrl Pts',(38.4768007344543,-1.72944453425166,5.55005284049271));
#69994=CARTESIAN_POINT('Ctrl Pts',(38.5773706444121,-4.16868796902945,4.05167934888527));
#69995=CARTESIAN_POINT('Ctrl Pts',(38.6779405543699,-5.59702815984374,1.57077710297491));
#69996=CARTESIAN_POINT('Ctrl Pts',(38.7785104643277,-5.6680938399783,-1.29103723823687));
#69997=CARTESIAN_POINT('Ctrl Pts',(38.8790803742854,-4.36465164317584,-3.8397761605381));
#69998=CARTESIAN_POINT('Ctrl Pts',(38.9796502842433,-2.00278518012054,-5.45737266929827));
#69999=CARTESIAN_POINT('Ctrl Pts',(39.080220194201,0.844754965059067,-5.75156100361652));
#70000=CARTESIAN_POINT('Ctrl Pts',(39.1807901041589,3.48744275840115,-4.65100074566642));
#70001=CARTESIAN_POINT('Ctrl Pts',(39.2813600141166,5.28442868492169,-2.42257681060703));
#70002=CARTESIAN_POINT('Ctrl Pts',(39.3819299240745,5.79994520433648,0.39331991560096));
#70003=CARTESIAN_POINT('Ctrl Pts',(39.4824998340322,4.90898000445885,3.11383690085679));
#70004=CARTESIAN_POINT('Ctrl Pts',(39.5830697439901,2.8275913792907,5.07925111813494));
#70005=CARTESIAN_POINT('Ctrl Pts',(39.6836396539479,0.0605142787163216,
5.8129513116304));
#70006=CARTESIAN_POINT('Ctrl Pts',(39.7842095639056,-2.72123748235436,5.13701581601069));
#70007=CARTESIAN_POINT('Ctrl Pts',(39.8847794738635,-4.84309149647335,3.21535840709891));
#70008=CARTESIAN_POINT('Ctrl Pts',(39.9853493838212,-5.79049999176961,0.513979352338406));
#70009=CARTESIAN_POINT('Ctrl Pts',(40.0859192937791,-5.33371722369023,-2.31203925291599));
#70010=CARTESIAN_POINT('Ctrl Pts',(40.1864892037368,-3.58351262028272,-4.57739032960799));
#70011=CARTESIAN_POINT('Ctrl Pts',(40.2870591136947,-0.964309291247043,
-5.73272819171892));
#70012=CARTESIAN_POINT('Ctrl Pts',(40.3876290236525,1.88873821081094,-5.49788440223482));
#70013=CARTESIAN_POINT('Ctrl Pts',(40.4881989336103,4.28376832262728,-3.92980837794532));
#70014=CARTESIAN_POINT('Ctrl Pts',(40.5887688435681,5.63998830379708,-1.40875720489588));
#70015=CARTESIAN_POINT('Ctrl Pts',(40.6893387535259,5.62851597635984,1.45391637764221));
#70016=CARTESIAN_POINT('Ctrl Pts',(40.7899086634837,4.25213336984329,3.964016490175));
#70017=CARTESIAN_POINT('Ctrl Pts',(40.8904785734415,1.84461208149807,5.51284601617945));
#70018=CARTESIAN_POINT('Ctrl Pts',(40.9910484833993,-1.01022604871547,5.7248151288763));
#70019=CARTESIAN_POINT('Ctrl Pts',(41.0916183933571,-3.62008523174703,4.54852150090567));
#70020=CARTESIAN_POINT('Ctrl Pts',(41.1921883033149,-5.3520768623531,2.2692153244632));
#70021=CARTESIAN_POINT('Ctrl Pts',(41.2927582132727,-5.78619446105984,-0.560373614755946));
#70022=CARTESIAN_POINT('Ctrl Pts',(41.3933281232305,-4.81716488388169,-3.25407243478249));
#70023=CARTESIAN_POINT('Ctrl Pts',(41.4938980331883,-2.6799769691159,-5.15866149057317));
#70024=CARTESIAN_POINT('Ctrl Pts',(41.5944679431461,0.107103053659489,-5.81227957562358));
#70025=CARTESIAN_POINT('Ctrl Pts',(41.6950378531039,2.8682106781198,-5.0564248669622));
#70026=CARTESIAN_POINT('Ctrl Pts',(41.7956077630617,4.93377968217404,-3.07439148077804));
#70027=CARTESIAN_POINT('Ctrl Pts',(41.8961776730195,5.80291136044017,-0.346820807029599));
#70028=CARTESIAN_POINT('Ctrl Pts',(41.9967475829773,5.26484202911207,2.46485361387027));
#70029=CARTESIAN_POINT('Ctrl Pts',(42.0973174929351,3.4500530378513,4.67880315522326));
#70030=CARTESIAN_POINT('Ctrl Pts',(42.1978874028929,0.798629154816186,5.75814695908256));
#70031=CARTESIAN_POINT('Ctrl Pts',(42.2984573128507,-2.04646161077897,5.44114508214238));
#70032=CARTESIAN_POINT('Ctrl Pts',(42.3990272228085,-4.39528719741307,3.80467020667639));
#70033=CARTESIAN_POINT('Ctrl Pts',(42.4995971327662,-5.67825942226375,1.24556608126063));
#70034=CARTESIAN_POINT('Ctrl Pts',(42.6001670427242,-5.58425862522408,-1.61558674664179));
#70035=CARTESIAN_POINT('Ctrl Pts',(42.7007369526818,-4.13607991865755,-4.08496117922704));
#70036=CARTESIAN_POINT('Ctrl Pts',(42.8013068626397,-1.68490539227271,-5.56373604230149));
#70037=CARTESIAN_POINT('Ctrl Pts',(42.9018767725975,1.1748572413234,-5.69330970454131));
#70038=CARTESIAN_POINT('Ctrl Pts',(43.0024466825553,3.74971800524932,-4.4422606643941));
#70039=CARTESIAN_POINT('Ctrl Pts',(43.1030165925131,5.41527538076706,-2.11396723715677));
#70040=CARTESIAN_POINT('Ctrl Pts',(43.2035865024709,5.76763313807318,0.726961425327436));
#70041=CARTESIAN_POINT('Ctrl Pts',(43.3041564124287,4.72134482434061,3.39160256795904));
#70042=CARTESIAN_POINT('Ctrl Pts',(43.4047263223865,2.5301344549744,5.23378300744937));
#70043=CARTESIAN_POINT('Ctrl Pts',(43.5052962323444,-0.274631341710833,
5.80677557302366));
#70044=CARTESIAN_POINT('Ctrl Pts',(43.6058661423021,-3.01279927444167,4.97163006077864));
#70045=CARTESIAN_POINT('Ctrl Pts',(43.7064360522599,-5.02036597662438,2.93086853851659));
#70046=CARTESIAN_POINT('Ctrl Pts',(43.8070059622177,-5.81049825115074,0.179373918639988));
#70047=CARTESIAN_POINT('Ctrl Pts',(43.9075758721755,-5.19158970161661,-2.61561872209666));
#70048=CARTESIAN_POINT('Ctrl Pts',(44.0081457821333,-3.31372511850974,-4.77632607432447));
#70049=CARTESIAN_POINT('Ctrl Pts',(44.1087156920912,-0.632285046713879,
-5.77877846512705));
#70050=CARTESIAN_POINT('Ctrl Pts',(44.2092856020489,2.202483604621,-5.37988205267457));
#70051=CARTESIAN_POINT('Ctrl Pts',(44.3098555120068,4.50315187779634,-3.67636887360525));
#70052=CARTESIAN_POINT('Ctrl Pts',(44.4104254219645,5.71180969704834,-1.08133940741041));
#70053=CARTESIAN_POINT('Ctrl Pts',(44.5109953319224,5.53535858165572,1.77591393423347));
#70054=CARTESIAN_POINT('Ctrl Pts',(44.6115652418801,4.01658777520697,4.20250967558343));
#70055=CARTESIAN_POINT('Ctrl Pts',(44.712135151838,1.52379789086441,5.61000043824521));
#70056=CARTESIAN_POINT('Ctrl Pts',(44.8127050617957,-1.33851167028378,5.65707092388173));
#70057=CARTESIAN_POINT('Ctrl Pts',(44.9132749717536,-3.87623330361735,4.33230658024589));
#70058=CARTESIAN_POINT('Ctrl Pts',(45.0138448817113,-5.47397169759653,1.95696162027419));
#70059=CARTESIAN_POINT('Ctrl Pts',(45.1144147916692,-5.74427666706043,-0.892944848005343));
#70060=CARTESIAN_POINT('Ctrl Pts',(45.2149847016269,-4.62159948960023,-3.52631295931618));
#70061=CARTESIAN_POINT('Ctrl Pts',(45.3155546115848,-2.3781884143173,-5.30455321354411));
#70062=CARTESIAN_POINT('Ctrl Pts',(45.4161245215426,0.441931304224746,-5.79644387979909));
#70063=CARTESIAN_POINT('Ctrl Pts',(45.5166944315003,3.15488306191939,-4.88270189494794));
#70064=CARTESIAN_POINT('Ctrl Pts',(45.6172643414582,5.1027783929124,-2.78490890374179));
#70065=CARTESIAN_POINT('Ctrl Pts',(45.717834251416,5.81325435624223,-0.0117779007076735));
#70066=CARTESIAN_POINT('Ctrl Pts',(45.8184041613737,5.11402114239932,2.76420923310936));
#70067=CARTESIAN_POINT('Ctrl Pts',(45.9189740713316,3.1746422038206,4.86987800740792));
#70068=CARTESIAN_POINT('Ctrl Pts',(46.0195439812894,0.465415263638452,5.79460555704065));
#70069=CARTESIAN_POINT('Ctrl Pts',(46.1201138912472,-2.35667447733314,5.3141462472537));
#70070=CARTESIAN_POINT('Ctrl Pts',(46.220683801205,-4.60727268624445,3.54501104707727));
#70071=CARTESIAN_POINT('Ctrl Pts',(46.3212537111628,-5.74061123481401,0.91621371963175));
#70072=CARTESIAN_POINT('Ctrl Pts',(46.4218236211205,-5.48185650062392,-1.93476464612143));
#70073=CARTESIAN_POINT('Ctrl Pts',(46.5223935310784,-3.89375628397183,-4.31656425069105));
#70074=CARTESIAN_POINT('Ctrl Pts',(46.6229634410361,-1.36142352031365,-5.65160074029039));
#70075=CARTESIAN_POINT('Ctrl Pts',(46.723533350994,1.50105327506819,-5.61612891542932));
#70076=CARTESIAN_POINT('Ctrl Pts',(46.8241032609517,3.99952594339569,-4.21875066310145));
#70077=CARTESIAN_POINT('Ctrl Pts',(46.9246731709096,5.52811701335638,-1.79832900659305));
#70078=CARTESIAN_POINT('Ctrl Pts',(47.0252430808674,5.71614446633981,1.05818588596099));
#70079=CARTESIAN_POINT('Ctrl Pts',(47.1258129908252,4.5180118068569,3.65809161208624));
#70080=CARTESIAN_POINT('Ctrl Pts',(47.226382900783,2.22426517344535,5.37091327127076));
#70081=CARTESIAN_POINT('Ctrl Pts',(47.3269528107408,-0.608863849815457,
5.78129308560828));
#70082=CARTESIAN_POINT('Ctrl Pts',(47.4275227206986,-3.29434391362348,4.78971430338867));
#70083=CARTESIAN_POINT('Ctrl Pts',(47.5280926306563,-5.18094841424352,2.63663392572076));
#70084=CARTESIAN_POINT('Ctrl Pts',(47.6286625406143,-5.8111773843185,-0.155827909244348));
#70085=CARTESIAN_POINT('Ctrl Pts',(47.729232450572,-5.03220084112436,-2.91050161035883));
#70086=CARTESIAN_POINT('Ctrl Pts',(47.8298023605298,-3.03291992582039,-4.95938117640456));
#70087=CARTESIAN_POINT('Ctrl Pts',(47.9303722704876,-0.298158539329414,
-5.80561507634972));
#70088=CARTESIAN_POINT('Ctrl Pts',(48.0309421804455,2.50890603628552,-5.24399231792002));
#70089=CARTESIAN_POINT('Ctrl Pts',(48.1315120904031,4.70756305783949,-3.41070593657371));
#70090=CARTESIAN_POINT('Ctrl Pts',(48.2320820003611,5.76464009027266,-0.750326301641742));
#70091=CARTESIAN_POINT('Ctrl Pts',(48.3326519103187,5.42379686318222,2.09200681553594));
#70092=CARTESIAN_POINT('Ctrl Pts',(48.4332218202766,3.76768756572999,4.42703008080563));
#70093=CARTESIAN_POINT('Ctrl Pts',(48.5337917302344,1.19791727692173,5.6885023623944));
#70094=CARTESIAN_POINT('Ctrl Pts',(48.6343616401922,-1.6623469203385,5.57051771792849));
#70095=CARTESIAN_POINT('Ctrl Pts',(48.73493155015,-4.11949342041254,4.10168732212634));
#70096=CARTESIAN_POINT('Ctrl Pts',(48.8355014601078,-5.57766631221463,1.63820128155862));
#70097=CARTESIAN_POINT('Ctrl Pts',(48.9360713700656,-5.68325992471977,-1.22254715957641));
#70098=CARTESIAN_POINT('Ctrl Pts',(49.0366412800234,-4.41066789779351,-3.78682896691783));
#70099=CARTESIAN_POINT('Ctrl Pts',(49.1372111899812,-2.06849270248174,-5.43280800959264));
#70100=CARTESIAN_POINT('Ctrl Pts',(49.2377810999391,0.775290192564016,-5.76133578665817));
#70101=CARTESIAN_POINT('Ctrl Pts',(49.3383510098967,3.43106588330503,-4.69274459498218));
#70102=CARTESIAN_POINT('Ctrl Pts',(49.4389209198547,5.25481105090448,-2.48616687867213));
#70103=CARTESIAN_POINT('Ctrl Pts',(49.5394908298124,5.80426906215165,0.323304165552166));
#70104=CARTESIAN_POINT('Ctrl Pts',(49.6400607397703,4.94619682230831,3.05437422793956));
#70105=CARTESIAN_POINT('Ctrl Pts',(49.740630649728,2.88867611088328,5.04476116934454));
#70106=CARTESIAN_POINT('Ctrl Pts',(49.8412005596858,0.130653929224284,5.81179786985854));
#70107=CARTESIAN_POINT('Ctrl Pts',(49.9417704696436,-2.65905171780094,5.16947858989416));
#70108=CARTESIAN_POINT('Ctrl Pts',(50.0423403796015,-4.80393961224742,3.27356520191584));
#70109=CARTESIAN_POINT('Ctrl Pts',(50.1429102895592,-5.78387628609288,0.583815070451743));
#70110=CARTESIAN_POINT('Ctrl Pts',(50.243480199517,-5.3612279394874,-2.24750971303215));
#70111=CARTESIAN_POINT('Ctrl Pts',(50.3440501094749,-3.63848643265499,-4.53381532582656));
#70112=CARTESIAN_POINT('Ctrl Pts',(50.4446200194326,-1.0334150980172,-5.72067462494628));
#70113=CARTESIAN_POINT('Ctrl Pts',(50.5451899293905,1.82225850829634,-5.52027525203731));
#70114=CARTESIAN_POINT('Ctrl Pts',(50.6457598393482,4.23603599500043,-3.98121388252061));
#70115=CARTESIAN_POINT('Ctrl Pts',(50.7463297493061,5.62257839941823,-1.47671157363573));
#70116=CARTESIAN_POINT('Ctrl Pts',(50.8468996592638,5.64565038205386,1.38589202066021));
#70117=CARTESIAN_POINT('Ctrl Pts',(50.9474695692217,4.29965700697908,3.91241799296163));
#70118=CARTESIAN_POINT('Ctrl Pts',(51.0480394791794,1.91100050897997,5.4901859698914));
#70119=CARTESIAN_POINT('Ctrl Pts',(51.1486093891373,-0.941071967402673,
5.73658857523205));
#70120=CARTESIAN_POINT('Ctrl Pts',(51.249179299095,-3.56493530179192,4.59187338929895));
#70121=CARTESIAN_POINT('Ctrl Pts',(51.3497492090528,-5.32430489429523,2.33363285927715));
#70122=CARTESIAN_POINT('Ctrl Pts',(51.4503191190107,-5.79253513324631,-0.490511630261341));
#70123=CARTESIAN_POINT('Ctrl Pts',(51.5508890289684,-4.85608058876542,-3.19570747170793));
#70124=CARTESIAN_POINT('Ctrl Pts',(51.6514589389262,-2.74203068176238,-5.12594700222191));
#70125=CARTESIAN_POINT('Ctrl Pts',(51.7520288488841,0.036959305149328,-5.81314879725927));
#70126=CARTESIAN_POINT('Ctrl Pts',(51.8525987588419,2.80698669237795,-5.09066701308651));
#70127=CARTESIAN_POINT('Ctrl Pts',(51.9531686687997,4.89632222303964,-3.13370286043244));
#70128=CARTESIAN_POINT('Ctrl Pts',(52.0537385787575,5.79830382950879,-0.41681846170471));
#70129=CARTESIAN_POINT('Ctrl Pts',(52.1543084887152,5.29420174866827,2.4011440551771));
#70130=CARTESIAN_POINT('Ctrl Pts',(52.2548783986731,3.50626030117625,4.63683120565213));
#70131=CARTESIAN_POINT('Ctrl Pts',(52.3554483086308,0.868053748938764,5.74809078027364));
#70132=CARTESIAN_POINT('Ctrl Pts',(52.4560182185887,-1.98065509017138,5.46544328880053));
#70133=CARTESIAN_POINT('Ctrl Pts',(52.5565881285464,-4.34905677491859,3.85743050460308));
#70134=CARTESIAN_POINT('Ctrl Pts',(52.6571580385043,-5.6628159355431,1.31399414362717));
#70135=CARTESIAN_POINT('Ctrl Pts',(52.7577279484621,-5.60334710650831,-1.54808466605653));
#70136=CARTESIAN_POINT('Ctrl Pts',(52.8582978584198,-4.18507142767569,-4.03475427685318));
#70137=CARTESIAN_POINT('Ctrl Pts',(52.9588677683777,-1.75191953024455,-5.54299944875284));
#70138=CARTESIAN_POINT('Ctrl Pts',(53.0594376783355,1.10607134513556,-5.70707202588776));
#70139=CARTESIAN_POINT('Ctrl Pts',(53.1600075882933,3.69584087152237,-4.48718454958579));
#70140=CARTESIAN_POINT('Ctrl Pts',(53.2605774982511,5.38937216792545,-2.1791586826484));
#70141=CARTESIAN_POINT('Ctrl Pts',(53.3611474082089,5.77598535317805,0.657311288835543));
#70142=CARTESIAN_POINT('Ctrl Pts',(53.4617173181667,4.76192706193859,3.33438383883116));
#70143=CARTESIAN_POINT('Ctrl Pts',(53.5622872281245,2.59310555832215,5.2028711778091));
#70144=CARTESIAN_POINT('Ctrl Pts',(53.6628571380823,-0.204541812806597,
5.80966673579904));
#70145=CARTESIAN_POINT('Ctrl Pts',(53.7634270480401,-2.95258796680689,5.00762310982228));
#70146=CARTESIAN_POINT('Ctrl Pts',(53.8639969579978,-4.98463408757047,2.99123519367383));
#70147=CARTESIAN_POINT('Ctrl Pts',(53.9645668679557,-5.8079107192347,0.249475311631604));
#70148=CARTESIAN_POINT('Ctrl Pts',(54.0651367779134,-5.22277402806538,-2.55278210626261));
#70149=CARTESIAN_POINT('Ctrl Pts',(54.1657066878714,-3.37111907823718,-4.73599208528508));
#70150=CARTESIAN_POINT('Ctrl Pts',(54.2662765978291,-0.701970757150338,
-5.77072801277767));
#70151=CARTESIAN_POINT('Ctrl Pts',(54.3668465077869,2.13740507033186,-5.40606745817384));
#70152=CARTESIAN_POINT('Ctrl Pts',(54.4674164177447,4.45846161278591,-3.73044001590026));
#70153=CARTESIAN_POINT('Ctrl Pts',(54.5679863277025,5.69834582588392,-1.15018443868033));
#70154=CARTESIAN_POINT('Ctrl Pts',(54.6685562376603,5.55638456732653,1.70899057466459));
#70155=CARTESIAN_POINT('Ctrl Pts',(54.7691261476182,4.06700779734722,4.15373547526812));
#70156=CARTESIAN_POINT('Ctrl Pts',(54.8696960575759,1.59137933916517,5.59120577878235));
#70157=CARTESIAN_POINT('Ctrl Pts',(54.9702659675337,-1.27014589220361,5.67280824955481));
#70158=CARTESIAN_POINT('Ctrl Pts',(55.0708358774915,-3.82368404225601,4.37876986600632));
#70159=CARTESIAN_POINT('Ctrl Pts',(55.1714057874494,-5.44993865105018,2.02286347478549));
#70160=CARTESIAN_POINT('Ctrl Pts',(55.271975697407,-5.75467287847216,-0.82354625023189));
#70161=CARTESIAN_POINT('Ctrl Pts',(55.372545607365,-4.66373725166594,-3.47032381488753));
#70162=CARTESIAN_POINT('Ctrl Pts',(55.4731155173227,-2.44217762540687,-5.27539828092228));
#70163=CARTESIAN_POINT('Ctrl Pts',(55.5736854272806,0.372273903066788,-5.80150997087913));
#70164=CARTESIAN_POINT('Ctrl Pts',(55.6407320339191,2.18734716132424,-5.21379159096135));
#70165=CARTESIAN_POINT('Ctrl Pts',(55.6742553372383,2.970363104022,-4.72114838740161));
#70166=CARTESIAN_POINT('Ctrl Pts',(55.26731,3.34571636511758,-5.31774159209381));
#70167=CARTESIAN_POINT('Ctrl Pts',(55.2337866966807,2.46375373567184,-5.8726382059394));
#70168=CARTESIAN_POINT('Ctrl Pts',(55.2002633933615,1.44153522376391,-6.20363124162395));
#70169=CARTESIAN_POINT('Ctrl Pts',(55.1667400900422,0.402075493031596,-6.27036202896318));
#70170=CARTESIAN_POINT('Ctrl Pts',(55.1332167867229,-0.637384237700717,
-6.33709281630241));
#70171=CARTESIAN_POINT('Ctrl Pts',(55.0996934834037,-1.69408518725741,-6.13956135529632));
#70172=CARTESIAN_POINT('Ctrl Pts',(55.0661701800844,-2.63948391154636,-5.70193317095775));
#70173=CARTESIAN_POINT('Ctrl Pts',(55.0326468767652,-3.58488263583531,-5.26430498661918));
#70174=CARTESIAN_POINT('Ctrl Pts',(54.9991235734459,-4.41897913485652,-4.58658007894814));
#70175=CARTESIAN_POINT('Ctrl Pts',(54.9656002701266,-5.04082620592946,-3.75084419568217));
#70176=CARTESIAN_POINT('Ctrl Pts',(54.9320769668074,-5.66267327700243,-2.91510831241616));
#70177=CARTESIAN_POINT('Ctrl Pts',(54.898553663488,-6.07227092012711,-1.92136145355521));
#70178=CARTESIAN_POINT('Ctrl Pts',(54.8650303601688,-6.21986269011626,-0.890138111038006));
#70179=CARTESIAN_POINT('Ctrl Pts',(54.8554530504693,-6.26202834654978,-0.595526770785087));
#70180=CARTESIAN_POINT('Ctrl Pts',(54.8458757407699,-6.28280923827804,-0.297856622058228));
#70181=CARTESIAN_POINT('Ctrl Pts',(54.8362984310704,-6.28252994889952,-0.000148679754663761));
#70182=CARTESIAN_POINT('Origin',(37.,0.,0.));
#70183=CARTESIAN_POINT('Origin',(0.6,7.15372402116488,-1.00753790450219));
#70184=CARTESIAN_POINT('',(17.4,7.09390928188606,-1.04180185273915));
#70185=CARTESIAN_POINT('',(0.600000000000001,7.09390928188606,-1.04180185273915));
#70186=CARTESIAN_POINT('',(9.,7.09390928188606,-1.04180185273915));
#70187=CARTESIAN_POINT('',(17.4,6.81486965084448,-1.20164538945516));
#70188=CARTESIAN_POINT('',(17.4,7.15372402116488,-1.00753790450219));
#70189=CARTESIAN_POINT('',(0.6,6.81486965084448,-1.20164538945516));
#70190=CARTESIAN_POINT('',(0.6,6.81486965084448,-1.20164538945516));
#70191=CARTESIAN_POINT('',(0.6,7.15372402116488,-1.00753790450219));
#70192=CARTESIAN_POINT('Origin',(0.6,6.96259081379631,-1.2276926161052));
#70193=CARTESIAN_POINT('',(0.600000000000001,7.02241142370379,-1.4472863559899));
#70194=CARTESIAN_POINT('Origin',(0.600000000000001,0.,0.));
#70195=CARTESIAN_POINT('',(0.6,6.81486965084448,-1.20164538945516));
#70196=CARTESIAN_POINT('Origin',(0.6,6.81486965084448,-1.20164538945516));
#70197=CARTESIAN_POINT('',(17.4,7.02241142370379,-1.4472863559899));
#70198=CARTESIAN_POINT('',(9.,7.02241142370379,-1.4472863559899));
#70199=CARTESIAN_POINT('',(17.4,6.81486965084448,-1.20164538945516));
#70200=CARTESIAN_POINT('Origin',(17.4,6.96259081379631,-1.2276926161052));
#70201=CARTESIAN_POINT('Origin',(17.4,0.,0.));
#70202=CARTESIAN_POINT('Origin',(0.6,6.87008575790567,-2.23446227961486));
#70203=CARTESIAN_POINT('',(17.4,6.80522986674848,-2.25781896101404));
#70204=CARTESIAN_POINT('',(0.600000000000001,6.80522986674848,-2.25781896101404));
#70205=CARTESIAN_POINT('',(9.,6.80522986674848,-2.25781896101404));
#70206=CARTESIAN_POINT('',(17.4,6.50267293583848,-2.36677939181363));
#70207=CARTESIAN_POINT('',(17.4,6.87008575790567,-2.23446227961486));
#70208=CARTESIAN_POINT('',(0.6,6.50267293583848,-2.36677939181363));
#70209=CARTESIAN_POINT('',(0.6,6.50267293583848,-2.36677939181363));
#70210=CARTESIAN_POINT('',(0.6,6.87008575790567,-2.23446227961486));
#70211=CARTESIAN_POINT('Origin',(0.6,6.64362682895637,-2.41808241331248));
#70212=CARTESIAN_POINT('',(0.600000000000001,6.66440657662513,-2.64472777076124));
#70213=CARTESIAN_POINT('Origin',(0.600000000000001,0.,0.));
#70214=CARTESIAN_POINT('',(0.6,6.50267293583848,-2.36677939181363));
#70215=CARTESIAN_POINT('Origin',(0.6,6.50267293583848,-2.36677939181363));
#70216=CARTESIAN_POINT('',(17.4,6.66440657662513,-2.64472777076124));
#70217=CARTESIAN_POINT('',(9.,6.66440657662513,-2.64472777076124));
#70218=CARTESIAN_POINT('',(17.4,6.50267293583848,-2.36677939181363));
#70219=CARTESIAN_POINT('Origin',(17.4,6.64362682895637,-2.41808241331248));
#70220=CARTESIAN_POINT('Origin',(17.4,0.,0.));
#70221=CARTESIAN_POINT('Origin',(0.6,6.37770341532365,-3.39349364905389));
#70222=CARTESIAN_POINT('',(17.4,6.3097769857222,-3.40523338267004));
#70223=CARTESIAN_POINT('',(0.600000000000001,6.3097769857222,-3.40523338267004));
#70224=CARTESIAN_POINT('',(9.,6.3097769857222,-3.40523338267003));
#70225=CARTESIAN_POINT('',(17.4,5.99289579418831,-3.46));
#70226=CARTESIAN_POINT('',(17.4,6.37770341532365,-3.39349364905389));
#70227=CARTESIAN_POINT('',(0.6,5.99289579418831,-3.46));
#70228=CARTESIAN_POINT('',(0.6,5.99289579418831,-3.46));
#70229=CARTESIAN_POINT('',(0.6,6.37770341532365,-3.39349364905389));
#70230=CARTESIAN_POINT('Origin',(0.6,6.12279960475598,-3.535));
#70231=CARTESIAN_POINT('',(0.600000000000001,6.10390710806817,-3.76181047051482));
#70232=CARTESIAN_POINT('Origin',(0.600000000000001,0.,0.));
#70233=CARTESIAN_POINT('',(0.6,5.99289579418831,-3.46));
#70234=CARTESIAN_POINT('Origin',(0.6,5.99289579418831,-3.46));
#70235=CARTESIAN_POINT('',(17.4,6.10390710806817,-3.76181047051482));
#70236=CARTESIAN_POINT('',(9.,6.10390710806817,-3.76181047051482));
#70237=CARTESIAN_POINT('',(17.4,5.99289579418831,-3.46));
#70238=CARTESIAN_POINT('Origin',(17.4,6.12279960475598,-3.535));
#70239=CARTESIAN_POINT('Origin',(17.4,0.,0.));
#70240=CARTESIAN_POINT('Origin',(0.6,5.69153778174065,-4.44941543115707));
#70241=CARTESIAN_POINT('',(17.4,5.62260472388598,-4.44918151112483));
#70242=CARTESIAN_POINT('',(0.600000000000001,5.62260472388598,-4.44918151112483));
#70243=CARTESIAN_POINT('',(9.,5.62260472388598,-4.44918151112483));
#70244=CARTESIAN_POINT('',(17.4,5.30102754638333,-4.44809025903085));
#70245=CARTESIAN_POINT('',(17.4,5.69153778174065,-4.44941543115707));
#70246=CARTESIAN_POINT('',(0.6,5.30102754638333,-4.44809025903085));
#70247=CARTESIAN_POINT('',(0.6,5.30102754638333,-4.44809025903085));
#70248=CARTESIAN_POINT('',(0.6,5.69153778174065,-4.44941543115707));
#70249=CARTESIAN_POINT('Origin',(0.6,5.41593421285117,-4.54450840048383));
#70250=CARTESIAN_POINT('',(0.599999999999999,5.35794351075858,-4.76459246268976));
#70251=CARTESIAN_POINT('Origin',(0.600000000000001,0.,0.));
#70252=CARTESIAN_POINT('',(0.6,5.30102754638333,-4.44809025903085));
#70253=CARTESIAN_POINT('Origin',(0.6,5.30102754638333,-4.44809025903085));
#70254=CARTESIAN_POINT('',(17.4,5.35794351075858,-4.76459246268976));
#70255=CARTESIAN_POINT('',(9.,5.35794351075858,-4.76459246268976));
#70256=CARTESIAN_POINT('',(17.4,5.30102754638333,-4.44809025903085));
#70257=CARTESIAN_POINT('Origin',(17.4,5.41593421285117,-4.54450840048383));
#70258=CARTESIAN_POINT('Origin',(17.4,0.,0.));
#70259=CARTESIAN_POINT('Origin',(0.6,4.83243765271656,-5.37014397689739));
#70260=CARTESIAN_POINT('',(17.4,4.76459246268975,-5.35794351075858));
#70261=CARTESIAN_POINT('',(0.600000000000001,4.76459246268975,-5.35794351075858));
#70262=CARTESIAN_POINT('',(9.,4.76459246268975,-5.35794351075858));
#70263=CARTESIAN_POINT('',(17.4,4.44809025903085,-5.30102754638333));
#70264=CARTESIAN_POINT('',(17.4,4.83243765271656,-5.37014397689739));
#70265=CARTESIAN_POINT('',(0.6,4.44809025903085,-5.30102754638333));
#70266=CARTESIAN_POINT('',(0.6,4.44809025903085,-5.30102754638333));
#70267=CARTESIAN_POINT('',(0.6,4.83243765271656,-5.37014397689739));
#70268=CARTESIAN_POINT('Origin',(0.6,4.54450840048383,-5.41593421285118));
#70269=CARTESIAN_POINT('',(0.600000000000001,4.44918151112483,-5.62260472388598));
#70270=CARTESIAN_POINT('Origin',(0.600000000000001,0.,0.));
#70271=CARTESIAN_POINT('',(0.6,4.44809025903085,-5.30102754638333));
#70272=CARTESIAN_POINT('Origin',(0.6,4.44809025903085,-5.30102754638333));
#70273=CARTESIAN_POINT('',(17.4,4.44918151112483,-5.62260472388598));
#70274=CARTESIAN_POINT('',(9.,4.44918151112483,-5.62260472388598));
#70275=CARTESIAN_POINT('',(17.4,4.44809025903085,-5.30102754638333));
#70276=CARTESIAN_POINT('Origin',(17.4,4.54450840048383,-5.41593421285118));
#70277=CARTESIAN_POINT('Origin',(17.4,0.,0.));
#70278=CARTESIAN_POINT('Origin',(0.6,3.82650635094611,-6.12770341532365));
#70279=CARTESIAN_POINT('',(17.4,3.76181047051482,-6.10390710806817));
#70280=CARTESIAN_POINT('',(0.599999999999999,3.76181047051482,-6.10390710806817));
#70281=CARTESIAN_POINT('',(9.,3.76181047051482,-6.10390710806817));
#70282=CARTESIAN_POINT('',(17.4,3.46,-5.99289579418831));
#70283=CARTESIAN_POINT('',(17.4,3.82650635094611,-6.12770341532365));
#70284=CARTESIAN_POINT('',(0.6,3.46,-5.99289579418831));
#70285=CARTESIAN_POINT('',(0.6,3.46,-5.99289579418831));
#70286=CARTESIAN_POINT('',(0.6,3.82650635094611,-6.12770341532365));
#70287=CARTESIAN_POINT('Origin',(0.6,3.535,-6.12279960475598));
#70288=CARTESIAN_POINT('',(0.599999999999999,3.40523338267003,-6.30977698572221));
#70289=CARTESIAN_POINT('Origin',(0.600000000000001,0.,0.));
#70290=CARTESIAN_POINT('',(0.6,3.46,-5.99289579418831));
#70291=CARTESIAN_POINT('Origin',(0.6,3.46,-5.99289579418831));
#70292=CARTESIAN_POINT('',(17.4,3.40523338267003,-6.30977698572221));
#70293=CARTESIAN_POINT('',(9.,3.40523338267003,-6.30977698572221));
#70294=CARTESIAN_POINT('',(17.4,3.46,-5.99289579418831));
#70295=CARTESIAN_POINT('Origin',(17.4,3.535,-6.12279960475598));
#70296=CARTESIAN_POINT('Origin',(17.4,0.,0.));
#70297=CARTESIAN_POINT('Origin',(0.6,2.7043085900078,-6.69907568624284));
#70298=CARTESIAN_POINT('',(17.4,2.64472777076123,-6.66440657662513));
#70299=CARTESIAN_POINT('',(0.599999999999999,2.64472777076123,-6.66440657662513));
#70300=CARTESIAN_POINT('',(9.,2.64472777076123,-6.66440657662513));
#70301=CARTESIAN_POINT('',(17.4,2.36677939181362,-6.50267293583849));
#70302=CARTESIAN_POINT('',(17.4,2.7043085900078,-6.69907568624284));
#70303=CARTESIAN_POINT('',(0.6,2.36677939181362,-6.50267293583849));
#70304=CARTESIAN_POINT('',(0.6,2.36677939181362,-6.50267293583849));
#70305=CARTESIAN_POINT('',(0.6,2.7043085900078,-6.69907568624284));
#70306=CARTESIAN_POINT('Origin',(0.6,2.41808241331247,-6.64362682895637));
#70307=CARTESIAN_POINT('',(0.600000000000001,2.25781896101403,-6.80522986674848));
#70308=CARTESIAN_POINT('Origin',(0.600000000000001,0.,0.));
#70309=CARTESIAN_POINT('',(0.6,2.36677939181362,-6.50267293583849));
#70310=CARTESIAN_POINT('Origin',(0.6,2.36677939181362,-6.50267293583849));
#70311=CARTESIAN_POINT('',(17.4,2.25781896101403,-6.80522986674848));
#70312=CARTESIAN_POINT('',(9.,2.25781896101403,-6.80522986674848));
#70313=CARTESIAN_POINT('',(17.4,2.36677939181362,-6.50267293583849));
#70314=CARTESIAN_POINT('Origin',(17.4,2.41808241331247,-6.64362682895637));
#70315=CARTESIAN_POINT('Origin',(17.4,0.,0.));
#70316=CARTESIAN_POINT('Origin',(0.6,1.49994178100829,-7.06689993233141));
#70317=CARTESIAN_POINT('',(17.4,1.44728635598989,-7.02241142370379));
#70318=CARTESIAN_POINT('',(0.600000000000001,1.44728635598989,-7.02241142370379));
#70319=CARTESIAN_POINT('',(9.,1.44728635598989,-7.02241142370379));
#70320=CARTESIAN_POINT('',(17.4,1.20164538945516,-6.81486965084448));
#70321=CARTESIAN_POINT('',(17.4,1.49994178100829,-7.06689993233141));
#70322=CARTESIAN_POINT('',(0.6,1.20164538945516,-6.81486965084448));
#70323=CARTESIAN_POINT('',(0.6,1.20164538945516,-6.81486965084448));
#70324=CARTESIAN_POINT('',(0.6,1.49994178100829,-7.06689993233141));
#70325=CARTESIAN_POINT('Origin',(0.6,1.22769261610519,-6.96259081379631));
#70326=CARTESIAN_POINT('',(0.600000000000001,1.04180185273915,-7.09390928188606));
#70327=CARTESIAN_POINT('Origin',(0.600000000000001,0.,0.));
#70328=CARTESIAN_POINT('',(0.6,1.20164538945516,-6.81486965084448));
#70329=CARTESIAN_POINT('Origin',(0.6,1.20164538945516,-6.81486965084448));
#70330=CARTESIAN_POINT('',(17.4,1.04180185273915,-7.09390928188606));
#70331=CARTESIAN_POINT('',(9.,1.04180185273915,-7.09390928188607));
#70332=CARTESIAN_POINT('',(17.4,1.20164538945516,-6.81486965084448));
#70333=CARTESIAN_POINT('Origin',(17.4,1.22769261610519,-6.96259081379631));
#70334=CARTESIAN_POINT('Origin',(17.4,0.,0.));
#70335=CARTESIAN_POINT('Origin',(0.6,0.249999999999999,-7.22));
#70336=CARTESIAN_POINT('',(17.4,0.205869877654039,-7.16704385318485));
#70337=CARTESIAN_POINT('',(0.599999999999999,0.205869877654039,-7.16704385318485));
#70338=CARTESIAN_POINT('',(9.,0.205869877654039,-7.16704385318485));
#70339=CARTESIAN_POINT('',(17.4,-1.27118337751495E-15,-6.92));
#70340=CARTESIAN_POINT('',(17.4,0.249999999999999,-7.22));
#70341=CARTESIAN_POINT('',(0.6,-1.27118337751495E-15,-6.92));
#70342=CARTESIAN_POINT('',(0.6,-1.27118337751495E-15,-6.92));
#70343=CARTESIAN_POINT('',(0.6,0.249999999999999,-7.22));
#70344=CARTESIAN_POINT('Origin',(0.6,-1.29873793049577E-15,-7.07));
#70345=CARTESIAN_POINT('',(0.600000000000001,-0.20586987765404,-7.16704385318485));
#70346=CARTESIAN_POINT('Origin',(0.600000000000001,0.,0.));
#70347=CARTESIAN_POINT('',(0.6,-1.27118337751495E-15,-6.92));
#70348=CARTESIAN_POINT('Origin',(0.6,-1.27118337751495E-15,-6.92));
#70349=CARTESIAN_POINT('',(17.4,-0.20586987765404,-7.16704385318485));
#70350=CARTESIAN_POINT('',(9.,-0.20586987765404,-7.16704385318485));
#70351=CARTESIAN_POINT('',(17.4,-1.27118337751495E-15,-6.92));
#70352=CARTESIAN_POINT('Origin',(17.4,-1.29873793049577E-15,-7.07));
#70353=CARTESIAN_POINT('Origin',(17.4,0.,0.));
#70354=CARTESIAN_POINT('Origin',(0.6,-1.00753790450219,-7.15372402116488));
#70355=CARTESIAN_POINT('',(17.4,-1.04180185273915,-7.09390928188606));
#70356=CARTESIAN_POINT('',(0.600000000000001,-1.04180185273915,-7.09390928188606));
#70357=CARTESIAN_POINT('',(9.,-1.04180185273915,-7.09390928188606));
#70358=CARTESIAN_POINT('',(17.4,-1.20164538945516,-6.81486965084448));
#70359=CARTESIAN_POINT('',(17.4,-1.00753790450219,-7.15372402116488));
#70360=CARTESIAN_POINT('',(0.6,-1.20164538945516,-6.81486965084448));
#70361=CARTESIAN_POINT('',(0.6,-1.20164538945516,-6.81486965084448));
#70362=CARTESIAN_POINT('',(0.6,-1.00753790450219,-7.15372402116488));
#70363=CARTESIAN_POINT('Origin',(0.6,-1.2276926161052,-6.96259081379631));
#70364=CARTESIAN_POINT('',(0.600000000000001,-1.4472863559899,-7.02241142370379));
#70365=CARTESIAN_POINT('Origin',(0.600000000000001,0.,0.));
#70366=CARTESIAN_POINT('',(0.6,-1.20164538945516,-6.81486965084448));
#70367=CARTESIAN_POINT('Origin',(0.6,-1.20164538945516,-6.81486965084448));
#70368=CARTESIAN_POINT('',(17.4,-1.4472863559899,-7.02241142370379));
#70369=CARTESIAN_POINT('',(9.,-1.4472863559899,-7.02241142370379));
#70370=CARTESIAN_POINT('',(17.4,-1.20164538945516,-6.81486965084448));
#70371=CARTESIAN_POINT('Origin',(17.4,-1.2276926161052,-6.96259081379631));
#70372=CARTESIAN_POINT('Origin',(17.4,0.,0.));
#70373=CARTESIAN_POINT('Origin',(0.6,-2.23446227961486,-6.87008575790567));
#70374=CARTESIAN_POINT('',(17.4,-2.25781896101404,-6.80522986674848));
#70375=CARTESIAN_POINT('',(0.600000000000001,-2.25781896101404,-6.80522986674848));
#70376=CARTESIAN_POINT('',(9.,-2.25781896101404,-6.80522986674847));
#70377=CARTESIAN_POINT('',(17.4,-2.36677939181363,-6.50267293583848));
#70378=CARTESIAN_POINT('',(17.4,-2.23446227961486,-6.87008575790567));
#70379=CARTESIAN_POINT('',(0.6,-2.36677939181363,-6.50267293583848));
#70380=CARTESIAN_POINT('',(0.6,-2.36677939181363,-6.50267293583848));
#70381=CARTESIAN_POINT('',(0.6,-2.23446227961486,-6.87008575790567));
#70382=CARTESIAN_POINT('Origin',(0.6,-2.41808241331248,-6.64362682895637));
#70383=CARTESIAN_POINT('',(0.600000000000001,-2.64472777076124,-6.66440657662513));
#70384=CARTESIAN_POINT('Origin',(0.600000000000001,0.,0.));
#70385=CARTESIAN_POINT('',(0.6,-2.36677939181363,-6.50267293583848));
#70386=CARTESIAN_POINT('Origin',(0.6,-2.36677939181363,-6.50267293583848));
#70387=CARTESIAN_POINT('',(17.4,-2.64472777076124,-6.66440657662513));
#70388=CARTESIAN_POINT('',(9.,-2.64472777076124,-6.66440657662513));
#70389=CARTESIAN_POINT('',(17.4,-2.36677939181363,-6.50267293583848));
#70390=CARTESIAN_POINT('Origin',(17.4,-2.41808241331248,-6.64362682895637));
#70391=CARTESIAN_POINT('Origin',(17.4,0.,0.));
#70392=CARTESIAN_POINT('Origin',(0.6,-3.39349364905389,-6.37770341532365));
#70393=CARTESIAN_POINT('',(17.4,-3.40523338267004,-6.3097769857222));
#70394=CARTESIAN_POINT('',(0.600000000000001,-3.40523338267004,-6.3097769857222));
#70395=CARTESIAN_POINT('',(9.,-3.40523338267003,-6.3097769857222));
#70396=CARTESIAN_POINT('',(17.4,-3.46,-5.99289579418831));
#70397=CARTESIAN_POINT('',(17.4,-3.39349364905389,-6.37770341532365));
#70398=CARTESIAN_POINT('',(0.6,-3.46,-5.99289579418831));
#70399=CARTESIAN_POINT('',(0.6,-3.46,-5.99289579418831));
#70400=CARTESIAN_POINT('',(0.6,-3.39349364905389,-6.37770341532365));
#70401=CARTESIAN_POINT('Origin',(0.6,-3.535,-6.12279960475598));
#70402=CARTESIAN_POINT('',(0.600000000000001,-3.76181047051482,-6.10390710806817));
#70403=CARTESIAN_POINT('Origin',(0.600000000000001,0.,0.));
#70404=CARTESIAN_POINT('',(0.6,-3.46,-5.99289579418831));
#70405=CARTESIAN_POINT('Origin',(0.6,-3.46,-5.99289579418831));
#70406=CARTESIAN_POINT('',(17.4,-3.76181047051482,-6.10390710806817));
#70407=CARTESIAN_POINT('',(9.,-3.76181047051482,-6.10390710806817));
#70408=CARTESIAN_POINT('',(17.4,-3.46,-5.99289579418831));
#70409=CARTESIAN_POINT('Origin',(17.4,-3.535,-6.12279960475598));
#70410=CARTESIAN_POINT('Origin',(17.4,0.,0.));
#70411=CARTESIAN_POINT('Origin',(0.6,-4.44941543115707,-5.69153778174066));
#70412=CARTESIAN_POINT('',(17.4,-4.44918151112483,-5.62260472388598));
#70413=CARTESIAN_POINT('',(0.599999999999999,-4.44918151112483,-5.62260472388598));
#70414=CARTESIAN_POINT('',(9.,-4.44918151112483,-5.62260472388598));
#70415=CARTESIAN_POINT('',(17.4,-4.44809025903085,-5.30102754638333));
#70416=CARTESIAN_POINT('',(17.4,-4.44941543115707,-5.69153778174066));
#70417=CARTESIAN_POINT('',(0.6,-4.44809025903085,-5.30102754638333));
#70418=CARTESIAN_POINT('',(0.6,-4.44809025903085,-5.30102754638333));
#70419=CARTESIAN_POINT('',(0.6,-4.44941543115707,-5.69153778174066));
#70420=CARTESIAN_POINT('Origin',(0.6,-4.54450840048383,-5.41593421285117));
#70421=CARTESIAN_POINT('',(0.599999999999999,-4.76459246268976,-5.35794351075858));
#70422=CARTESIAN_POINT('Origin',(0.600000000000001,0.,0.));
#70423=CARTESIAN_POINT('',(0.6,-4.44809025903085,-5.30102754638333));
#70424=CARTESIAN_POINT('Origin',(0.6,-4.44809025903085,-5.30102754638333));
#70425=CARTESIAN_POINT('',(17.4,-4.76459246268976,-5.35794351075858));
#70426=CARTESIAN_POINT('',(9.,-4.76459246268976,-5.35794351075858));
#70427=CARTESIAN_POINT('',(17.4,-4.44809025903085,-5.30102754638333));
#70428=CARTESIAN_POINT('Origin',(17.4,-4.54450840048383,-5.41593421285117));
#70429=CARTESIAN_POINT('Origin',(17.4,0.,0.));
#70430=CARTESIAN_POINT('Origin',(0.6,-5.37014397689739,-4.83243765271656));
#70431=CARTESIAN_POINT('',(17.4,-5.35794351075858,-4.76459246268975));
#70432=CARTESIAN_POINT('',(0.599999999999999,-5.35794351075858,-4.76459246268975));
#70433=CARTESIAN_POINT('',(9.,-5.35794351075858,-4.76459246268975));
#70434=CARTESIAN_POINT('',(17.4,-5.30102754638333,-4.44809025903085));
#70435=CARTESIAN_POINT('',(17.4,-5.37014397689739,-4.83243765271656));
#70436=CARTESIAN_POINT('',(0.6,-5.30102754638333,-4.44809025903085));
#70437=CARTESIAN_POINT('',(0.6,-5.30102754638333,-4.44809025903085));
#70438=CARTESIAN_POINT('',(0.6,-5.37014397689739,-4.83243765271656));
#70439=CARTESIAN_POINT('Origin',(0.6,-5.41593421285118,-4.54450840048383));
#70440=CARTESIAN_POINT('',(0.599999999999999,-5.62260472388598,-4.44918151112483));
#70441=CARTESIAN_POINT('Origin',(0.600000000000001,0.,0.));
#70442=CARTESIAN_POINT('',(0.6,-5.30102754638333,-4.44809025903085));
#70443=CARTESIAN_POINT('Origin',(0.6,-5.30102754638333,-4.44809025903085));
#70444=CARTESIAN_POINT('',(17.4,-5.62260472388598,-4.44918151112483));
#70445=CARTESIAN_POINT('',(9.,-5.62260472388598,-4.44918151112483));
#70446=CARTESIAN_POINT('',(17.4,-5.30102754638333,-4.44809025903085));
#70447=CARTESIAN_POINT('Origin',(17.4,-5.41593421285118,-4.54450840048383));
#70448=CARTESIAN_POINT('Origin',(17.4,0.,0.));
#70449=CARTESIAN_POINT('Origin',(0.6,-6.12770341532365,-3.82650635094611));
#70450=CARTESIAN_POINT('',(17.4,-6.10390710806817,-3.76181047051481));
#70451=CARTESIAN_POINT('',(0.599999999999999,-6.10390710806817,-3.76181047051481));
#70452=CARTESIAN_POINT('',(9.,-6.10390710806817,-3.76181047051481));
#70453=CARTESIAN_POINT('',(17.4,-5.99289579418832,-3.46));
#70454=CARTESIAN_POINT('',(17.4,-6.12770341532365,-3.82650635094611));
#70455=CARTESIAN_POINT('',(0.6,-5.99289579418832,-3.46));
#70456=CARTESIAN_POINT('',(0.6,-5.99289579418832,-3.46));
#70457=CARTESIAN_POINT('',(0.6,-6.12770341532365,-3.82650635094611));
#70458=CARTESIAN_POINT('Origin',(0.6,-6.12279960475598,-3.535));
#70459=CARTESIAN_POINT('',(0.600000000000001,-6.30977698572221,-3.40523338267003));
#70460=CARTESIAN_POINT('Origin',(0.600000000000001,0.,0.));
#70461=CARTESIAN_POINT('',(0.6,-5.99289579418832,-3.46));
#70462=CARTESIAN_POINT('Origin',(0.6,-5.99289579418832,-3.46));
#70463=CARTESIAN_POINT('',(17.4,-6.30977698572221,-3.40523338267003));
#70464=CARTESIAN_POINT('',(9.,-6.30977698572221,-3.40523338267003));
#70465=CARTESIAN_POINT('',(17.4,-5.99289579418832,-3.46));
#70466=CARTESIAN_POINT('Origin',(17.4,-6.12279960475598,-3.535));
#70467=CARTESIAN_POINT('Origin',(17.4,0.,0.));
#70468=CARTESIAN_POINT('Origin',(0.6,-6.69907568624284,-2.7043085900078));
#70469=CARTESIAN_POINT('',(17.4,-6.66440657662513,-2.64472777076123));
#70470=CARTESIAN_POINT('',(0.600000000000001,-6.66440657662513,-2.64472777076123));
#70471=CARTESIAN_POINT('',(9.,-6.66440657662513,-2.64472777076123));
#70472=CARTESIAN_POINT('',(17.4,-6.50267293583849,-2.36677939181363));
#70473=CARTESIAN_POINT('',(17.4,-6.69907568624284,-2.7043085900078));
#70474=CARTESIAN_POINT('',(0.6,-6.50267293583849,-2.36677939181363));
#70475=CARTESIAN_POINT('',(0.6,-6.50267293583849,-2.36677939181363));
#70476=CARTESIAN_POINT('',(0.6,-6.69907568624284,-2.7043085900078));
#70477=CARTESIAN_POINT('Origin',(0.6,-6.64362682895637,-2.41808241331248));
#70478=CARTESIAN_POINT('',(0.599999999999999,-6.80522986674848,-2.25781896101403));
#70479=CARTESIAN_POINT('Origin',(0.600000000000001,0.,0.));
#70480=CARTESIAN_POINT('',(0.6,-6.50267293583849,-2.36677939181363));
#70481=CARTESIAN_POINT('Origin',(0.6,-6.50267293583849,-2.36677939181363));
#70482=CARTESIAN_POINT('',(17.4,-6.80522986674848,-2.25781896101403));
#70483=CARTESIAN_POINT('',(9.,-6.80522986674848,-2.25781896101403));
#70484=CARTESIAN_POINT('',(17.4,-6.50267293583849,-2.36677939181363));
#70485=CARTESIAN_POINT('Origin',(17.4,-6.64362682895637,-2.41808241331248));
#70486=CARTESIAN_POINT('Origin',(17.4,0.,0.));
#70487=CARTESIAN_POINT('Origin',(0.6,-7.06689993233141,-1.49994178100829));
#70488=CARTESIAN_POINT('',(17.4,-7.02241142370379,-1.44728635598989));
#70489=CARTESIAN_POINT('',(0.600000000000001,-7.02241142370379,-1.44728635598989));
#70490=CARTESIAN_POINT('',(9.,-7.02241142370379,-1.44728635598989));
#70491=CARTESIAN_POINT('',(17.4,-6.81486965084448,-1.20164538945516));
#70492=CARTESIAN_POINT('',(17.4,-7.06689993233141,-1.49994178100829));
#70493=CARTESIAN_POINT('',(0.6,-6.81486965084448,-1.20164538945516));
#70494=CARTESIAN_POINT('',(0.6,-6.81486965084448,-1.20164538945516));
#70495=CARTESIAN_POINT('',(0.6,-7.06689993233141,-1.49994178100829));
#70496=CARTESIAN_POINT('Origin',(0.6,-6.96259081379631,-1.2276926161052));
#70497=CARTESIAN_POINT('',(0.599999999999999,-7.09390928188607,-1.04180185273915));
#70498=CARTESIAN_POINT('Origin',(0.600000000000001,0.,0.));
#70499=CARTESIAN_POINT('',(0.6,-6.81486965084448,-1.20164538945516));
#70500=CARTESIAN_POINT('Origin',(0.6,-6.81486965084448,-1.20164538945516));
#70501=CARTESIAN_POINT('',(17.4,-7.09390928188607,-1.04180185273915));
#70502=CARTESIAN_POINT('',(9.,-7.09390928188607,-1.04180185273915));
#70503=CARTESIAN_POINT('',(17.4,-6.81486965084448,-1.20164538945516));
#70504=CARTESIAN_POINT('Origin',(17.4,-6.96259081379631,-1.2276926161052));
#70505=CARTESIAN_POINT('Origin',(17.4,0.,0.));
#70506=CARTESIAN_POINT('Origin',(0.6,-7.22,-0.249999999999999));
#70507=CARTESIAN_POINT('',(17.4,-7.16704385318485,-0.205869877654039));
#70508=CARTESIAN_POINT('',(0.599999999999999,-7.16704385318485,-0.205869877654039));
#70509=CARTESIAN_POINT('',(9.,-7.16704385318485,-0.205869877654039));
#70510=CARTESIAN_POINT('',(17.4,-6.92,8.47455585009968E-16));
#70511=CARTESIAN_POINT('',(17.4,-7.22,-0.249999999999999));
#70512=CARTESIAN_POINT('',(0.6,-6.92,8.47455585009968E-16));
#70513=CARTESIAN_POINT('',(0.6,-6.92,8.47455585009968E-16));
#70514=CARTESIAN_POINT('',(0.6,-7.22,-0.249999999999999));
#70515=CARTESIAN_POINT('Origin',(0.6,-7.07,8.65825286997179E-16));
#70516=CARTESIAN_POINT('',(0.600000000000001,-7.17,-8.78071754988652E-16));
#70517=CARTESIAN_POINT('Origin',(0.600000000000001,0.,0.));
#70518=CARTESIAN_POINT('',(0.600000000000001,-7.16704385318485,0.20586987765404));
#70519=CARTESIAN_POINT('',(0.6,-6.92,8.47455585009968E-16));
#70520=CARTESIAN_POINT('Origin',(0.600000000000001,0.,0.));
#70521=CARTESIAN_POINT('Origin',(0.6,-6.92,8.47455585009968E-16));
#70522=CARTESIAN_POINT('',(17.4,-7.16704385318485,0.20586987765404));
#70523=CARTESIAN_POINT('',(9.,-7.16704385318485,0.20586987765404));
#70524=CARTESIAN_POINT('',(17.4,-6.92,8.47455585009968E-16));
#70525=CARTESIAN_POINT('Origin',(17.4,-7.07,8.65825286997179E-16));
#70526=CARTESIAN_POINT('',(17.4,-7.17,-8.78071754988652E-16));
#70527=CARTESIAN_POINT('Origin',(17.4,0.,0.));
#70528=CARTESIAN_POINT('Origin',(17.4,0.,0.));
#70529=CARTESIAN_POINT('Origin',(0.6,-7.15372402116487,1.00753790450219));
#70530=CARTESIAN_POINT('',(17.4,-7.09390928188606,1.04180185273915));
#70531=CARTESIAN_POINT('',(0.599999999999999,-7.09390928188606,1.04180185273915));
#70532=CARTESIAN_POINT('',(9.,-7.09390928188606,1.04180185273915));
#70533=CARTESIAN_POINT('',(17.4,-6.81486965084448,1.20164538945516));
#70534=CARTESIAN_POINT('',(17.4,-7.15372402116487,1.00753790450219));
#70535=CARTESIAN_POINT('',(0.6,-6.81486965084448,1.20164538945516));
#70536=CARTESIAN_POINT('',(0.6,-6.81486965084448,1.20164538945516));
#70537=CARTESIAN_POINT('',(0.6,-7.15372402116487,1.00753790450219));
#70538=CARTESIAN_POINT('Origin',(0.6,-6.96259081379631,1.2276926161052));
#70539=CARTESIAN_POINT('',(0.600000000000001,-7.02241142370379,1.4472863559899));
#70540=CARTESIAN_POINT('Origin',(0.600000000000001,0.,0.));
#70541=CARTESIAN_POINT('',(0.6,-6.81486965084448,1.20164538945516));
#70542=CARTESIAN_POINT('Origin',(0.6,-6.81486965084448,1.20164538945516));
#70543=CARTESIAN_POINT('',(17.4,-7.02241142370379,1.4472863559899));
#70544=CARTESIAN_POINT('',(9.,-7.02241142370379,1.4472863559899));
#70545=CARTESIAN_POINT('',(17.4,-6.81486965084448,1.20164538945516));
#70546=CARTESIAN_POINT('Origin',(17.4,-6.96259081379631,1.2276926161052));
#70547=CARTESIAN_POINT('Origin',(17.4,0.,0.));
#70548=CARTESIAN_POINT('Origin',(0.6,-6.87008575790568,2.23446227961485));
#70549=CARTESIAN_POINT('',(17.4,-6.80522986674848,2.25781896101404));
#70550=CARTESIAN_POINT('',(0.599999999999999,-6.80522986674848,2.25781896101404));
#70551=CARTESIAN_POINT('',(9.,-6.80522986674848,2.25781896101404));
#70552=CARTESIAN_POINT('',(17.4,-6.50267293583849,2.36677939181363));
#70553=CARTESIAN_POINT('',(17.4,-6.87008575790568,2.23446227961485));
#70554=CARTESIAN_POINT('',(0.6,-6.50267293583849,2.36677939181363));
#70555=CARTESIAN_POINT('',(0.6,-6.50267293583849,2.36677939181363));
#70556=CARTESIAN_POINT('',(0.6,-6.87008575790568,2.23446227961485));
#70557=CARTESIAN_POINT('Origin',(0.6,-6.64362682895637,2.41808241331248));
#70558=CARTESIAN_POINT('',(0.600000000000001,-6.66440657662513,2.64472777076123));
#70559=CARTESIAN_POINT('Origin',(0.600000000000001,0.,0.));
#70560=CARTESIAN_POINT('',(0.6,-6.50267293583849,2.36677939181363));
#70561=CARTESIAN_POINT('Origin',(0.6,-6.50267293583849,2.36677939181363));
#70562=CARTESIAN_POINT('',(17.4,-6.66440657662513,2.64472777076123));
#70563=CARTESIAN_POINT('',(9.,-6.66440657662513,2.64472777076123));
#70564=CARTESIAN_POINT('',(17.4,-6.50267293583849,2.36677939181363));
#70565=CARTESIAN_POINT('Origin',(17.4,-6.64362682895637,2.41808241331248));
#70566=CARTESIAN_POINT('Origin',(17.4,0.,0.));
#70567=CARTESIAN_POINT('Origin',(0.6,-6.37770341532365,3.39349364905389));
#70568=CARTESIAN_POINT('',(17.4,-6.30977698572221,3.40523338267003));
#70569=CARTESIAN_POINT('',(0.600000000000001,-6.30977698572221,3.40523338267003));
#70570=CARTESIAN_POINT('',(9.,-6.30977698572221,3.40523338267003));
#70571=CARTESIAN_POINT('',(17.4,-5.99289579418832,3.46));
#70572=CARTESIAN_POINT('',(17.4,-6.37770341532365,3.39349364905389));
#70573=CARTESIAN_POINT('',(0.6,-5.99289579418832,3.46));
#70574=CARTESIAN_POINT('',(0.6,-5.99289579418832,3.46));
#70575=CARTESIAN_POINT('',(0.6,-6.37770341532365,3.39349364905389));
#70576=CARTESIAN_POINT('Origin',(0.6,-6.12279960475598,3.535));
#70577=CARTESIAN_POINT('',(0.600000000000001,-6.10390710806817,3.76181047051481));
#70578=CARTESIAN_POINT('Origin',(0.600000000000001,0.,0.));
#70579=CARTESIAN_POINT('',(0.6,-5.99289579418832,3.46));
#70580=CARTESIAN_POINT('Origin',(0.6,-5.99289579418832,3.46));
#70581=CARTESIAN_POINT('',(17.4,-6.10390710806817,3.76181047051481));
#70582=CARTESIAN_POINT('',(9.,-6.10390710806817,3.76181047051481));
#70583=CARTESIAN_POINT('',(17.4,-5.99289579418832,3.46));
#70584=CARTESIAN_POINT('Origin',(17.4,-6.12279960475598,3.535));
#70585=CARTESIAN_POINT('Origin',(17.4,0.,0.));
#70586=CARTESIAN_POINT('Origin',(0.6,-5.69153778174066,4.44941543115707));
#70587=CARTESIAN_POINT('',(17.4,-5.62260472388598,4.44918151112483));
#70588=CARTESIAN_POINT('',(0.599999999999999,-5.62260472388598,4.44918151112483));
#70589=CARTESIAN_POINT('',(9.,-5.62260472388598,4.44918151112483));
#70590=CARTESIAN_POINT('',(17.4,-5.30102754638333,4.44809025903085));
#70591=CARTESIAN_POINT('',(17.4,-5.69153778174066,4.44941543115707));
#70592=CARTESIAN_POINT('',(0.6,-5.30102754638333,4.44809025903085));
#70593=CARTESIAN_POINT('',(0.6,-5.30102754638333,4.44809025903085));
#70594=CARTESIAN_POINT('',(0.6,-5.69153778174066,4.44941543115707));
#70595=CARTESIAN_POINT('Origin',(0.6,-5.41593421285117,4.54450840048383));
#70596=CARTESIAN_POINT('',(0.599999999999999,-5.35794351075858,4.76459246268976));
#70597=CARTESIAN_POINT('Origin',(0.600000000000001,0.,0.));
#70598=CARTESIAN_POINT('',(0.6,-5.30102754638333,4.44809025903085));
#70599=CARTESIAN_POINT('Origin',(0.6,-5.30102754638333,4.44809025903085));
#70600=CARTESIAN_POINT('',(17.4,-5.35794351075858,4.76459246268976));
#70601=CARTESIAN_POINT('',(9.,-5.35794351075858,4.76459246268976));
#70602=CARTESIAN_POINT('',(17.4,-5.30102754638333,4.44809025903085));
#70603=CARTESIAN_POINT('Origin',(17.4,-5.41593421285117,4.54450840048383));
#70604=CARTESIAN_POINT('Origin',(17.4,0.,0.));
#70605=CARTESIAN_POINT('Origin',(0.6,-4.83243765271656,5.37014397689739));
#70606=CARTESIAN_POINT('',(17.4,-4.76459246268975,5.35794351075858));
#70607=CARTESIAN_POINT('',(0.599999999999999,-4.76459246268975,5.35794351075858));
#70608=CARTESIAN_POINT('',(9.,-4.76459246268975,5.35794351075858));
#70609=CARTESIAN_POINT('',(17.4,-4.44809025903085,5.30102754638333));
#70610=CARTESIAN_POINT('',(17.4,-4.83243765271656,5.37014397689739));
#70611=CARTESIAN_POINT('',(0.6,-4.44809025903085,5.30102754638333));
#70612=CARTESIAN_POINT('',(0.6,-4.44809025903085,5.30102754638333));
#70613=CARTESIAN_POINT('',(0.6,-4.83243765271656,5.37014397689739));
#70614=CARTESIAN_POINT('Origin',(0.6,-4.54450840048383,5.41593421285117));
#70615=CARTESIAN_POINT('',(0.599999999999999,-4.44918151112483,5.62260472388598));
#70616=CARTESIAN_POINT('Origin',(0.600000000000001,0.,0.));
#70617=CARTESIAN_POINT('',(0.6,-4.44809025903085,5.30102754638333));
#70618=CARTESIAN_POINT('Origin',(0.6,-4.44809025903085,5.30102754638333));
#70619=CARTESIAN_POINT('',(17.4,-4.44918151112483,5.62260472388598));
#70620=CARTESIAN_POINT('',(9.,-4.44918151112483,5.62260472388598));
#70621=CARTESIAN_POINT('',(17.4,-4.44809025903085,5.30102754638333));
#70622=CARTESIAN_POINT('Origin',(17.4,-4.54450840048383,5.41593421285117));
#70623=CARTESIAN_POINT('Origin',(17.4,0.,0.));
#70624=CARTESIAN_POINT('Origin',(0.6,-3.82650635094611,6.12770341532365));
#70625=CARTESIAN_POINT('',(17.4,-3.76181047051481,6.10390710806817));
#70626=CARTESIAN_POINT('',(0.600000000000001,-3.76181047051481,6.10390710806817));
#70627=CARTESIAN_POINT('',(9.,-3.76181047051481,6.10390710806817));
#70628=CARTESIAN_POINT('',(17.4,-3.46,5.99289579418832));
#70629=CARTESIAN_POINT('',(17.4,-3.82650635094611,6.12770341532365));
#70630=CARTESIAN_POINT('',(0.6,-3.46,5.99289579418832));
#70631=CARTESIAN_POINT('',(0.6,-3.46,5.99289579418832));
#70632=CARTESIAN_POINT('',(0.6,-3.82650635094611,6.12770341532365));
#70633=CARTESIAN_POINT('Origin',(0.6,-3.535,6.12279960475598));
#70634=CARTESIAN_POINT('',(0.599999999999999,-3.40523338267003,6.30977698572221));
#70635=CARTESIAN_POINT('Origin',(0.600000000000001,0.,0.));
#70636=CARTESIAN_POINT('',(0.6,-3.46,5.99289579418832));
#70637=CARTESIAN_POINT('Origin',(0.6,-3.46,5.99289579418832));
#70638=CARTESIAN_POINT('',(17.4,-3.40523338267003,6.30977698572221));
#70639=CARTESIAN_POINT('',(9.,-3.40523338267003,6.30977698572221));
#70640=CARTESIAN_POINT('',(17.4,-3.46,5.99289579418832));
#70641=CARTESIAN_POINT('Origin',(17.4,-3.535,6.12279960475598));
#70642=CARTESIAN_POINT('Origin',(17.4,0.,0.));
#70643=CARTESIAN_POINT('Origin',(0.6,-2.7043085900078,6.69907568624284));
#70644=CARTESIAN_POINT('',(17.4,-2.64472777076123,6.66440657662513));
#70645=CARTESIAN_POINT('',(0.599999999999999,-2.64472777076123,6.66440657662513));
#70646=CARTESIAN_POINT('',(9.,-2.64472777076123,6.66440657662513));
#70647=CARTESIAN_POINT('',(17.4,-2.36677939181363,6.50267293583849));
#70648=CARTESIAN_POINT('',(17.4,-2.7043085900078,6.69907568624284));
#70649=CARTESIAN_POINT('',(0.6,-2.36677939181363,6.50267293583849));
#70650=CARTESIAN_POINT('',(0.6,-2.36677939181363,6.50267293583849));
#70651=CARTESIAN_POINT('',(0.6,-2.7043085900078,6.69907568624284));
#70652=CARTESIAN_POINT('Origin',(0.6,-2.41808241331248,6.64362682895637));
#70653=CARTESIAN_POINT('',(0.599999999999999,-2.25781896101403,6.80522986674848));
#70654=CARTESIAN_POINT('Origin',(0.600000000000001,0.,0.));
#70655=CARTESIAN_POINT('',(0.6,-2.36677939181363,6.50267293583849));
#70656=CARTESIAN_POINT('Origin',(0.6,-2.36677939181363,6.50267293583849));
#70657=CARTESIAN_POINT('',(17.4,-2.25781896101403,6.80522986674848));
#70658=CARTESIAN_POINT('',(9.,-2.25781896101403,6.80522986674848));
#70659=CARTESIAN_POINT('',(17.4,-2.36677939181363,6.50267293583849));
#70660=CARTESIAN_POINT('Origin',(17.4,-2.41808241331248,6.64362682895637));
#70661=CARTESIAN_POINT('Origin',(17.4,0.,0.));
#70662=CARTESIAN_POINT('Origin',(0.6,-1.49994178100829,7.06689993233141));
#70663=CARTESIAN_POINT('',(17.4,-1.4472863559899,7.02241142370379));
#70664=CARTESIAN_POINT('',(0.600000000000001,-1.4472863559899,7.02241142370379));
#70665=CARTESIAN_POINT('',(9.,-1.4472863559899,7.02241142370379));
#70666=CARTESIAN_POINT('',(17.4,-1.20164538945516,6.81486965084448));
#70667=CARTESIAN_POINT('',(17.4,-1.49994178100829,7.06689993233141));
#70668=CARTESIAN_POINT('',(0.6,-1.20164538945516,6.81486965084448));
#70669=CARTESIAN_POINT('',(0.6,-1.20164538945516,6.81486965084448));
#70670=CARTESIAN_POINT('',(0.6,-1.49994178100829,7.06689993233141));
#70671=CARTESIAN_POINT('Origin',(0.6,-1.2276926161052,6.96259081379631));
#70672=CARTESIAN_POINT('',(0.600000000000001,-1.04180185273915,7.09390928188606));
#70673=CARTESIAN_POINT('Origin',(0.600000000000001,0.,0.));
#70674=CARTESIAN_POINT('',(0.6,-1.20164538945516,6.81486965084448));
#70675=CARTESIAN_POINT('Origin',(0.6,-1.20164538945516,6.81486965084448));
#70676=CARTESIAN_POINT('',(17.4,-1.04180185273915,7.09390928188606));
#70677=CARTESIAN_POINT('',(9.,-1.04180185273915,7.09390928188606));
#70678=CARTESIAN_POINT('',(17.4,-1.20164538945516,6.81486965084448));
#70679=CARTESIAN_POINT('Origin',(17.4,-1.2276926161052,6.96259081379631));
#70680=CARTESIAN_POINT('Origin',(17.4,0.,0.));
#70681=CARTESIAN_POINT('Origin',(0.6,-0.25,7.22));
#70682=CARTESIAN_POINT('',(17.4,-0.20586987765404,7.16704385318485));
#70683=CARTESIAN_POINT('',(0.600000000000001,-0.20586987765404,7.16704385318485));
#70684=CARTESIAN_POINT('',(9.,-0.20586987765404,7.16704385318485));
#70685=CARTESIAN_POINT('',(17.4,4.23727792504984E-16,6.92));
#70686=CARTESIAN_POINT('',(17.4,-0.25,7.22));
#70687=CARTESIAN_POINT('',(0.6,4.23727792504984E-16,6.92));
#70688=CARTESIAN_POINT('',(0.6,4.23727792504984E-16,6.92));
#70689=CARTESIAN_POINT('',(0.6,-0.25,7.22));
#70690=CARTESIAN_POINT('Origin',(0.6,4.32912643498589E-16,7.07));
#70691=CARTESIAN_POINT('',(0.600000000000001,0.20586987765404,7.16704385318485));
#70692=CARTESIAN_POINT('Origin',(0.600000000000001,0.,0.));
#70693=CARTESIAN_POINT('',(0.6,4.23727792504984E-16,6.92));
#70694=CARTESIAN_POINT('Origin',(0.6,4.23727792504984E-16,6.92));
#70695=CARTESIAN_POINT('',(17.4,0.20586987765404,7.16704385318485));
#70696=CARTESIAN_POINT('',(9.,0.205869877654041,7.16704385318485));
#70697=CARTESIAN_POINT('',(17.4,4.23727792504984E-16,6.92));
#70698=CARTESIAN_POINT('Origin',(17.4,4.32912643498589E-16,7.07));
#70699=CARTESIAN_POINT('Origin',(17.4,0.,0.));
#70700=CARTESIAN_POINT('Origin',(0.6,1.00753790450219,7.15372402116488));
#70701=CARTESIAN_POINT('',(17.4,1.04180185273915,7.09390928188606));
#70702=CARTESIAN_POINT('',(0.600000000000001,1.04180185273915,7.09390928188606));
#70703=CARTESIAN_POINT('',(9.,1.04180185273915,7.09390928188606));
#70704=CARTESIAN_POINT('',(17.4,1.20164538945516,6.81486965084448));
#70705=CARTESIAN_POINT('',(17.4,1.00753790450219,7.15372402116488));
#70706=CARTESIAN_POINT('',(0.6,1.20164538945516,6.81486965084448));
#70707=CARTESIAN_POINT('',(0.6,1.20164538945516,6.81486965084448));
#70708=CARTESIAN_POINT('',(0.6,1.00753790450219,7.15372402116488));
#70709=CARTESIAN_POINT('Origin',(0.6,1.2276926161052,6.96259081379631));
#70710=CARTESIAN_POINT('',(0.600000000000001,1.4472863559899,7.02241142370379));
#70711=CARTESIAN_POINT('Origin',(0.600000000000001,0.,0.));
#70712=CARTESIAN_POINT('',(0.6,1.20164538945516,6.81486965084448));
#70713=CARTESIAN_POINT('Origin',(0.6,1.20164538945516,6.81486965084448));
#70714=CARTESIAN_POINT('',(17.4,1.4472863559899,7.02241142370379));
#70715=CARTESIAN_POINT('',(9.,1.4472863559899,7.02241142370379));
#70716=CARTESIAN_POINT('',(17.4,1.20164538945516,6.81486965084448));
#70717=CARTESIAN_POINT('Origin',(17.4,1.2276926161052,6.96259081379631));
#70718=CARTESIAN_POINT('Origin',(17.4,0.,0.));
#70719=CARTESIAN_POINT('Origin',(0.6,2.23446227961485,6.87008575790568));
#70720=CARTESIAN_POINT('',(17.4,2.25781896101404,6.80522986674848));
#70721=CARTESIAN_POINT('',(0.600000000000001,2.25781896101404,6.80522986674848));
#70722=CARTESIAN_POINT('',(9.,2.25781896101404,6.80522986674848));
#70723=CARTESIAN_POINT('',(17.4,2.36677939181363,6.50267293583849));
#70724=CARTESIAN_POINT('',(17.4,2.23446227961485,6.87008575790568));
#70725=CARTESIAN_POINT('',(0.6,2.36677939181363,6.50267293583849));
#70726=CARTESIAN_POINT('',(0.6,2.36677939181363,6.50267293583849));
#70727=CARTESIAN_POINT('',(0.6,2.23446227961485,6.87008575790568));
#70728=CARTESIAN_POINT('Origin',(0.6,2.41808241331248,6.64362682895637));
#70729=CARTESIAN_POINT('',(0.600000000000001,2.64472777076123,6.66440657662513));
#70730=CARTESIAN_POINT('Origin',(0.600000000000001,0.,0.));
#70731=CARTESIAN_POINT('',(0.6,2.36677939181363,6.50267293583849));
#70732=CARTESIAN_POINT('Origin',(0.6,2.36677939181363,6.50267293583849));
#70733=CARTESIAN_POINT('',(17.4,2.64472777076123,6.66440657662513));
#70734=CARTESIAN_POINT('',(9.,2.64472777076123,6.66440657662513));
#70735=CARTESIAN_POINT('',(17.4,2.36677939181363,6.50267293583849));
#70736=CARTESIAN_POINT('Origin',(17.4,2.41808241331248,6.64362682895637));
#70737=CARTESIAN_POINT('Origin',(17.4,0.,0.));
#70738=CARTESIAN_POINT('Origin',(0.6,3.39349364905389,6.37770341532365));
#70739=CARTESIAN_POINT('',(17.4,3.40523338267003,6.30977698572221));
#70740=CARTESIAN_POINT('',(0.599999999999999,3.40523338267003,6.30977698572221));
#70741=CARTESIAN_POINT('',(9.,3.40523338267003,6.30977698572221));
#70742=CARTESIAN_POINT('',(17.4,3.46,5.99289579418831));
#70743=CARTESIAN_POINT('',(17.4,3.39349364905389,6.37770341532365));
#70744=CARTESIAN_POINT('',(0.6,3.46,5.99289579418831));
#70745=CARTESIAN_POINT('',(0.6,3.46,5.99289579418831));
#70746=CARTESIAN_POINT('',(0.6,3.39349364905389,6.37770341532365));
#70747=CARTESIAN_POINT('Origin',(0.6,3.535,6.12279960475598));
#70748=CARTESIAN_POINT('',(0.599999999999999,3.76181047051482,6.10390710806817));
#70749=CARTESIAN_POINT('Origin',(0.600000000000001,0.,0.));
#70750=CARTESIAN_POINT('',(0.6,3.46,5.99289579418831));
#70751=CARTESIAN_POINT('Origin',(0.6,3.46,5.99289579418831));
#70752=CARTESIAN_POINT('',(17.4,3.76181047051482,6.10390710806817));
#70753=CARTESIAN_POINT('',(9.,3.76181047051482,6.10390710806817));
#70754=CARTESIAN_POINT('',(17.4,3.46,5.99289579418831));
#70755=CARTESIAN_POINT('Origin',(17.4,3.535,6.12279960475598));
#70756=CARTESIAN_POINT('Origin',(17.4,0.,0.));
#70757=CARTESIAN_POINT('Origin',(0.6,4.44941543115707,5.69153778174066));
#70758=CARTESIAN_POINT('',(17.4,4.44918151112483,5.62260472388598));
#70759=CARTESIAN_POINT('',(0.599999999999999,4.44918151112483,5.62260472388598));
#70760=CARTESIAN_POINT('',(9.,4.44918151112483,5.62260472388598));
#70761=CARTESIAN_POINT('',(17.4,4.44809025903085,5.30102754638333));
#70762=CARTESIAN_POINT('',(17.4,4.44941543115707,5.69153778174066));
#70763=CARTESIAN_POINT('',(0.6,4.44809025903085,5.30102754638333));
#70764=CARTESIAN_POINT('',(0.6,4.44809025903085,5.30102754638333));
#70765=CARTESIAN_POINT('',(0.6,4.44941543115707,5.69153778174066));
#70766=CARTESIAN_POINT('Origin',(0.6,4.54450840048383,5.41593421285117));
#70767=CARTESIAN_POINT('',(0.599999999999999,4.76459246268975,5.35794351075858));
#70768=CARTESIAN_POINT('Origin',(0.600000000000001,0.,0.));
#70769=CARTESIAN_POINT('',(0.6,4.44809025903085,5.30102754638333));
#70770=CARTESIAN_POINT('Origin',(0.6,4.44809025903085,5.30102754638333));
#70771=CARTESIAN_POINT('',(17.4,4.76459246268975,5.35794351075858));
#70772=CARTESIAN_POINT('',(9.,4.76459246268975,5.35794351075858));
#70773=CARTESIAN_POINT('',(17.4,4.44809025903085,5.30102754638333));
#70774=CARTESIAN_POINT('Origin',(17.4,4.54450840048383,5.41593421285117));
#70775=CARTESIAN_POINT('Origin',(17.4,0.,0.));
#70776=CARTESIAN_POINT('Origin',(0.6,5.37014397689739,4.83243765271656));
#70777=CARTESIAN_POINT('',(17.4,5.35794351075858,4.76459246268975));
#70778=CARTESIAN_POINT('',(0.599999999999999,5.35794351075858,4.76459246268975));
#70779=CARTESIAN_POINT('',(9.,5.35794351075858,4.76459246268975));
#70780=CARTESIAN_POINT('',(17.4,5.30102754638333,4.44809025903085));
#70781=CARTESIAN_POINT('',(17.4,5.37014397689739,4.83243765271656));
#70782=CARTESIAN_POINT('',(0.6,5.30102754638333,4.44809025903085));
#70783=CARTESIAN_POINT('',(0.6,5.30102754638333,4.44809025903085));
#70784=CARTESIAN_POINT('',(0.6,5.37014397689739,4.83243765271656));
#70785=CARTESIAN_POINT('Origin',(0.6,5.41593421285118,4.54450840048383));
#70786=CARTESIAN_POINT('',(0.599999999999999,5.62260472388598,4.44918151112483));
#70787=CARTESIAN_POINT('Origin',(0.600000000000001,0.,0.));
#70788=CARTESIAN_POINT('',(0.6,5.30102754638333,4.44809025903085));
#70789=CARTESIAN_POINT('Origin',(0.6,5.30102754638333,4.44809025903085));
#70790=CARTESIAN_POINT('',(17.4,5.62260472388598,4.44918151112483));
#70791=CARTESIAN_POINT('',(9.,5.62260472388598,4.44918151112483));
#70792=CARTESIAN_POINT('',(17.4,5.30102754638333,4.44809025903085));
#70793=CARTESIAN_POINT('Origin',(17.4,5.41593421285118,4.54450840048383));
#70794=CARTESIAN_POINT('Origin',(17.4,0.,0.));
#70795=CARTESIAN_POINT('Origin',(0.6,6.12770341532365,3.82650635094611));
#70796=CARTESIAN_POINT('',(17.4,6.10390710806817,3.76181047051481));
#70797=CARTESIAN_POINT('',(0.600000000000001,6.10390710806817,3.76181047051481));
#70798=CARTESIAN_POINT('',(9.,6.10390710806817,3.76181047051481));
#70799=CARTESIAN_POINT('',(17.4,5.99289579418832,3.46));
#70800=CARTESIAN_POINT('',(17.4,6.12770341532365,3.82650635094611));
#70801=CARTESIAN_POINT('',(0.6,5.99289579418832,3.46));
#70802=CARTESIAN_POINT('',(0.6,5.99289579418832,3.46));
#70803=CARTESIAN_POINT('',(0.6,6.12770341532365,3.82650635094611));
#70804=CARTESIAN_POINT('Origin',(0.6,6.12279960475598,3.535));
#70805=CARTESIAN_POINT('',(0.600000000000001,6.30977698572221,3.40523338267003));
#70806=CARTESIAN_POINT('Origin',(0.600000000000001,0.,0.));
#70807=CARTESIAN_POINT('',(0.6,5.99289579418832,3.46));
#70808=CARTESIAN_POINT('Origin',(0.6,5.99289579418832,3.46));
#70809=CARTESIAN_POINT('',(17.4,6.30977698572221,3.40523338267003));
#70810=CARTESIAN_POINT('',(9.,6.30977698572221,3.40523338267003));
#70811=CARTESIAN_POINT('',(17.4,5.99289579418832,3.46));
#70812=CARTESIAN_POINT('Origin',(17.4,6.12279960475598,3.535));
#70813=CARTESIAN_POINT('Origin',(17.4,0.,0.));
#70814=CARTESIAN_POINT('Origin',(0.6,6.69907568624284,2.7043085900078));
#70815=CARTESIAN_POINT('',(17.4,6.66440657662513,2.64472777076123));
#70816=CARTESIAN_POINT('',(0.599999999999999,6.66440657662513,2.64472777076123));
#70817=CARTESIAN_POINT('',(9.,6.66440657662513,2.64472777076123));
#70818=CARTESIAN_POINT('',(17.4,6.50267293583849,2.36677939181363));
#70819=CARTESIAN_POINT('',(17.4,6.69907568624284,2.7043085900078));
#70820=CARTESIAN_POINT('',(0.6,6.50267293583849,2.36677939181363));
#70821=CARTESIAN_POINT('',(0.6,6.50267293583849,2.36677939181363));
#70822=CARTESIAN_POINT('',(0.6,6.69907568624284,2.7043085900078));
#70823=CARTESIAN_POINT('Origin',(0.6,6.64362682895637,2.41808241331248));
#70824=CARTESIAN_POINT('',(0.599999999999999,6.80522986674848,2.25781896101403));
#70825=CARTESIAN_POINT('Origin',(0.600000000000001,0.,0.));
#70826=CARTESIAN_POINT('',(0.6,6.50267293583849,2.36677939181363));
#70827=CARTESIAN_POINT('Origin',(0.6,6.50267293583849,2.36677939181363));
#70828=CARTESIAN_POINT('',(17.4,6.80522986674848,2.25781896101403));
#70829=CARTESIAN_POINT('',(9.,6.80522986674848,2.25781896101403));
#70830=CARTESIAN_POINT('',(17.4,6.50267293583849,2.36677939181363));
#70831=CARTESIAN_POINT('Origin',(17.4,6.64362682895637,2.41808241331248));
#70832=CARTESIAN_POINT('Origin',(17.4,0.,0.));
#70833=CARTESIAN_POINT('Origin',(0.6,7.06689993233141,1.49994178100829));
#70834=CARTESIAN_POINT('',(17.4,7.02241142370379,1.4472863559899));
#70835=CARTESIAN_POINT('',(0.600000000000001,7.02241142370379,1.4472863559899));
#70836=CARTESIAN_POINT('',(9.,7.02241142370379,1.4472863559899));
#70837=CARTESIAN_POINT('',(17.4,6.81486965084448,1.20164538945516));
#70838=CARTESIAN_POINT('',(17.4,7.06689993233141,1.49994178100829));
#70839=CARTESIAN_POINT('',(0.6,6.81486965084448,1.20164538945516));
#70840=CARTESIAN_POINT('',(0.6,6.81486965084448,1.20164538945516));
#70841=CARTESIAN_POINT('',(0.6,7.06689993233141,1.49994178100829));
#70842=CARTESIAN_POINT('Origin',(0.6,6.96259081379631,1.2276926161052));
#70843=CARTESIAN_POINT('',(0.600000000000001,7.09390928188606,1.04180185273915));
#70844=CARTESIAN_POINT('Origin',(0.600000000000001,0.,0.));
#70845=CARTESIAN_POINT('',(0.6,6.81486965084448,1.20164538945516));
#70846=CARTESIAN_POINT('Origin',(0.6,6.81486965084448,1.20164538945516));
#70847=CARTESIAN_POINT('',(17.4,7.09390928188606,1.04180185273915));
#70848=CARTESIAN_POINT('',(9.,7.09390928188606,1.04180185273915));
#70849=CARTESIAN_POINT('',(17.4,6.81486965084448,1.20164538945516));
#70850=CARTESIAN_POINT('Origin',(17.4,6.96259081379631,1.2276926161052));
#70851=CARTESIAN_POINT('Origin',(17.4,0.,0.));
#70852=CARTESIAN_POINT('Origin',(0.6,7.22,0.25));
#70853=CARTESIAN_POINT('',(17.4,7.16704385318485,0.20586987765404));
#70854=CARTESIAN_POINT('',(0.600000000000001,7.16704385318485,0.20586987765404));
#70855=CARTESIAN_POINT('',(9.,7.16704385318485,0.20586987765404));
#70856=CARTESIAN_POINT('',(17.4,6.92,0.));
#70857=CARTESIAN_POINT('',(17.4,7.22,0.25));
#70858=CARTESIAN_POINT('',(0.6,6.92,0.));
#70859=CARTESIAN_POINT('',(0.6,6.92,0.));
#70860=CARTESIAN_POINT('',(0.6,7.22,0.25));
#70861=CARTESIAN_POINT('Origin',(0.6,7.07,0.));
#70862=CARTESIAN_POINT('',(0.600000000000001,7.16704385318485,-0.20586987765404));
#70863=CARTESIAN_POINT('Origin',(0.600000000000001,0.,0.));
#70864=CARTESIAN_POINT('',(0.6,6.92,0.));
#70865=CARTESIAN_POINT('Origin',(0.6,6.92,0.));
#70866=CARTESIAN_POINT('',(17.4,7.16704385318485,-0.20586987765404));
#70867=CARTESIAN_POINT('',(9.,7.16704385318485,-0.205869877654039));
#70868=CARTESIAN_POINT('',(17.4,6.92,0.));
#70869=CARTESIAN_POINT('Origin',(17.4,7.07,0.));
#70870=CARTESIAN_POINT('Origin',(17.4,0.,0.));
#70871=CARTESIAN_POINT('Origin',(9.,0.,0.));
#70872=CARTESIAN_POINT('',(18.,-7.17,-8.78071754988652E-16));
#70873=CARTESIAN_POINT('Origin',(18.,0.,0.));
#70874=CARTESIAN_POINT('',(9.,-7.17,-8.78071754988652E-16));
#70875=CARTESIAN_POINT('',(9.,-7.17,-8.78071754988652E-16));
#70876=CARTESIAN_POINT('Origin',(18.4,0.,0.));
#70877=CARTESIAN_POINT('',(18.4,-6.76,-8.27861236223611E-16));
#70878=CARTESIAN_POINT('',(0.,0.,0.));
#70879=CARTESIAN_POINT('Origin',(14.1667966825785,0.,-2.87239068222369E-16));
#70880=CARTESIAN_POINT('',(14.3,-8.45882352941176,1.03590711598464E-15));
#70881=CARTESIAN_POINT('Origin',(14.3,0.,0.));
#70882=CARTESIAN_POINT('',(14.0966872156073,-9.1646003104954,-0.000235982960761385));
#70883=CARTESIAN_POINT('',(14.1667966825785,-8.9203817394342,-1.6669098308818E-15));
#70884=CARTESIAN_POINT('',(14.0358618182521,-9.09714729409388,-2.2913561246914));
#70885=CARTESIAN_POINT('Ctrl Pts',(14.0966872156073,-9.1646003104954,-0.000235982960761354));
#70886=CARTESIAN_POINT('Ctrl Pts',(14.096667975927,-9.16460269692416,-0.0788499963175328));
#70887=CARTESIAN_POINT('Ctrl Pts',(14.0964337489381,-9.16436435538848,-0.157458304901251));
#70888=CARTESIAN_POINT('Ctrl Pts',(14.0959893606634,-9.16388490893575,-0.23607213292966));
#70889=CARTESIAN_POINT('Ctrl Pts',(14.0951146780166,-9.16294122181289,-0.390806528744216));
#70890=CARTESIAN_POINT('Ctrl Pts',(14.0934278040135,-9.16106393006443,-0.545363216810532));
#70891=CARTESIAN_POINT('Ctrl Pts',(14.0909765857551,-9.15825881192215,-0.699825257957074));
#70892=CARTESIAN_POINT('Ctrl Pts',(14.0891704149768,-9.15619187137072,-0.813640020939149));
#70893=CARTESIAN_POINT('Ctrl Pts',(14.0869493584505,-9.15362107196599,-0.927403243780337));
#70894=CARTESIAN_POINT('Ctrl Pts',(14.0842873855616,-9.15055006079841,-1.04117270406207));
#70895=CARTESIAN_POINT('Ctrl Pts',(14.0808085904244,-9.14653671462165,-1.1898521466101));
#70896=CARTESIAN_POINT('Ctrl Pts',(14.0765836260547,-9.14167463053302,-1.33830456859723));
#70897=CARTESIAN_POINT('Ctrl Pts',(14.0715649306596,-9.1359838442516,-1.48668516439165));
#70898=CARTESIAN_POINT('Ctrl Pts',(14.0667384825238,-9.13051105049219,-1.62938186015989));
#70899=CARTESIAN_POINT('Ctrl Pts',(14.0611778355173,-9.12427176256957,-1.77201223274345));
#70900=CARTESIAN_POINT('Ctrl Pts',(14.0548601236482,-9.11728218271552,-1.91467104387642));
#70901=CARTESIAN_POINT('Ctrl Pts',(14.0493110055173,-9.11114293402874,-2.0399744150652));
#70902=CARTESIAN_POINT('Ctrl Pts',(14.0431780217821,-9.10442480241651,-2.16529922277692));
#70903=CARTESIAN_POINT('Ctrl Pts',(14.0364597916687,-9.0971382152186,-2.29067954584981));
#70904=CARTESIAN_POINT('',(14.0346021788821,-6.53571152371397,-6.73113542385575));
#70905=CARTESIAN_POINT('Origin',(14.0335933651569,0.,-5.74478136444738E-16));
#70906=CARTESIAN_POINT('',(14.0357899498044,-2.56414768532747,-9.02407043229182));
#70907=CARTESIAN_POINT('Ctrl Pts',(14.0346021788821,-6.53571152371397,-6.73113542385575));
#70908=CARTESIAN_POINT('Ctrl Pts',(14.037490920202,-6.49086101686042,-6.76062130272172));
#70909=CARTESIAN_POINT('Ctrl Pts',(14.0402815726799,-6.44595104664353,-6.79002177619354));
#70910=CARTESIAN_POINT('Ctrl Pts',(14.0429752481594,-6.40097722143761,-6.81933831082405));
#70911=CARTESIAN_POINT('Ctrl Pts',(14.0504757625031,-6.27574802303614,-6.90096992910151));
#70912=CARTESIAN_POINT('Ctrl Pts',(14.0572232832294,-6.15002692231759,-6.98194901081926));
#70913=CARTESIAN_POINT('Ctrl Pts',(14.0631875076052,-6.02378040933136,-7.06227499667437));
#70914=CARTESIAN_POINT('Ctrl Pts',(14.0670738259238,-5.94151755247907,-7.11461580926091));
#70915=CARTESIAN_POINT('Ctrl Pts',(14.0706279215876,-5.85903066199963,-7.16667984778686));
#70916=CARTESIAN_POINT('Ctrl Pts',(14.0738450240434,-5.77630052750431,-7.21847226290525));
#70917=CARTESIAN_POINT('Ctrl Pts',(14.0791867260652,-5.63893476661847,-7.30446879312068));
#70918=CARTESIAN_POINT('Ctrl Pts',(14.0835906402011,-5.50109523148508,-7.38959315710351));
#70919=CARTESIAN_POINT('Ctrl Pts',(14.0870443139107,-5.36272714628941,-7.47386405825115));
#70920=CARTESIAN_POINT('Ctrl Pts',(14.0900251718151,-5.24330196743517,-7.54659808089469));
#70921=CARTESIAN_POINT('Ctrl Pts',(14.0922987244798,-5.12348189405599,-7.61869696507324));
#70922=CARTESIAN_POINT('Ctrl Pts',(14.0938730282238,-5.0032076555115,-7.6901839122321));
#70923=CARTESIAN_POINT('Ctrl Pts',(14.0960271700124,-4.83863473600432,-7.78800049991507));
#70924=CARTESIAN_POINT('Ctrl Pts',(14.0968652699818,-4.67348773079844,-7.8845083580373));
#70925=CARTESIAN_POINT('Ctrl Pts',(14.0964383665758,-4.5076387644692,-7.97977606599508));
#70926=CARTESIAN_POINT('Ctrl Pts',(14.0963267565809,-4.46427906755682,-8.00468293779545));
#70927=CARTESIAN_POINT('Ctrl Pts',(14.0961289474093,-4.42087129224503,-8.02950504143431));
#70928=CARTESIAN_POINT('Ctrl Pts',(14.0958463988297,-4.37741303746945,-8.0542435417795));
#70929=CARTESIAN_POINT('Ctrl Pts',(14.094972077556,-4.24293536027673,-8.13079461546694));
#70930=CARTESIAN_POINT('Ctrl Pts',(14.0932865822815,-4.10814556901557,-8.2064478459118));
#70931=CARTESIAN_POINT('Ctrl Pts',(14.0908378720276,-3.97297486435817,-8.2812496228984));
#70932=CARTESIAN_POINT('Ctrl Pts',(14.0890335492626,-3.87337484872653,-8.3363670255636));
#70933=CARTESIAN_POINT('Ctrl Pts',(14.0868149528525,-3.77356809910472,-8.39102197337117));
#70934=CARTESIAN_POINT('Ctrl Pts',(14.0841559268849,-3.67350630415314,-8.44524657114366));
#70935=CARTESIAN_POINT('Ctrl Pts',(14.0806813229798,-3.54275349928081,-8.5161029679858));
#70936=CARTESIAN_POINT('Ctrl Pts',(14.0764615201052,-3.41177376280883,-8.58611052772029));
#70937=CARTESIAN_POINT('Ctrl Pts',(14.0714486898468,-3.28044252824194,-8.65536429918192));
#70938=CARTESIAN_POINT('Ctrl Pts',(14.0666278773627,-3.15414197096834,-8.72196528681254));
#70939=CARTESIAN_POINT('Ctrl Pts',(14.0610735151129,-3.0275162045262,-8.7878691248368));
#70940=CARTESIAN_POINT('Ctrl Pts',(14.054762506757,-2.90049109866216,-8.85313731723162));
#70941=CARTESIAN_POINT('Ctrl Pts',(14.04921748605,-2.7888834438153,-8.9104836964354));
#70942=CARTESIAN_POINT('Ctrl Pts',(14.0430885450049,-2.67696791838211,-8.96733907859069));
#70943=CARTESIAN_POINT('Ctrl Pts',(14.036374153903,-2.56472008839194,-9.02372962028732));
#70944=CARTESIAN_POINT('',(14.0357899498032,2.56414768532832,-9.02407043229137));
#70945=CARTESIAN_POINT('Origin',(14.0335933651569,0.,-5.74478136444738E-16));
#70946=CARTESIAN_POINT('',(14.0346021788821,6.53571152371399,-6.73113542385574));
#70947=CARTESIAN_POINT('Ctrl Pts',(14.036374153903,2.56472008839191,-9.02372962028734));
#70948=CARTESIAN_POINT('Ctrl Pts',(14.0439581544769,2.69150561430802,-8.96003569866473));
#70949=CARTESIAN_POINT('Ctrl Pts',(14.0507940165627,2.81788693530708,-8.89574019624407));
#70950=CARTESIAN_POINT('Ctrl Pts',(14.056887537588,2.9439106365035,-8.83079680975475));
#70951=CARTESIAN_POINT('Ctrl Pts',(14.0631313247637,3.07304208055634,-8.76425192018689));
#70952=CARTESIAN_POINT('Ctrl Pts',(14.0685958234887,3.2017981474923,-8.69702680530498));
#70953=CARTESIAN_POINT('Ctrl Pts',(14.0733090155991,3.33027166379957,-8.62904584746935));
#70954=CARTESIAN_POINT('Ctrl Pts',(14.0737328173227,3.3418237703919,-8.62293312249895));
#70955=CARTESIAN_POINT('Ctrl Pts',(14.0741505579372,3.35337361963567,-8.61681426950855));
#70956=CARTESIAN_POINT('Ctrl Pts',(14.0745622655563,3.36492129486017,-8.61068922364997));
#70957=CARTESIAN_POINT('Ctrl Pts',(14.0794394387139,3.50171743128368,-8.5381306702978));
#70958=CARTESIAN_POINT('Ctrl Pts',(14.0834615310168,3.63801904201667,-8.46480359133271));
#70959=CARTESIAN_POINT('Ctrl Pts',(14.0866814188315,3.77393577057594,-8.39063029663735));
#70960=CARTESIAN_POINT('Ctrl Pts',(14.0882552127477,3.84036818462935,-8.35437640002625));
#70961=CARTESIAN_POINT('Ctrl Pts',(14.0896378032368,3.90670926990041,-8.31791993646687));
#70962=CARTESIAN_POINT('Ctrl Pts',(14.090837669424,3.97297492845534,-8.28124971544123));
#70963=CARTESIAN_POINT('Ctrl Pts',(14.0919557958865,4.03472630304775,-8.24707761779182));
#70964=CARTESIAN_POINT('Ctrl Pts',(14.0929152942354,4.09641222151585,-8.21271986900143));
#70965=CARTESIAN_POINT('Ctrl Pts',(14.0937114070427,4.15803990964946,-8.17817121287965));
#70966=CARTESIAN_POINT('Ctrl Pts',(14.0958985068728,4.32734494406736,-8.0832583321448));
#70967=CARTESIAN_POINT('Ctrl Pts',(14.0968439958901,4.49592110849515,-7.98706849201295));
#70968=CARTESIAN_POINT('Ctrl Pts',(14.0964643580788,4.66390152286281,-7.88952765023803));
#70969=CARTESIAN_POINT('Ctrl Pts',(14.0963723250581,4.7046238758636,-7.86588148526276));
#70970=CARTESIAN_POINT('Ctrl Pts',(14.0962026412764,4.74531125568717,-7.84215584473792));
#70971=CARTESIAN_POINT('Ctrl Pts',(14.095954561874,4.78596555791062,-7.81834956722902));
#70972=CARTESIAN_POINT('Ctrl Pts',(14.0950534684957,4.9336332891507,-7.73187854702333));
#70973=CARTESIAN_POINT('Ctrl Pts',(14.0931172756095,5.08065748201068,-7.64446522212414));
#70974=CARTESIAN_POINT('Ctrl Pts',(14.0901216005508,5.22713884337462,-7.55606608075544));
#70975=CARTESIAN_POINT('Ctrl Pts',(14.0884090550303,5.31087823243389,-7.50553070872822));
#70976=CARTESIAN_POINT('Ctrl Pts',(14.0863508376835,5.39443971659127,-7.4546733264031));
#70977=CARTESIAN_POINT('Ctrl Pts',(14.0839473935999,5.47783644876651,-7.40348815992952));
#70978=CARTESIAN_POINT('Ctrl Pts',(14.0801455293264,5.60975674545584,-7.32252141014012));
#70979=CARTESIAN_POINT('Ctrl Pts',(14.0754874908681,5.74104585820764,-7.24086784135944));
#70980=CARTESIAN_POINT('Ctrl Pts',(14.0699826640698,5.87179177769892,-7.15849937346099));
#70981=CARTESIAN_POINT('Ctrl Pts',(14.0646793238266,5.99775216153913,-7.07914573953355));
#70982=CARTESIAN_POINT('Ctrl Pts',(14.0585899970415,6.12320849014782,-6.9991284498085));
#70983=CARTESIAN_POINT('Ctrl Pts',(14.0517394686096,6.2481988125042,-6.91844353123613));
#70984=CARTESIAN_POINT('Ctrl Pts',(14.0489440163948,6.2992028302131,-6.88551894205096));
#70985=CARTESIAN_POINT('Ctrl Pts',(14.046022010621,6.35012876048407,-6.85248344327514));
#70986=CARTESIAN_POINT('Ctrl Pts',(14.0429759898738,6.40097709821819,-6.81933789599594));
#70987=CARTESIAN_POINT('Ctrl Pts',(14.0402820510809,6.44594800319266,-6.79002356000301));
#70988=CARTESIAN_POINT('Ctrl Pts',(14.0374911009489,6.49085821058925,-6.76062314763669));
#70989=CARTESIAN_POINT('Ctrl Pts',(14.0346021788821,6.53571152371399,-6.73113542385574));
#70990=CARTESIAN_POINT('',(14.0346846831548,9.09718960292736,-2.29455299637842));
#70991=CARTESIAN_POINT('Origin',(14.0335933651569,0.,-5.74478136444738E-16));
#70992=CARTESIAN_POINT('',(14.035861818251,9.09714729409392,2.2913561246905));
#70993=CARTESIAN_POINT('Ctrl Pts',(14.0346846831548,9.09718960292737,-2.29455299637841));
#70994=CARTESIAN_POINT('Ctrl Pts',(14.0375755696933,9.10029985513172,-2.24096964017326));
#70995=CARTESIAN_POINT('Ctrl Pts',(14.0403683507454,9.10330641202518,-2.18737754787367));
#70996=CARTESIAN_POINT('Ctrl Pts',(14.043064127072,9.1062083478486,-2.13377218640335));
#70997=CARTESIAN_POINT('Ctrl Pts',(14.0505699144896,9.11428814036511,-1.98452002343093));
#70998=CARTESIAN_POINT('Ctrl Pts',(14.0573226099963,9.12155698997572,-1.83516862171975));
#70999=CARTESIAN_POINT('Ctrl Pts',(14.0632917846551,9.12799766353303,-1.68568903224694));
#71000=CARTESIAN_POINT('Ctrl Pts',(14.0671820861082,9.1321952558521,-1.58826841760994));
#71001=CARTESIAN_POINT('Ctrl Pts',(14.0707399396716,9.13604105522664,-1.49079227060806));
#71002=CARTESIAN_POINT('Ctrl Pts',(14.0739605337436,9.13952991576929,-1.39324130828909));
#71003=CARTESIAN_POINT('Ctrl Pts',(14.079307034207,9.1453217647546,-1.23129719065638));
#71004=CARTESIAN_POINT('Ctrl Pts',(14.0837153543481,9.15012154561387,-1.06937897158459));
#71005=CARTESIAN_POINT('Ctrl Pts',(14.0871728595391,9.15391807261198,-0.907429557799676));
#71006=CARTESIAN_POINT('Ctrl Pts',(14.0901574685142,9.15719533408425,-0.767630585075904));
#71007=CARTESIAN_POINT('Ctrl Pts',(14.0924341327935,9.15972498534993,-0.627807045688716));
#71008=CARTESIAN_POINT('Ctrl Pts',(14.0940107917454,9.16149748328792,-0.487895780218637));
#71009=CARTESIAN_POINT('Ctrl Pts',(14.0961676570875,9.16392225585315,-0.296497533254805));
#71010=CARTESIAN_POINT('Ctrl Pts',(14.0970076672682,9.16492702857341,-0.105255742388477));
#71011=CARTESIAN_POINT('Ctrl Pts',(14.0965815587046,9.16450726213935,0.0859751166229818));
#71012=CARTESIAN_POINT('Ctrl Pts',(14.096470075072,9.16439743781078,0.13600722731108));
#71013=CARTESIAN_POINT('Ctrl Pts',(14.096272189818,9.16419005072871,0.186038673928651));
#71014=CARTESIAN_POINT('Ctrl Pts',(14.0959893606634,9.16388490893575,0.236072132929773));
#71015=CARTESIAN_POINT('Ctrl Pts',(14.0951146780166,9.16294122181289,0.390806528744278));
#71016=CARTESIAN_POINT('Ctrl Pts',(14.0934278040135,9.16106393006444,0.545363216810541));
#71017=CARTESIAN_POINT('Ctrl Pts',(14.0909765857551,9.15825881192215,0.699825257957071));
#71018=CARTESIAN_POINT('Ctrl Pts',(14.0891704149768,9.15619187137072,0.813640020939152));
#71019=CARTESIAN_POINT('Ctrl Pts',(14.0869493584505,9.15362107196599,0.927403243780368));
#71020=CARTESIAN_POINT('Ctrl Pts',(14.0842873855616,9.15055006079841,1.04117270406217));
#71021=CARTESIAN_POINT('Ctrl Pts',(14.0808085904244,9.14653671462164,1.18985214661074));
#71022=CARTESIAN_POINT('Ctrl Pts',(14.0765836260547,9.14167463053298,1.33830456859842));
#71023=CARTESIAN_POINT('Ctrl Pts',(14.0715649306595,9.13598384425154,1.48668516439338));
#71024=CARTESIAN_POINT('Ctrl Pts',(14.0667384825238,9.13051105049213,1.6293818601613));
#71025=CARTESIAN_POINT('Ctrl Pts',(14.0611778355173,9.12427176256952,1.77201223274453));
#71026=CARTESIAN_POINT('Ctrl Pts',(14.0548601236482,9.11728218271549,1.91467104387717));
#71027=CARTESIAN_POINT('Ctrl Pts',(14.0493110055172,9.11114293402872,2.03997441506574));
#71028=CARTESIAN_POINT('Ctrl Pts',(14.043178021782,9.1044248024165,2.16529922277725));
#71029=CARTESIAN_POINT('Ctrl Pts',(14.0364597916687,9.0971382152186,2.29067954584992));
#71030=CARTESIAN_POINT('',(14.0346021788821,6.53571152371428,6.73113542385557));
#71031=CARTESIAN_POINT('Origin',(14.0335933651569,0.,-5.74478136444738E-16));
#71032=CARTESIAN_POINT('',(14.0357899498033,2.56414768532805,9.02407043229152));
#71033=CARTESIAN_POINT('Ctrl Pts',(14.0346021788821,6.53571152371428,6.73113542385557));
#71034=CARTESIAN_POINT('Ctrl Pts',(14.037490920202,6.49086101686062,6.76062130272161));
#71035=CARTESIAN_POINT('Ctrl Pts',(14.0402815726799,6.44595104664364,6.79002177619349));
#71036=CARTESIAN_POINT('Ctrl Pts',(14.0429752481594,6.40097722143762,6.81933831082406));
#71037=CARTESIAN_POINT('Ctrl Pts',(14.0504757625032,6.27574802303421,6.90096992910279));
#71038=CARTESIAN_POINT('Ctrl Pts',(14.0572232832295,6.15002692231372,6.98194901082178));
#71039=CARTESIAN_POINT('Ctrl Pts',(14.0631875076055,6.02378040932554,7.06227499667809));
#71040=CARTESIAN_POINT('Ctrl Pts',(14.0670738259239,5.9415175524751,7.11461580926345));
#71041=CARTESIAN_POINT('Ctrl Pts',(14.0706279215876,5.85903066199751,7.16667984778822));
#71042=CARTESIAN_POINT('Ctrl Pts',(14.0738450240434,5.77630052750406,7.21847226290544));
#71043=CARTESIAN_POINT('Ctrl Pts',(14.079186726065,5.63893476662222,7.30446879311835));
#71044=CARTESIAN_POINT('Ctrl Pts',(14.0835906402009,5.5010952314928,7.38959315709877));
#71045=CARTESIAN_POINT('Ctrl Pts',(14.0870443139104,5.3627271463011,7.47386405824405));
#71046=CARTESIAN_POINT('Ctrl Pts',(14.0900251718149,5.24330196744293,7.54659808089004));
#71047=CARTESIAN_POINT('Ctrl Pts',(14.0922987244797,5.1234818940598,7.618696965071));
#71048=CARTESIAN_POINT('Ctrl Pts',(14.0938730282238,5.00320765551131,7.69018391223224));
#71049=CARTESIAN_POINT('Ctrl Pts',(14.0960271700123,4.838634736007,7.7880004999135));
#71050=CARTESIAN_POINT('Ctrl Pts',(14.0968652699817,4.67348773080399,7.88450835803408));
#71051=CARTESIAN_POINT('Ctrl Pts',(14.0964383665758,4.50763876447763,7.97977606599027));
#71052=CARTESIAN_POINT('Ctrl Pts',(14.0963267565808,4.46427906756238,8.0046829377923));
#71053=CARTESIAN_POINT('Ctrl Pts',(14.0961289474093,4.42087129224772,8.02950504143281));
#71054=CARTESIAN_POINT('Ctrl Pts',(14.0958463988297,4.37741303746927,8.05424354177964));
#71055=CARTESIAN_POINT('Ctrl Pts',(14.0949720775559,4.24293536027659,8.13079461546704));
#71056=CARTESIAN_POINT('Ctrl Pts',(14.0932865822815,4.10814556901548,8.20644784591187));
#71057=CARTESIAN_POINT('Ctrl Pts',(14.0908378720275,3.97297486435819,8.28124962289842));
#71058=CARTESIAN_POINT('Ctrl Pts',(14.0890335492626,3.87337484872643,8.33636702556368));
#71059=CARTESIAN_POINT('Ctrl Pts',(14.0868149528524,3.77356809910453,8.3910219733713));
#71060=CARTESIAN_POINT('Ctrl Pts',(14.0841559268849,3.6735063041529,8.44524657114381));
#71061=CARTESIAN_POINT('Ctrl Pts',(14.0806813229798,3.54275349928009,8.51610296798621));
#71062=CARTESIAN_POINT('Ctrl Pts',(14.0764615201051,3.41177376280762,8.58611052772096));
#71063=CARTESIAN_POINT('Ctrl Pts',(14.0714486898467,3.28044252824023,8.65536429918285));
#71064=CARTESIAN_POINT('Ctrl Pts',(14.0666278773626,3.1541419709661,8.72196528681374));
#71065=CARTESIAN_POINT('Ctrl Pts',(14.0610735151127,3.02751620452341,8.78786912483827));
#71066=CARTESIAN_POINT('Ctrl Pts',(14.0547625067568,2.90049109865881,8.85313731723337));
#71067=CARTESIAN_POINT('Ctrl Pts',(14.0492174860498,2.78888344381294,8.91048369643663));
#71068=CARTESIAN_POINT('Ctrl Pts',(14.0430885450048,2.67696791838073,8.96733907859141));
#71069=CARTESIAN_POINT('Ctrl Pts',(14.0363741539029,2.56472008839153,9.02372962028756));
#71070=CARTESIAN_POINT('',(14.0357899498033,-2.56414768532805,9.02407043229152));
#71071=CARTESIAN_POINT('Origin',(14.0335933651569,0.,-5.74478136444738E-16));
#71072=CARTESIAN_POINT('',(14.0346021788821,-6.53571152371428,6.73113542385556));
#71073=CARTESIAN_POINT('Ctrl Pts',(14.0363741539029,-2.56472008839153,9.02372962028756));
#71074=CARTESIAN_POINT('Ctrl Pts',(14.043958154477,-2.69150561431106,8.96003569866323));
#71075=CARTESIAN_POINT('Ctrl Pts',(14.050794016563,-2.81788693531343,8.89574019624087));
#71076=CARTESIAN_POINT('Ctrl Pts',(14.0568875375885,-2.94391063651312,8.83079680974982));
#71077=CARTESIAN_POINT('Ctrl Pts',(14.0631313247643,-3.07304208056859,8.76425192018057));
#71078=CARTESIAN_POINT('Ctrl Pts',(14.0685958234893,-3.20179814750712,8.69702680529725));
#71079=CARTESIAN_POINT('Ctrl Pts',(14.0733090155997,-3.33027166381696,8.62904584746018));
#71080=CARTESIAN_POINT('Ctrl Pts',(14.0737328173231,-3.34182377040356,8.6229331224928));
#71081=CARTESIAN_POINT('Ctrl Pts',(14.0741505579373,-3.35337361964161,8.61681426950542));
#71082=CARTESIAN_POINT('Ctrl Pts',(14.0745622655563,-3.36492129486038,8.61068922364988));
#71083=CARTESIAN_POINT('Ctrl Pts',(14.0794394387138,-3.50171743128173,8.53813067029886));
#71084=CARTESIAN_POINT('Ctrl Pts',(14.0834615310167,-3.63801904201261,8.46480359133492));
#71085=CARTESIAN_POINT('Ctrl Pts',(14.0866814188314,-3.77393577056981,8.39063029664073));
#71086=CARTESIAN_POINT('Ctrl Pts',(14.0882552127476,-3.84036818462527,8.35437640002852));
#71087=CARTESIAN_POINT('Ctrl Pts',(14.0896378032368,-3.90670926989839,8.31791993646802));
#71088=CARTESIAN_POINT('Ctrl Pts',(14.0908376694239,-3.97297492845536,8.28124971544124));
#71089=CARTESIAN_POINT('Ctrl Pts',(14.0919557958864,-4.0347263030478,8.24707761779182));
#71090=CARTESIAN_POINT('Ctrl Pts',(14.0929152942353,-4.09641222151593,8.21271986900141));
#71091=CARTESIAN_POINT('Ctrl Pts',(14.0937114070427,-4.15803990964958,8.17817121287961));
#71092=CARTESIAN_POINT('Ctrl Pts',(14.0958985068726,-4.32734494405542,8.08325833215152));
#71093=CARTESIAN_POINT('Ctrl Pts',(14.0968439958899,-4.49592110847136,7.98706849202655));
#71094=CARTESIAN_POINT('Ctrl Pts',(14.0964643580789,-4.66390152282726,7.8895276502587));
#71095=CARTESIAN_POINT('Ctrl Pts',(14.0963723250581,-4.70462387583996,7.86588148527657));
#71096=CARTESIAN_POINT('Ctrl Pts',(14.0962026412765,-4.74531125567541,7.84215584474483));
#71097=CARTESIAN_POINT('Ctrl Pts',(14.0959545618739,-4.78596555791072,7.81834956722898));
#71098=CARTESIAN_POINT('Ctrl Pts',(14.0950534684957,-4.93363328914806,7.7318785470249));
#71099=CARTESIAN_POINT('Ctrl Pts',(14.0931172756096,-5.08065748200534,7.64446522212734));
#71100=CARTESIAN_POINT('Ctrl Pts',(14.0901216005509,-5.22713884336655,7.55606608076033));
#71101=CARTESIAN_POINT('Ctrl Pts',(14.0884090550304,-5.31087823242858,7.50553070873148));
#71102=CARTESIAN_POINT('Ctrl Pts',(14.0863508376835,-5.3944397165887,7.4546733264047));
#71103=CARTESIAN_POINT('Ctrl Pts',(14.0839473935998,-5.47783644876665,7.40348815992946));
#71104=CARTESIAN_POINT('Ctrl Pts',(14.0801455293263,-5.60975674545588,7.32252141014012));
#71105=CARTESIAN_POINT('Ctrl Pts',(14.0754874908681,-5.74104585820757,7.2408678413595));
#71106=CARTESIAN_POINT('Ctrl Pts',(14.0699826640698,-5.87179177769875,7.15849937346112));
#71107=CARTESIAN_POINT('Ctrl Pts',(14.0646793238266,-5.9977521615382,7.07914573953416));
#71108=CARTESIAN_POINT('Ctrl Pts',(14.0585899970416,-6.12320849014614,6.99912844980959));
#71109=CARTESIAN_POINT('Ctrl Pts',(14.0517394686097,-6.24819881250178,6.91844353123771));
#71110=CARTESIAN_POINT('Ctrl Pts',(14.0489440163948,-6.2992028302115,6.88551894205202));
#71111=CARTESIAN_POINT('Ctrl Pts',(14.046022010621,-6.35012876048327,6.85248344327568));
#71112=CARTESIAN_POINT('Ctrl Pts',(14.0429759898737,-6.4009770982182,6.81933789599595));
#71113=CARTESIAN_POINT('Ctrl Pts',(14.0402820510809,-6.44594800319277,6.79002356000296));
#71114=CARTESIAN_POINT('Ctrl Pts',(14.0374911009489,-6.49085821058945,6.76062314763658));
#71115=CARTESIAN_POINT('Ctrl Pts',(14.0346021788821,-6.53571152371428,6.73113542385556));
#71116=CARTESIAN_POINT('',(14.0346124314935,-9.09718908205277,2.29451127187482));
#71117=CARTESIAN_POINT('Origin',(14.0335933651569,0.,-5.74478136444738E-16));
#71118=CARTESIAN_POINT('Ctrl Pts',(14.0346846831548,-9.09718960292737,2.2945529963785));
#71119=CARTESIAN_POINT('Ctrl Pts',(14.0375755696933,-9.10029985513173,2.24096964017332));
#71120=CARTESIAN_POINT('Ctrl Pts',(14.0403683507454,-9.10330641202519,2.18737754787371));
#71121=CARTESIAN_POINT('Ctrl Pts',(14.043064127072,-9.10620834784861,2.13377218640334));
#71122=CARTESIAN_POINT('Ctrl Pts',(14.0505699144896,-9.11428814036506,1.98452002343198));
#71123=CARTESIAN_POINT('Ctrl Pts',(14.0573226099962,-9.12155698997562,1.83516862172181));
#71124=CARTESIAN_POINT('Ctrl Pts',(14.063291784655,-9.1279976635329,1.68568903225001));
#71125=CARTESIAN_POINT('Ctrl Pts',(14.0671820861081,-9.13219525585202,1.58826841761204));
#71126=CARTESIAN_POINT('Ctrl Pts',(14.0707399396716,-9.1360410552266,1.49079227060918));
#71127=CARTESIAN_POINT('Ctrl Pts',(14.0739605337436,-9.13952991576929,1.39324130828922));
#71128=CARTESIAN_POINT('Ctrl Pts',(14.0793070342071,-9.14532176475466,1.23129719065468));
#71129=CARTESIAN_POINT('Ctrl Pts',(14.0837153543482,-9.15012154561397,1.06937897158109));
#71130=CARTESIAN_POINT('Ctrl Pts',(14.0871728595392,-9.1539180726121,0.907429557794384));
#71131=CARTESIAN_POINT('Ctrl Pts',(14.0901574685142,-9.15719533408431,0.767630585072405));
#71132=CARTESIAN_POINT('Ctrl Pts',(14.0924341327935,-9.15972498534995,0.627807045687021));
#71133=CARTESIAN_POINT('Ctrl Pts',(14.0940107917454,-9.16149748328792,0.487895780218749));
#71134=CARTESIAN_POINT('Ctrl Pts',(14.0958453211638,-9.16355988213915,0.325101326699524));
#71135=CARTESIAN_POINT('Ctrl Pts',(14.0967276209543,-9.16459504304142,0.162420881184377));
#71136=CARTESIAN_POINT('Ctrl Pts',(14.0966872156073,-9.1646003104954,-0.000235982960761354));
#71137=CARTESIAN_POINT('Ctrl Pts',(12.6361849146756,-0.403980496774264,
-10.7652843795024));
#71138=CARTESIAN_POINT('Ctrl Pts',(13.1323548632684,-1.83314667576049,-9.94015490134798));
#71139=CARTESIAN_POINT('Ctrl Pts',(13.5259820957649,-3.8118564888613,-8.79774625810608));
#71140=CARTESIAN_POINT('Ctrl Pts',(13.3920458446166,-6.48443612385918,-7.25473168640934));
#71141=CARTESIAN_POINT('Ctrl Pts',(12.9669648804042,-8.16824205056825,-6.28258588136077));
#71142=CARTESIAN_POINT('Ctrl Pts',(12.6361849146757,-9.12101950322573,-5.73249956259117));
#71143=CARTESIAN_POINT('Ctrl Pts',(12.8699890291072,-0.269320331182842,
-10.6726380968212));
#71144=CARTESIAN_POINT('Ctrl Pts',(13.3767756515671,-1.71258108335182,-9.84301179383112));
#71145=CARTESIAN_POINT('Ctrl Pts',(13.7845689781422,-3.72407315433307,-8.68667090248932));
#71146=CARTESIAN_POINT('Ctrl Pts',(13.6453803397493,-6.44473655178331,-7.11403939432886));
#71147=CARTESIAN_POINT('Ctrl Pts',(13.2078467774138,-8.14804366490556,-6.12628217974948));
#71148=CARTESIAN_POINT('Ctrl Pts',(12.8699890291072,-9.10811555165335,-5.56955729697059));
#71149=CARTESIAN_POINT('Ctrl Pts',(13.1037931435388,-0.134660165591419,
-10.57999181414));
#71150=CARTESIAN_POINT('Ctrl Pts',(13.6211964398659,-1.59201549094316,-9.74586868631425));
#71151=CARTESIAN_POINT('Ctrl Pts',(14.0431558605194,-3.63628981980485,-8.57559554687257));
#71152=CARTESIAN_POINT('Ctrl Pts',(13.898714834882,-6.40503697970743,-6.97334710224838));
#71153=CARTESIAN_POINT('Ctrl Pts',(13.4487286744235,-8.12784527924288,-5.96997847813818));
#71154=CARTESIAN_POINT('Ctrl Pts',(13.1037931435388,-9.09521160008097,-5.40661503135001));
#71155=CARTESIAN_POINT('Ctrl Pts',(13.3375972579703,2.97082320207775E-15,
-10.4873455314589));
#71156=CARTESIAN_POINT('Ctrl Pts',(13.8656172281646,-1.4714498985345,-9.64872557879739));
#71157=CARTESIAN_POINT('Ctrl Pts',(14.3017427428967,-3.54850648527662,-8.46452019125581));
#71158=CARTESIAN_POINT('Ctrl Pts',(14.1520493300147,-6.36533740763157,-6.83265481016789));
#71159=CARTESIAN_POINT('Ctrl Pts',(13.6896105714332,-8.1076468935802,-5.81367477652689));
#71160=CARTESIAN_POINT('Ctrl Pts',(13.3375972579703,-9.08230764850859,-5.24367276572944));
#71161=CARTESIAN_POINT('',(13.3375972579703,-9.0823076485086,-5.24367276572943));
#71162=CARTESIAN_POINT('Ctrl Pts',(14.0346021788807,-6.53571152372215,-6.73113542385098));
#71163=CARTESIAN_POINT('Ctrl Pts',(13.8952900661411,-7.33167501862017,-6.26749768919284));
#71164=CARTESIAN_POINT('Ctrl Pts',(13.6704419928349,-8.16072119666195,-5.78263581314881));
#71165=CARTESIAN_POINT('Ctrl Pts',(13.3375972579703,-9.08230764850859,-5.24367276572944));
#71166=CARTESIAN_POINT('',(12.6462384144175,-9.0919872981105,-5.74926131402961));
#71167=CARTESIAN_POINT('Ctrl Pts',(12.6462384144175,-9.0919872981105,-5.74926131402961));
#71168=CARTESIAN_POINT('Ctrl Pts',(12.7615608863228,-9.0902706516109,-5.66510306978528));
#71169=CARTESIAN_POINT('Ctrl Pts',(12.8768443884274,-9.08860556242311,-5.58088496917862));
#71170=CARTESIAN_POINT('Ctrl Pts',(13.1072956815908,-9.08537904841867,-5.41235664115676));
#71171=CARTESIAN_POINT('Ctrl Pts',(13.2224686011676,-9.08381752761855,-5.32804270515258));
#71172=CARTESIAN_POINT('Ctrl Pts',(13.3375972579703,-9.08230764850859,-5.24367276572944));
#71173=CARTESIAN_POINT('',(12.6462384144167,-0.433012701892221,-10.7485226280624));
#71174=CARTESIAN_POINT('Ctrl Pts',(12.6462397169616,-9.09198644037733,-5.7492618092421));
#71175=CARTESIAN_POINT('Ctrl Pts',(12.9712786667833,-8.15112288573813,-6.29246963578375));
#71176=CARTESIAN_POINT('Ctrl Pts',(13.3924350002713,-6.47667086636881,-7.25921495991174));
#71177=CARTESIAN_POINT('Ctrl Pts',(13.5255929401102,-3.81962174635228,-8.79326298460333));
#71178=CARTESIAN_POINT('Ctrl Pts',(13.1355491140167,-1.84924327825312,-9.93086152356582));
#71179=CARTESIAN_POINT('Ctrl Pts',(12.6462405439417,-0.433014589690331,
-10.7485215381416));
#71180=CARTESIAN_POINT('',(13.3375972579703,-1.68649378841241E-15,-10.4873455314589));
#71181=CARTESIAN_POINT('Ctrl Pts',(13.3375972579703,2.97082320207775E-15,
-10.4873455314589));
#71182=CARTESIAN_POINT('Ctrl Pts',(13.2224673861593,-0.0723123344410041,
-10.530838553834));
#71183=CARTESIAN_POINT('Ctrl Pts',(13.1072932506126,-0.144550346101911,
-10.5743482978785));
#71184=CARTESIAN_POINT('Ctrl Pts',(12.8768419556923,-0.288886899219771,
-10.6614067056461));
#71185=CARTESIAN_POINT('Ctrl Pts',(12.7615596695621,-0.360988607620142,
-10.7049573061223));
#71186=CARTESIAN_POINT('Ctrl Pts',(12.6462384144189,-0.433012701893692,
-10.7485226280615));
#71187=CARTESIAN_POINT('Ctrl Pts',(13.3375972579703,2.97082320207775E-15,
-10.4873455314589));
#71188=CARTESIAN_POINT('Ctrl Pts',(13.6704419928349,-0.927548916689568,
-9.9587097760858));
#71189=CARTESIAN_POINT('Ctrl Pts',(13.8974523690185,-1.765606325871,-9.48097436223191));
#71190=CARTESIAN_POINT('Ctrl Pts',(14.0363741539015,-2.56472008838367,-9.02372962029205));
#71191=CARTESIAN_POINT('Ctrl Pts',(12.6361849146756,-9.525,-5.03278481691122));
#71192=CARTESIAN_POINT('Ctrl Pts',(13.1323548632684,-9.525,-3.38252586060241));
#71193=CARTESIAN_POINT('Ctrl Pts',(13.5261795528199,-9.525,-1.0975656251991));
#71194=CARTESIAN_POINT('Ctrl Pts',(13.3921464946308,-9.525,1.98832724851365));
#71195=CARTESIAN_POINT('Ctrl Pts',(12.9669648804042,-9.525,3.93261217937201));
#71196=CARTESIAN_POINT('Ctrl Pts',(12.6361849146757,-9.525,5.03278481691122));
#71197=CARTESIAN_POINT('Ctrl Pts',(12.8699890291072,-9.3774358828362,-5.10308079985063));
#71198=CARTESIAN_POINT('Ctrl Pts',(13.3767756515671,-9.3805888048835,-3.4383671726922));
#71199=CARTESIAN_POINT('Ctrl Pts',(13.7847648925596,-9.38491352314618,-1.11803995403544));
#71200=CARTESIAN_POINT('Ctrl Pts',(13.6454811073302,-9.38330701946683,2.02429453530628));
#71201=CARTESIAN_POINT('Ctrl Pts',(13.2078467774138,-9.37953783086773,3.99327171507834));
#71202=CARTESIAN_POINT('Ctrl Pts',(12.8699890291072,-9.3774358828362,5.10308079985062));
#71203=CARTESIAN_POINT('Ctrl Pts',(13.1037931435388,-9.2298717656724,-5.17337678279003));
#71204=CARTESIAN_POINT('Ctrl Pts',(13.6211964398659,-9.236177609767,-3.49420848478199));
#71205=CARTESIAN_POINT('Ctrl Pts',(14.0433502322992,-9.24482704629237,-1.13851428287178));
#71206=CARTESIAN_POINT('Ctrl Pts',(13.8988157200297,-9.24161403893367,2.06026182209891));
#71207=CARTESIAN_POINT('Ctrl Pts',(13.4487286744235,-9.23407566173547,4.05393125078467));
#71208=CARTESIAN_POINT('Ctrl Pts',(13.1037931435388,-9.2298717656724,5.17337678279003));
#71209=CARTESIAN_POINT('Ctrl Pts',(13.3375972579703,-9.0823076485086,-5.24367276572943));
#71210=CARTESIAN_POINT('Ctrl Pts',(13.8656172281646,-9.09176641465051,-3.55004979687178));
#71211=CARTESIAN_POINT('Ctrl Pts',(14.3019355720389,-9.10474056943856,-1.15898861170811));
#71212=CARTESIAN_POINT('Ctrl Pts',(14.1521503327292,-9.0999210584005,2.09622910889154));
#71213=CARTESIAN_POINT('Ctrl Pts',(13.6896105714332,-9.0886134926032,4.114590786491));
#71214=CARTESIAN_POINT('Ctrl Pts',(13.3375972579703,-9.08230764850859,5.24367276572943));
#71215=CARTESIAN_POINT('',(13.3375972579703,-9.08230764850859,5.24367276572943));
#71216=CARTESIAN_POINT('Ctrl Pts',(14.0346846831534,-9.09718960292733,2.29455299638773));
#71217=CARTESIAN_POINT('Ctrl Pts',(13.8953352172327,-9.09364959832235,3.21567361322219));
#71218=CARTESIAN_POINT('Ctrl Pts',(13.6704419928349,-9.08827011335153,4.17607396293699));
#71219=CARTESIAN_POINT('Ctrl Pts',(13.3375972579703,-9.08230764850859,5.24367276572943));
#71220=CARTESIAN_POINT('',(12.6462384144175,-9.525,4.99926131403433));
#71221=CARTESIAN_POINT('Ctrl Pts',(12.6462384144175,-9.525,4.99926131403433));
#71222=CARTESIAN_POINT('Ctrl Pts',(12.761560886318,-9.45125849929978,5.03985377667684));
#71223=CARTESIAN_POINT('Ctrl Pts',(12.8768443884248,-9.37749094012068,5.08052081744472));
#71224=CARTESIAN_POINT('Ctrl Pts',(13.1072956815865,-9.22992786979522,5.16199073836157));
#71225=CARTESIAN_POINT('Ctrl Pts',(13.2224686011656,-9.1561290989211,5.20279538968299));
#71226=CARTESIAN_POINT('Ctrl Pts',(13.3375972579703,-9.08230764850859,5.24367276572943));
#71227=CARTESIAN_POINT('',(12.6462384144167,-9.525,-4.99926131403118));
#71228=CARTESIAN_POINT('Ctrl Pts',(12.6462397325099,-9.525,4.99926032466067));
#71229=CARTESIAN_POINT('Ctrl Pts',(12.9712796891567,-9.525,3.91284474029011));
#71230=CARTESIAN_POINT('Ctrl Pts',(13.3925359315611,-9.525,1.97936109744437));
#71231=CARTESIAN_POINT('Ctrl Pts',(13.5257901158896,-9.525,-1.08859947412911));
#71232=CARTESIAN_POINT('Ctrl Pts',(13.1355507160135,-9.525,-3.36393794605574));
#71233=CARTESIAN_POINT('Ctrl Pts',(12.646240560211,-9.525,-4.99925912241684));
#71234=CARTESIAN_POINT('Ctrl Pts',(13.3375972579703,-9.0823076485086,-5.24367276572943));
#71235=CARTESIAN_POINT('Ctrl Pts',(13.2224673861572,-9.15612987799469,-5.20279495828338));
#71236=CARTESIAN_POINT('Ctrl Pts',(13.1072932506082,-9.22992942748129,-5.16198987708763));
#71237=CARTESIAN_POINT('Ctrl Pts',(12.8768419556921,-9.37749249677728,-5.08051995927811));
#71238=CARTESIAN_POINT('Ctrl Pts',(12.7615596695613,-9.45125927734028,-5.03985334838505));
#71239=CARTESIAN_POINT('Ctrl Pts',(12.6462384144189,-9.525,-4.99926131402949));
#71240=CARTESIAN_POINT('Ctrl Pts',(13.3375972579703,-9.0823076485086,-5.24367276572943));
#71241=CARTESIAN_POINT('Ctrl Pts',(13.6704419928349,-9.08827011335153,-4.176073962937));
#71242=CARTESIAN_POINT('Ctrl Pts',(13.8974983424166,-9.09356729120583,-3.21138559340686));
#71243=CARTESIAN_POINT('Ctrl Pts',(14.0364597916673,-9.09713821521857,-2.29067954585915));
#71244=CARTESIAN_POINT('Origin',(13.55,0.,0.));
#71245=CARTESIAN_POINT('Origin',(13.55,0.,0.));
#71246=CARTESIAN_POINT('Ctrl Pts',(13.3375972579703,-9.0823076485086,5.24367276572943));
#71247=CARTESIAN_POINT('Ctrl Pts',(13.6704419928349,-8.16072119666196,5.7826358131488));
#71248=CARTESIAN_POINT('Ctrl Pts',(13.8952900661411,-7.33167501862017,6.26749768919284));
#71249=CARTESIAN_POINT('Ctrl Pts',(14.0346021788807,-6.53571152372215,6.73113542385098));
#71250=CARTESIAN_POINT('Origin',(13.55,0.,0.));
#71251=CARTESIAN_POINT('',(13.3375972579703,6.4216470683267E-16,10.4873455314589));
#71252=CARTESIAN_POINT('Ctrl Pts',(13.3375972579703,6.4216470683267E-16,
10.4873455314589));
#71253=CARTESIAN_POINT('Ctrl Pts',(13.6704419928349,0.927548916689572,9.9587097760858));
#71254=CARTESIAN_POINT('Ctrl Pts',(13.8974523690185,1.76560632587101,9.4809743622319));
#71255=CARTESIAN_POINT('Ctrl Pts',(14.0363741539015,2.56472008838367,9.02372962029205));
#71256=CARTESIAN_POINT('Ctrl Pts',(14.0363741539015,-2.56472008838366,9.02372962029206));
#71257=CARTESIAN_POINT('Ctrl Pts',(13.8974523690185,-1.765606325871,9.48097436223191));
#71258=CARTESIAN_POINT('Ctrl Pts',(13.6704419928349,-0.927548916689566,
9.9587097760858));
#71259=CARTESIAN_POINT('Ctrl Pts',(13.3375972579703,2.97082320207775E-15,
10.4873455314589));
#71260=CARTESIAN_POINT('Origin',(13.55,0.,0.));
#71261=CARTESIAN_POINT('',(13.3375972579703,9.08230764850859,5.24367276572943));
#71262=CARTESIAN_POINT('Ctrl Pts',(13.3375972579703,9.08230764850859,5.24367276572943));
#71263=CARTESIAN_POINT('Ctrl Pts',(13.6704419928349,9.08827011335153,4.17607396293699));
#71264=CARTESIAN_POINT('Ctrl Pts',(13.8974983424166,9.09356729120583,3.21138559340686));
#71265=CARTESIAN_POINT('Ctrl Pts',(14.0364597916673,9.09713821521856,2.29067954585916));
#71266=CARTESIAN_POINT('Ctrl Pts',(14.0346021788807,6.53571152372216,6.73113542385098));
#71267=CARTESIAN_POINT('Ctrl Pts',(13.8952900661411,7.33167501862018,6.26749768919284));
#71268=CARTESIAN_POINT('Ctrl Pts',(13.6704419928349,8.16072119666196,5.7826358131488));
#71269=CARTESIAN_POINT('Ctrl Pts',(13.3375972579703,9.0823076485086,5.24367276572943));
#71270=CARTESIAN_POINT('Origin',(13.55,0.,0.));
#71271=CARTESIAN_POINT('',(13.3375972579703,9.08230764850859,-5.24367276572944));
#71272=CARTESIAN_POINT('Ctrl Pts',(13.3375972579703,9.08230764850859,-5.24367276572944));
#71273=CARTESIAN_POINT('Ctrl Pts',(13.6704419928349,8.16072119666195,-5.78263581314881));
#71274=CARTESIAN_POINT('Ctrl Pts',(13.8952900661411,7.33167501862017,-6.26749768919285));
#71275=CARTESIAN_POINT('Ctrl Pts',(14.0346021788807,6.53571152372214,-6.73113542385099));
#71276=CARTESIAN_POINT('Ctrl Pts',(14.0346846831534,9.09718960292733,-2.29455299638774));
#71277=CARTESIAN_POINT('Ctrl Pts',(13.8953352172327,9.09364959832235,-3.2156736132222));
#71278=CARTESIAN_POINT('Ctrl Pts',(13.6704419928349,9.08827011335152,-4.176073962937));
#71279=CARTESIAN_POINT('Ctrl Pts',(13.3375972579703,9.08230764850859,-5.24367276572944));
#71280=CARTESIAN_POINT('Origin',(13.55,0.,0.));
#71281=CARTESIAN_POINT('Ctrl Pts',(14.0363741539015,2.56472008838366,-9.02372962029206));
#71282=CARTESIAN_POINT('Ctrl Pts',(13.8974523690185,1.76560632587099,-9.48097436223191));
#71283=CARTESIAN_POINT('Ctrl Pts',(13.6704419928349,0.927548916689562,-9.9587097760858));
#71284=CARTESIAN_POINT('Ctrl Pts',(13.3375972579703,-6.34381077890256E-15,
-10.4873455314589));
#71285=CARTESIAN_POINT('Ctrl Pts',(12.6361849146756,-9.12101950322574,5.73249956259117));
#71286=CARTESIAN_POINT('Ctrl Pts',(12.9669648804042,-8.16824205056825,6.28258588136077));
#71287=CARTESIAN_POINT('Ctrl Pts',(13.3920458446166,-6.48443612385918,7.25473168640934));
#71288=CARTESIAN_POINT('Ctrl Pts',(13.5259820957649,-3.8118564888613,8.79774625810608));
#71289=CARTESIAN_POINT('Ctrl Pts',(13.1323548632684,-1.83314667576049,9.94015490134798));
#71290=CARTESIAN_POINT('Ctrl Pts',(12.6361849146756,-0.403980496774266,
10.7652843795024));
#71291=CARTESIAN_POINT('Ctrl Pts',(12.8699890291072,-9.10811555165336,5.56955729697059));
#71292=CARTESIAN_POINT('Ctrl Pts',(13.2078467774138,-8.14804366490556,6.12628217974948));
#71293=CARTESIAN_POINT('Ctrl Pts',(13.6453803397493,-6.4447365517833,7.11403939432885));
#71294=CARTESIAN_POINT('Ctrl Pts',(13.7845689781422,-3.72407315433307,8.68667090248933));
#71295=CARTESIAN_POINT('Ctrl Pts',(13.3767756515671,-1.71258108335183,9.84301179383112));
#71296=CARTESIAN_POINT('Ctrl Pts',(12.8699890291072,-0.269320331182843,
10.6726380968212));
#71297=CARTESIAN_POINT('Ctrl Pts',(13.1037931435388,-9.09521160008098,5.40661503135001));
#71298=CARTESIAN_POINT('Ctrl Pts',(13.4487286744235,-8.12784527924288,5.96997847813818));
#71299=CARTESIAN_POINT('Ctrl Pts',(13.898714834882,-6.40503697970743,6.97334710224837));
#71300=CARTESIAN_POINT('Ctrl Pts',(14.0431558605194,-3.63628981980485,8.57559554687257));
#71301=CARTESIAN_POINT('Ctrl Pts',(13.6211964398659,-1.59201549094317,9.74586868631425));
#71302=CARTESIAN_POINT('Ctrl Pts',(13.1037931435388,-0.13466016559142,10.57999181414));
#71303=CARTESIAN_POINT('Ctrl Pts',(13.3375972579703,-9.0823076485086,5.24367276572943));
#71304=CARTESIAN_POINT('Ctrl Pts',(13.6896105714332,-8.1076468935802,5.81367477652688));
#71305=CARTESIAN_POINT('Ctrl Pts',(14.1520493300147,-6.36533740763156,6.83265481016789));
#71306=CARTESIAN_POINT('Ctrl Pts',(14.3017427428967,-3.54850648527663,8.46452019125581));
#71307=CARTESIAN_POINT('Ctrl Pts',(13.8656172281646,-1.4714498985345,9.64872557879739));
#71308=CARTESIAN_POINT('Ctrl Pts',(13.3375972579703,2.97082320207775E-15,
10.4873455314589));
#71309=CARTESIAN_POINT('',(12.6462384144175,-0.433012701889492,10.7485226280639));
#71310=CARTESIAN_POINT('Ctrl Pts',(12.6462384144175,-0.43301270188949,10.7485226280639));
#71311=CARTESIAN_POINT('Ctrl Pts',(12.7615608863277,-0.360987847682757,
10.704956846462));
#71312=CARTESIAN_POINT('Ctrl Pts',(12.8768443884298,-0.288885377694372,
10.6614057866234));
#71313=CARTESIAN_POINT('Ctrl Pts',(13.1072956816033,-0.144548821365988,
10.5743473795151));
#71314=CARTESIAN_POINT('Ctrl Pts',(13.2224686011745,-0.0723115712969127,
10.5308380948337));
#71315=CARTESIAN_POINT('Ctrl Pts',(13.3375972579703,2.97082320207775E-15,
10.4873455314589));
#71316=CARTESIAN_POINT('',(12.6462384144167,-9.09198729810778,5.74926131403119));
#71317=CARTESIAN_POINT('Ctrl Pts',(12.6462405439409,-0.433014589688018,
10.748521538143));
#71318=CARTESIAN_POINT('Ctrl Pts',(13.1355491140165,-1.84924327825184,9.93086152356656));
#71319=CARTESIAN_POINT('Ctrl Pts',(13.5255929401103,-3.81962174635166,8.79326298460369));
#71320=CARTESIAN_POINT('Ctrl Pts',(13.3924350002713,-6.47667086636819,7.25921495991209));
#71321=CARTESIAN_POINT('Ctrl Pts',(12.9712786667837,-8.15112288573676,6.29246963578453));
#71322=CARTESIAN_POINT('Ctrl Pts',(12.6462397169624,-9.09198644037501,5.74926180924343));
#71323=CARTESIAN_POINT('Ctrl Pts',(13.3375972579703,-9.0823076485086,5.24367276572943));
#71324=CARTESIAN_POINT('Ctrl Pts',(13.2224673861609,-9.08381754355231,5.32804359554874));
#71325=CARTESIAN_POINT('Ctrl Pts',(13.1072932506156,-9.08537908137654,5.41235842078712));
#71326=CARTESIAN_POINT('Ctrl Pts',(12.8768419556905,-9.08860559755739,5.58088674636916));
#71327=CARTESIAN_POINT('Ctrl Pts',(12.7615596695584,-9.0902706697197,5.66510395773964));
#71328=CARTESIAN_POINT('Ctrl Pts',(12.6462384144189,-9.09198729810631,5.74926131403204));
#71329=CARTESIAN_POINT('Origin',(14.3,0.,0.));
#71330=CARTESIAN_POINT('',(14.3,-7.1,8.69499227394621E-16));
#71331=CARTESIAN_POINT('Origin',(14.3,0.,0.));
#71332=CARTESIAN_POINT('Origin',(3.,-9.025,5.21058617943637));
#71333=CARTESIAN_POINT('',(3.5,-9.09198729810778,5.74926131403119));
#71334=CARTESIAN_POINT('',(3.5,-9.525,4.99926131403119));
#71335=CARTESIAN_POINT('',(3.5,-9.09198729810778,5.74926131403119));
#71336=CARTESIAN_POINT('',(3.,-9.025,5.21058617943637));
#71337=CARTESIAN_POINT('',(3.,-9.025,5.21058617943637));
#71338=CARTESIAN_POINT('',(3.5,-9.525,4.99926131403119));
#71339=CARTESIAN_POINT('Origin',(3.,2.22044604925031E-15,10.4211723588727));
#71340=CARTESIAN_POINT('',(3.5,0.433012701892219,10.7485226280624));
#71341=CARTESIAN_POINT('',(3.5,-0.433012701892217,10.7485226280624));
#71342=CARTESIAN_POINT('',(3.5,0.433012701892221,10.7485226280624));
#71343=CARTESIAN_POINT('',(3.,3.60822483003176E-15,10.4211723588727));
#71344=CARTESIAN_POINT('',(3.,2.22044604925031E-15,10.4211723588727));
#71345=CARTESIAN_POINT('',(3.5,-0.433012701892217,10.7485226280624));
#71346=CARTESIAN_POINT('Origin',(3.,-9.025,-5.21058617943637));
#71347=CARTESIAN_POINT('',(3.5,-9.525,-4.99926131403118));
#71348=CARTESIAN_POINT('',(3.5,-9.09198729810778,-5.74926131403119));
#71349=CARTESIAN_POINT('',(3.5,-9.525,-4.99926131403118));
#71350=CARTESIAN_POINT('',(3.,-9.025,-5.21058617943637));
#71351=CARTESIAN_POINT('',(3.,-9.025,-5.21058617943637));
#71352=CARTESIAN_POINT('',(3.5,-9.09198729810778,-5.74926131403119));
#71353=CARTESIAN_POINT('Origin',(3.25,-9.275,2.74963065701559));
#71354=CARTESIAN_POINT('',(3.5,-9.525,2.74963065701559));
#71355=CARTESIAN_POINT('',(3.,-9.025,2.74963065701559));
#71356=CARTESIAN_POINT('Origin',(12.6462384144175,-9.525,4.99926131403433));
#71357=CARTESIAN_POINT('',(12.6462384144167,-9.525,4.99926131403119));
#71358=CARTESIAN_POINT('Origin',(3.,9.025,5.21058617943637));
#71359=CARTESIAN_POINT('',(3.5,9.525,4.99926131403119));
#71360=CARTESIAN_POINT('',(3.5,9.09198729810778,5.74926131403119));
#71361=CARTESIAN_POINT('',(3.5,9.525,4.99926131403119));
#71362=CARTESIAN_POINT('',(3.,9.025,5.21058617943637));
#71363=CARTESIAN_POINT('',(3.,9.025,5.21058617943637));
#71364=CARTESIAN_POINT('',(3.5,9.09198729810778,5.74926131403119));
#71365=CARTESIAN_POINT('Origin',(13.3375972579703,6.4216470683267E-16,10.4873455314589));
#71366=CARTESIAN_POINT('',(12.6462384144167,0.433012701892221,10.7485226280624));
#71367=CARTESIAN_POINT('Ctrl Pts',(13.3375972579703,7.6281401925679E-15,
10.4873455314589));
#71368=CARTESIAN_POINT('Ctrl Pts',(13.2224673861555,0.0723123344434218,
10.5308385538355));
#71369=CARTESIAN_POINT('Ctrl Pts',(13.1072932506048,0.14455034610674,10.5743482978814));
#71370=CARTESIAN_POINT('Ctrl Pts',(12.8768419556913,0.288886899220415,10.6614067056464));
#71371=CARTESIAN_POINT('Ctrl Pts',(12.7615596695601,0.36098860762136,10.704957306123));
#71372=CARTESIAN_POINT('Ctrl Pts',(12.6462384144189,0.433012701893687,10.7485226280615));
#71373=CARTESIAN_POINT('',(12.6462384144167,-0.433012701892217,10.7485226280624));
#71374=CARTESIAN_POINT('Origin',(3.,0.,-10.4211723588727));
#71375=CARTESIAN_POINT('',(3.5,-0.433012701892219,-10.7485226280624));
#71376=CARTESIAN_POINT('',(3.5,0.433012701892217,-10.7485226280624));
#71377=CARTESIAN_POINT('',(3.5,-0.433012701892221,-10.7485226280624));
#71378=CARTESIAN_POINT('',(3.,-1.38777878078145E-15,-10.4211723588727));
#71379=CARTESIAN_POINT('',(3.,0.,-10.4211723588727));
#71380=CARTESIAN_POINT('',(3.5,0.433012701892217,-10.7485226280624));
#71381=CARTESIAN_POINT('Origin',(3.25,-7.01875,-6.65757029159287));
#71382=CARTESIAN_POINT('',(3.5,-7.14375,-6.87407664253898));
#71383=CARTESIAN_POINT('',(3.,-6.89375,-6.44106394064676));
#71384=CARTESIAN_POINT('Origin',(12.6462384144175,-9.0919872981105,-5.74926131402961));
#71385=CARTESIAN_POINT('',(12.6462384144167,-9.09198729810778,-5.74926131403119));
#71386=CARTESIAN_POINT('Origin',(3.5,9.525,-4.99926131403119));
#71387=CARTESIAN_POINT('',(3.,9.025,-5.21058617943638));
#71388=CARTESIAN_POINT('',(3.5,9.09198729810778,-5.74926131403119));
#71389=CARTESIAN_POINT('',(3.,9.025,-5.21058617943638));
#71390=CARTESIAN_POINT('',(3.5,9.525,-4.99926131403119));
#71391=CARTESIAN_POINT('',(3.5,9.525,-4.99926131403119));
#71392=CARTESIAN_POINT('',(3.5,9.09198729810778,-5.74926131403119));
#71393=CARTESIAN_POINT('Origin',(3.25,9.275,-2.7496306570156));
#71394=CARTESIAN_POINT('',(3.5,9.525,-2.7496306570156));
#71395=CARTESIAN_POINT('',(3.,9.025,-2.7496306570156));
#71396=CARTESIAN_POINT('Origin',(13.3375972579703,9.08230764850859,5.24367276572943));
#71397=CARTESIAN_POINT('',(12.6462384144175,9.0919872981105,5.74926131402961));
#71398=CARTESIAN_POINT('Ctrl Pts',(12.6462384144175,9.09198729811051,5.74926131402961));
#71399=CARTESIAN_POINT('Ctrl Pts',(12.7615608863187,9.09027065161096,5.66510306978824));
#71400=CARTESIAN_POINT('Ctrl Pts',(12.8768443884255,9.08860556242314,5.58088496918004));
#71401=CARTESIAN_POINT('Ctrl Pts',(13.1072956816019,9.08537904841851,5.41235664114861));
#71402=CARTESIAN_POINT('Ctrl Pts',(13.2224686011735,9.08381752761848,5.32804270514828));
#71403=CARTESIAN_POINT('Ctrl Pts',(13.3375972579703,9.0823076485086,5.24367276572943));
#71404=CARTESIAN_POINT('',(12.6462384144167,9.525,4.99926131403119));
#71405=CARTESIAN_POINT('Ctrl Pts',(13.3375972579703,9.08230764850859,5.24367276572942));
#71406=CARTESIAN_POINT('Ctrl Pts',(13.2224673861562,9.15612987799533,5.20279495828302));
#71407=CARTESIAN_POINT('Ctrl Pts',(13.1072932506068,9.22992942748221,5.16198987708712));
#71408=CARTESIAN_POINT('Ctrl Pts',(12.8768419556941,9.37749249677602,5.08051995927881));
#71409=CARTESIAN_POINT('Ctrl Pts',(12.7615596695645,9.45125927733824,5.03985334838617));
#71410=CARTESIAN_POINT('Ctrl Pts',(12.6462384144189,9.525,4.99926131402949));
#71411=CARTESIAN_POINT('',(12.6462384144167,9.09198729810778,5.74926131403119));
#71412=CARTESIAN_POINT('Origin',(12.6462384144175,0.433012701889492,-10.7485226280639));
#71413=CARTESIAN_POINT('',(12.6462384144175,0.433012701889492,-10.7485226280639));
#71414=CARTESIAN_POINT('',(12.6462384144167,0.433012701892217,-10.7485226280624));
#71415=CARTESIAN_POINT('Ctrl Pts',(12.6462384144175,0.433012701889488,-10.7485226280639));
#71416=CARTESIAN_POINT('Ctrl Pts',(12.7615608863249,0.360987847684519,-10.704956846463));
#71417=CARTESIAN_POINT('Ctrl Pts',(12.8768443884286,0.288885377695135,-10.6614057866238));
#71418=CARTESIAN_POINT('Ctrl Pts',(13.1072956815852,0.144548821377305,-10.5743473795219));
#71419=CARTESIAN_POINT('Ctrl Pts',(13.2224686011646,0.0723115713031384,
-10.5308380948375));
#71420=CARTESIAN_POINT('Ctrl Pts',(13.3375972579703,-6.34381077890256E-15,
-10.4873455314589));
#71421=CARTESIAN_POINT('Origin',(13.3375972579703,9.08230764850859,-5.24367276572944));
#71422=CARTESIAN_POINT('',(12.6462384144175,9.525,-4.99926131403433));
#71423=CARTESIAN_POINT('Ctrl Pts',(12.6462384144175,9.525,-4.99926131403433));
#71424=CARTESIAN_POINT('Ctrl Pts',(12.7615608863322,9.45125849929071,-5.03985377668183));
#71425=CARTESIAN_POINT('Ctrl Pts',(12.8768443884316,9.37749094011633,-5.08052081744712));
#71426=CARTESIAN_POINT('Ctrl Pts',(13.1072956815797,9.22992786979956,-5.16199073835919));
#71427=CARTESIAN_POINT('Ctrl Pts',(13.2224686011626,9.15612909892297,-5.20279538968195));
#71428=CARTESIAN_POINT('Ctrl Pts',(13.3375972579703,9.08230764850859,-5.24367276572943));
#71429=CARTESIAN_POINT('',(12.6462384144167,9.09198729810778,-5.74926131403119));
#71430=CARTESIAN_POINT('Ctrl Pts',(13.3375972579703,9.08230764850859,-5.24367276572944));
#71431=CARTESIAN_POINT('Ctrl Pts',(13.2224673861615,9.08381754355229,-5.32804359554833));
#71432=CARTESIAN_POINT('Ctrl Pts',(13.1072932506172,9.08537908137651,-5.41235842078597));
#71433=CARTESIAN_POINT('Ctrl Pts',(12.8768419556896,9.0886055975574,-5.58088674636987));
#71434=CARTESIAN_POINT('Ctrl Pts',(12.7615596695564,9.09027066971973,-5.66510395774111));
#71435=CARTESIAN_POINT('Ctrl Pts',(12.6462384144189,9.09198729810631,-5.74926131403204));
#71436=CARTESIAN_POINT('',(12.6462384144167,9.525,-4.99926131403119));
#71437=CARTESIAN_POINT('Ctrl Pts',(12.6361849146757,9.12101950322573,-5.73249956259117));
#71438=CARTESIAN_POINT('Ctrl Pts',(12.9669648804042,8.16824205056824,-6.28258588136078));
#71439=CARTESIAN_POINT('Ctrl Pts',(13.3920458446166,6.48443612385917,-7.25473168640934));
#71440=CARTESIAN_POINT('Ctrl Pts',(13.5259820957649,3.81185648886129,-8.79774625810609));
#71441=CARTESIAN_POINT('Ctrl Pts',(13.1323548632684,1.83314667576048,-9.94015490134799));
#71442=CARTESIAN_POINT('Ctrl Pts',(12.6361849146757,0.403980496774259,-10.7652843795024));
#71443=CARTESIAN_POINT('Ctrl Pts',(12.8699890291072,9.10811555165335,-5.5695572969706));
#71444=CARTESIAN_POINT('Ctrl Pts',(13.2078467774138,8.14804366490556,-6.12628217974948));
#71445=CARTESIAN_POINT('Ctrl Pts',(13.6453803397493,6.4447365517833,-7.11403939432886));
#71446=CARTESIAN_POINT('Ctrl Pts',(13.7845689781422,3.72407315433307,-8.68667090248933));
#71447=CARTESIAN_POINT('Ctrl Pts',(13.3767756515671,1.71258108335182,-9.84301179383112));
#71448=CARTESIAN_POINT('Ctrl Pts',(12.8699890291072,0.269320331182837,-10.6726380968212));
#71449=CARTESIAN_POINT('Ctrl Pts',(13.1037931435388,9.09521160008097,-5.40661503135002));
#71450=CARTESIAN_POINT('Ctrl Pts',(13.4487286744235,8.12784527924288,-5.96997847813819));
#71451=CARTESIAN_POINT('Ctrl Pts',(13.898714834882,6.40503697970743,-6.97334710224838));
#71452=CARTESIAN_POINT('Ctrl Pts',(14.0431558605194,3.63628981980484,-8.57559554687257));
#71453=CARTESIAN_POINT('Ctrl Pts',(13.6211964398659,1.59201549094316,-9.74586868631426));
#71454=CARTESIAN_POINT('Ctrl Pts',(13.1037931435388,0.134660165591415,-10.57999181414));
#71455=CARTESIAN_POINT('Ctrl Pts',(13.3375972579703,9.08230764850859,-5.24367276572944));
#71456=CARTESIAN_POINT('Ctrl Pts',(13.6896105714332,8.10764689358019,-5.81367477652689));
#71457=CARTESIAN_POINT('Ctrl Pts',(14.1520493300147,6.36533740763156,-6.83265481016789));
#71458=CARTESIAN_POINT('Ctrl Pts',(14.3017427428967,3.54850648527662,-8.46452019125581));
#71459=CARTESIAN_POINT('Ctrl Pts',(13.8656172281646,1.47144989853449,-9.64872557879739));
#71460=CARTESIAN_POINT('Ctrl Pts',(13.3375972579703,-6.34381077890256E-15,
-10.4873455314589));
#71461=CARTESIAN_POINT('Ctrl Pts',(12.6462405439409,0.433014589688015,-10.748521538143));
#71462=CARTESIAN_POINT('Ctrl Pts',(13.1355491140165,1.84924327825183,-9.93086152356657));
#71463=CARTESIAN_POINT('Ctrl Pts',(13.5255929401103,3.81962174635166,-8.7932629846037));
#71464=CARTESIAN_POINT('Ctrl Pts',(13.3924350002713,6.47667086636819,-7.25921495991209));
#71465=CARTESIAN_POINT('Ctrl Pts',(12.9712786667837,8.15112288573676,-6.29246963578454));
#71466=CARTESIAN_POINT('Ctrl Pts',(12.6462397169624,9.09198644037501,-5.74926180924343));
#71467=CARTESIAN_POINT('Origin',(3.,9.30849364905389,-5.37426131403119));
#71468=CARTESIAN_POINT('',(3.,9.09198729810778,-5.74926131403119));
#71469=CARTESIAN_POINT('',(3.,9.525,-4.99926131403119));
#71470=CARTESIAN_POINT('Ctrl Pts',(12.6361849146757,9.525,5.03278481691122));
#71471=CARTESIAN_POINT('Ctrl Pts',(13.1323548632684,9.525,3.3825258606024));
#71472=CARTESIAN_POINT('Ctrl Pts',(13.5261795528199,9.525,1.0975656251991));
#71473=CARTESIAN_POINT('Ctrl Pts',(13.3921464946308,9.525,-1.98832724851366));
#71474=CARTESIAN_POINT('Ctrl Pts',(12.9669648804042,9.525,-3.93261217937201));
#71475=CARTESIAN_POINT('Ctrl Pts',(12.6361849146756,9.525,-5.03278481691123));
#71476=CARTESIAN_POINT('Ctrl Pts',(12.8699890291072,9.3774358828362,5.10308079985062));
#71477=CARTESIAN_POINT('Ctrl Pts',(13.3767756515671,9.3805888048835,3.43836717269219));
#71478=CARTESIAN_POINT('Ctrl Pts',(13.7847648925596,9.38491352314619,1.11803995403544));
#71479=CARTESIAN_POINT('Ctrl Pts',(13.6454811073302,9.38330701946683,-2.02429453530628));
#71480=CARTESIAN_POINT('Ctrl Pts',(13.2078467774138,9.37953783086773,-3.99327171507834));
#71481=CARTESIAN_POINT('Ctrl Pts',(12.8699890291072,9.3774358828362,-5.10308079985063));
#71482=CARTESIAN_POINT('Ctrl Pts',(13.1037931435388,9.2298717656724,5.17337678279002));
#71483=CARTESIAN_POINT('Ctrl Pts',(13.6211964398659,9.236177609767,3.49420848478198));
#71484=CARTESIAN_POINT('Ctrl Pts',(14.0433502322992,9.24482704629237,1.13851428287177));
#71485=CARTESIAN_POINT('Ctrl Pts',(13.8988157200297,9.24161403893366,-2.06026182209891));
#71486=CARTESIAN_POINT('Ctrl Pts',(13.4487286744235,9.23407566173546,-4.05393125078467));
#71487=CARTESIAN_POINT('Ctrl Pts',(13.1037931435388,9.22987176567239,-5.17337678279004));
#71488=CARTESIAN_POINT('Ctrl Pts',(13.3375972579703,9.08230764850859,5.24367276572943));
#71489=CARTESIAN_POINT('Ctrl Pts',(13.8656172281646,9.0917664146505,3.55004979687177));
#71490=CARTESIAN_POINT('Ctrl Pts',(14.3019355720389,9.10474056943856,1.15898861170811));
#71491=CARTESIAN_POINT('Ctrl Pts',(14.1521503327292,9.09992105840049,-2.09622910889154));
#71492=CARTESIAN_POINT('Ctrl Pts',(13.6896105714332,9.0886134926032,-4.114590786491));
#71493=CARTESIAN_POINT('Ctrl Pts',(13.3375972579703,9.08230764850859,-5.24367276572944));
#71494=CARTESIAN_POINT('Ctrl Pts',(12.64623973251,9.525,-4.99926032466067));
#71495=CARTESIAN_POINT('Ctrl Pts',(12.9712796891567,9.525,-3.91284474029011));
#71496=CARTESIAN_POINT('Ctrl Pts',(13.3925359315611,9.525,-1.97936109744437));
#71497=CARTESIAN_POINT('Ctrl Pts',(13.5257901158896,9.525,1.08859947412911));
#71498=CARTESIAN_POINT('Ctrl Pts',(13.1355507160135,9.525,3.36393794605573));
#71499=CARTESIAN_POINT('Ctrl Pts',(12.646240560211,9.525,4.99925912241684));
#71500=CARTESIAN_POINT('Origin',(3.,-1.83880688453542E-15,-10.7485226280624));
#71501=CARTESIAN_POINT('',(3.,-0.433012701892221,-10.7485226280624));
#71502=CARTESIAN_POINT('',(3.,0.433012701892217,-10.7485226280624));
#71503=CARTESIAN_POINT('Origin',(3.,9.30849364905389,5.37426131403119));
#71504=CARTESIAN_POINT('',(3.,9.525,4.99926131403119));
#71505=CARTESIAN_POINT('',(3.,9.09198729810778,5.74926131403119));
#71506=CARTESIAN_POINT('Ctrl Pts',(12.6361849146757,0.403980496774264,10.7652843795024));
#71507=CARTESIAN_POINT('Ctrl Pts',(13.1323548632684,1.83314667576049,9.94015490134798));
#71508=CARTESIAN_POINT('Ctrl Pts',(13.5259820957649,3.8118564888613,8.79774625810608));
#71509=CARTESIAN_POINT('Ctrl Pts',(13.3920458446166,6.48443612385918,7.25473168640934));
#71510=CARTESIAN_POINT('Ctrl Pts',(12.9669648804042,8.16824205056825,6.28258588136077));
#71511=CARTESIAN_POINT('Ctrl Pts',(12.6361849146756,9.12101950322573,5.73249956259117));
#71512=CARTESIAN_POINT('Ctrl Pts',(12.8699890291072,0.269320331182843,10.6726380968212));
#71513=CARTESIAN_POINT('Ctrl Pts',(13.3767756515671,1.71258108335183,9.84301179383112));
#71514=CARTESIAN_POINT('Ctrl Pts',(13.7845689781422,3.72407315433307,8.68667090248932));
#71515=CARTESIAN_POINT('Ctrl Pts',(13.6453803397493,6.44473655178331,7.11403939432886));
#71516=CARTESIAN_POINT('Ctrl Pts',(13.2078467774138,8.14804366490557,6.12628217974947));
#71517=CARTESIAN_POINT('Ctrl Pts',(12.8699890291072,9.10811555165335,5.56955729697059));
#71518=CARTESIAN_POINT('Ctrl Pts',(13.1037931435388,0.134660165591422,10.57999181414));
#71519=CARTESIAN_POINT('Ctrl Pts',(13.6211964398659,1.59201549094317,9.74586868631426));
#71520=CARTESIAN_POINT('Ctrl Pts',(14.0431558605194,3.63628981980485,8.57559554687256));
#71521=CARTESIAN_POINT('Ctrl Pts',(13.898714834882,6.40503697970744,6.97334710224837));
#71522=CARTESIAN_POINT('Ctrl Pts',(13.4487286744235,8.12784527924288,5.96997847813818));
#71523=CARTESIAN_POINT('Ctrl Pts',(13.1037931435388,9.09521160008098,5.40661503135001));
#71524=CARTESIAN_POINT('Ctrl Pts',(13.3375972579703,6.4216470683267E-16,
10.4873455314589));
#71525=CARTESIAN_POINT('Ctrl Pts',(13.8656172281646,1.4714498985345,9.64872557879739));
#71526=CARTESIAN_POINT('Ctrl Pts',(14.3017427428967,3.54850648527663,8.4645201912558));
#71527=CARTESIAN_POINT('Ctrl Pts',(14.1520493300147,6.36533740763157,6.83265481016789));
#71528=CARTESIAN_POINT('Ctrl Pts',(13.6896105714332,8.1076468935802,5.81367477652688));
#71529=CARTESIAN_POINT('Ctrl Pts',(13.3375972579703,9.0823076485086,5.24367276572943));
#71530=CARTESIAN_POINT('Ctrl Pts',(12.6462397169616,9.09198644037732,5.7492618092421));
#71531=CARTESIAN_POINT('Ctrl Pts',(12.9712786667833,8.15112288573813,6.29246963578374));
#71532=CARTESIAN_POINT('Ctrl Pts',(13.3924350002713,6.47667086636881,7.25921495991173));
#71533=CARTESIAN_POINT('Ctrl Pts',(13.5255929401102,3.81962174635229,8.79326298460333));
#71534=CARTESIAN_POINT('Ctrl Pts',(13.1355491140168,1.84924327825312,9.93086152356583));
#71535=CARTESIAN_POINT('Ctrl Pts',(12.6462405439417,0.433014589690331,10.7485215381416));
#71536=CARTESIAN_POINT('Origin',(3.25,2.25625,-9.40720094860847));
#71537=CARTESIAN_POINT('',(3.5,2.38125,-9.62370729955458));
#71538=CARTESIAN_POINT('',(3.,2.13125,-9.19069459766236));
#71539=CARTESIAN_POINT('Origin',(3.,-9.30849364905389,-5.37426131403119));
#71540=CARTESIAN_POINT('',(3.,-9.525,-4.99926131403118));
#71541=CARTESIAN_POINT('',(3.,-9.09198729810778,-5.74926131403119));
#71542=CARTESIAN_POINT('Origin',(3.,2.0122792321331E-15,10.7485226280624));
#71543=CARTESIAN_POINT('',(3.,0.433012701892221,10.7485226280624));
#71544=CARTESIAN_POINT('',(3.,-0.433012701892217,10.7485226280624));
#71545=CARTESIAN_POINT('Origin',(3.25,7.01875,6.65757029159287));
#71546=CARTESIAN_POINT('',(3.5,7.14375,6.87407664253898));
#71547=CARTESIAN_POINT('',(3.,6.89375,6.44106394064676));
#71548=CARTESIAN_POINT('Origin',(3.,-9.30849364905389,5.37426131403119));
#71549=CARTESIAN_POINT('',(3.,-9.09198729810778,5.74926131403119));
#71550=CARTESIAN_POINT('',(3.,-9.525,4.99926131403119));
#71551=CARTESIAN_POINT('Origin',(3.25,-2.25625,9.40720094860847));
#71552=CARTESIAN_POINT('',(3.5,-2.38125,9.62370729955457));
#71553=CARTESIAN_POINT('',(3.,-2.13125,9.19069459766235));
#71554=CARTESIAN_POINT('Origin',(3.,9.525,-5.49926131403119));
#71555=CARTESIAN_POINT('Origin',(3.,0.,0.));
#71556=CARTESIAN_POINT('',(3.,-8.925,-1.09299726823901E-15));
#71557=CARTESIAN_POINT('Origin',(3.,0.,0.));
#71558=CARTESIAN_POINT('Origin',(3.,-2.02039582977095E-15,-10.9985226280624));
#71559=CARTESIAN_POINT('Origin',(3.,-9.525,-5.49926131403119));
#71560=CARTESIAN_POINT('Origin',(3.,9.525,5.49926131403119));
#71561=CARTESIAN_POINT('Origin',(3.,-9.525,5.49926131403119));
#71562=CARTESIAN_POINT('Origin',(3.,6.73465276590316E-16,10.9985226280624));
#71563=CARTESIAN_POINT('Origin',(14.,0.,0.));
#71564=CARTESIAN_POINT('',(13.6,-6.4,-7.83773951454306E-16));
#71565=CARTESIAN_POINT('',(13.6,-7.83773951454306E-16,6.4));
#71566=CARTESIAN_POINT('Origin',(13.6,0.,0.));
#71567=CARTESIAN_POINT('',(14.,-6.8,-8.327598234202E-16));
#71568=CARTESIAN_POINT('Origin',(13.6,0.,0.));
#71569=CARTESIAN_POINT('Origin',(2.,0.,0.));
#71570=CARTESIAN_POINT('',(2.77555756156289E-16,-7.2,-8.81745695386094E-16));
#71571=CARTESIAN_POINT('',(2.,-8.35,-1.02258007728804E-15));
#71572=CARTESIAN_POINT('Origin',(0.,0.,0.));
#71573=CARTESIAN_POINT('Origin',(0.,7.2,0.));
#71574=CARTESIAN_POINT('',(0.,-7.83773951454306E-16,6.4));
#71575=CARTESIAN_POINT('Origin',(0.,0.,0.));
#71576=CARTESIAN_POINT('Origin',(3.,0.,0.));
#71577=CARTESIAN_POINT('',(3.,-7.83773951454306E-16,6.4));
#71578=CARTESIAN_POINT('',(0.,0.,0.));
#71579=CARTESIAN_POINT('',(0.,0.,0.));
#71580=CARTESIAN_POINT('',(5.5,2.40741243048398E-34,3.46944695195361E-17));
#71581=CARTESIAN_POINT('',(31.9399999999999,0.,0.));
#71582=CARTESIAN_POINT('',(31.94,0.,0.));
#71583=CARTESIAN_POINT('',(80.,0.,0.));
#71584=CARTESIAN_POINT('',(80.,0.,0.));
#71585=CARTESIAN_POINT('',(94.25,0.,0.));
#71586=CARTESIAN_POINT('',(96.7,0.,0.));
#71587=CARTESIAN_POINT('',(0.,0.,0.));
#71588=CARTESIAN_POINT('',(105.,0.,0.));
#71589=CARTESIAN_POINT('',(61.9999999999999,1.83936199604773E-14,57.1499999999999));
#71590=CARTESIAN_POINT('',(86.35,9.20597457513686E-15,57.1499999999999));
#71591=CARTESIAN_POINT('',(62.,-54.352879906268,17.6603212285283));
#71592=CARTESIAN_POINT('',(86.35,-54.3528799062679,17.6603212285283));
#71593=CARTESIAN_POINT('',(62.,-33.5919271685149,-46.2353212285282));
#71594=CARTESIAN_POINT('',(86.35,-33.5919271685149,-46.2353212285282));
#71595=CARTESIAN_POINT('',(62.,33.5919271685148,-46.2353212285282));
#71596=CARTESIAN_POINT('',(86.35,33.5919271685149,-46.2353212285282));
#71597=CARTESIAN_POINT('',(61.9999999999999,54.352879906268,17.6603212285283));
#71598=CARTESIAN_POINT('',(86.35,54.3528799062679,17.6603212285282));
#71599=UNCERTAINTY_MEASURE_WITH_UNIT(LENGTH_MEASURE(0.01),#71629,
'DISTANCE_ACCURACY_VALUE',
'Maximum model space distance between geometric entities at asserted c
onnectivities');
#71600=UNCERTAINTY_MEASURE_WITH_UNIT(LENGTH_MEASURE(0.01),#71629,
'DISTANCE_ACCURACY_VALUE',
'Maximum model space distance between geometric entities at asserted c
onnectivities');
#71601=UNCERTAINTY_MEASURE_WITH_UNIT(LENGTH_MEASURE(0.01),#71629,
'DISTANCE_ACCURACY_VALUE',
'Maximum model space distance between geometric entities at asserted c
onnectivities');
#71602=UNCERTAINTY_MEASURE_WITH_UNIT(LENGTH_MEASURE(0.01),#71629,
'DISTANCE_ACCURACY_VALUE',
'Maximum model space distance between geometric entities at asserted c
onnectivities');
#71603=UNCERTAINTY_MEASURE_WITH_UNIT(LENGTH_MEASURE(0.01),#71629,
'DISTANCE_ACCURACY_VALUE',
'Maximum model space distance between geometric entities at asserted c
onnectivities');
#71604=UNCERTAINTY_MEASURE_WITH_UNIT(LENGTH_MEASURE(0.01),#71629,
'DISTANCE_ACCURACY_VALUE',
'Maximum model space distance between geometric entities at asserted c
onnectivities');
#71605=UNCERTAINTY_MEASURE_WITH_UNIT(LENGTH_MEASURE(0.01),#71629,
'DISTANCE_ACCURACY_VALUE',
'Maximum model space distance between geometric entities at asserted c
onnectivities');
#71606=UNCERTAINTY_MEASURE_WITH_UNIT(LENGTH_MEASURE(0.01),#71629,
'DISTANCE_ACCURACY_VALUE',
'Maximum model space distance between geometric entities at asserted c
onnectivities');
#71607=UNCERTAINTY_MEASURE_WITH_UNIT(LENGTH_MEASURE(0.01),#71629,
'DISTANCE_ACCURACY_VALUE',
'Maximum model space distance between geometric entities at asserted c
onnectivities');
#71608=UNCERTAINTY_MEASURE_WITH_UNIT(LENGTH_MEASURE(0.01),#71629,
'DISTANCE_ACCURACY_VALUE',
'Maximum model space distance between geometric entities at asserted c
onnectivities');
#71609=UNCERTAINTY_MEASURE_WITH_UNIT(LENGTH_MEASURE(0.01),#71629,
'DISTANCE_ACCURACY_VALUE',
'Maximum model space distance between geometric entities at asserted c
onnectivities');
#71610=UNCERTAINTY_MEASURE_WITH_UNIT(LENGTH_MEASURE(0.01),#71629,
'DISTANCE_ACCURACY_VALUE',
'Maximum model space distance between geometric entities at asserted c
onnectivities');
#71611=UNCERTAINTY_MEASURE_WITH_UNIT(LENGTH_MEASURE(0.01),#71629,
'DISTANCE_ACCURACY_VALUE',
'Maximum model space distance between geometric entities at asserted c
onnectivities');
#71612=UNCERTAINTY_MEASURE_WITH_UNIT(LENGTH_MEASURE(0.01),#71629,
'DISTANCE_ACCURACY_VALUE',
'Maximum model space distance between geometric entities at asserted c
onnectivities');
#71613=UNCERTAINTY_MEASURE_WITH_UNIT(LENGTH_MEASURE(0.01),#71629,
'DISTANCE_ACCURACY_VALUE',
'Maximum model space distance between geometric entities at asserted c
onnectivities');
#71614=(
GEOMETRIC_REPRESENTATION_CONTEXT(3)
GLOBAL_UNCERTAINTY_ASSIGNED_CONTEXT((#71599))
GLOBAL_UNIT_ASSIGNED_CONTEXT((#71629,#71631,#71632))
REPRESENTATION_CONTEXT('','3D')
);
#71615=(
GEOMETRIC_REPRESENTATION_CONTEXT(3)
GLOBAL_UNCERTAINTY_ASSIGNED_CONTEXT((#71600))
GLOBAL_UNIT_ASSIGNED_CONTEXT((#71629,#71631,#71632))
REPRESENTATION_CONTEXT('','3D')
);
#71616=(
GEOMETRIC_REPRESENTATION_CONTEXT(3)
GLOBAL_UNCERTAINTY_ASSIGNED_CONTEXT((#71601))
GLOBAL_UNIT_ASSIGNED_CONTEXT((#71629,#71631,#71632))
REPRESENTATION_CONTEXT('','3D')
);
#71617=(
GEOMETRIC_REPRESENTATION_CONTEXT(3)
GLOBAL_UNCERTAINTY_ASSIGNED_CONTEXT((#71602))
GLOBAL_UNIT_ASSIGNED_CONTEXT((#71629,#71631,#71632))
REPRESENTATION_CONTEXT('','3D')
);
#71618=(
GEOMETRIC_REPRESENTATION_CONTEXT(3)
GLOBAL_UNCERTAINTY_ASSIGNED_CONTEXT((#71603))
GLOBAL_UNIT_ASSIGNED_CONTEXT((#71629,#71631,#71632))
REPRESENTATION_CONTEXT('','3D')
);
#71619=(
GEOMETRIC_REPRESENTATION_CONTEXT(3)
GLOBAL_UNCERTAINTY_ASSIGNED_CONTEXT((#71604))
GLOBAL_UNIT_ASSIGNED_CONTEXT((#71629,#71631,#71632))
REPRESENTATION_CONTEXT('','3D')
);
#71620=(
GEOMETRIC_REPRESENTATION_CONTEXT(3)
GLOBAL_UNCERTAINTY_ASSIGNED_CONTEXT((#71605))
GLOBAL_UNIT_ASSIGNED_CONTEXT((#71629,#71631,#71632))
REPRESENTATION_CONTEXT('','3D')
);
#71621=(
GEOMETRIC_REPRESENTATION_CONTEXT(3)
GLOBAL_UNCERTAINTY_ASSIGNED_CONTEXT((#71606))
GLOBAL_UNIT_ASSIGNED_CONTEXT((#71629,#71631,#71632))
REPRESENTATION_CONTEXT('','3D')
);
#71622=(
GEOMETRIC_REPRESENTATION_CONTEXT(3)
GLOBAL_UNCERTAINTY_ASSIGNED_CONTEXT((#71607))
GLOBAL_UNIT_ASSIGNED_CONTEXT((#71629,#71631,#71632))
REPRESENTATION_CONTEXT('','3D')
);
#71623=(
GEOMETRIC_REPRESENTATION_CONTEXT(3)
GLOBAL_UNCERTAINTY_ASSIGNED_CONTEXT((#71608))
GLOBAL_UNIT_ASSIGNED_CONTEXT((#71629,#71631,#71632))
REPRESENTATION_CONTEXT('','3D')
);
#71624=(
GEOMETRIC_REPRESENTATION_CONTEXT(3)
GLOBAL_UNCERTAINTY_ASSIGNED_CONTEXT((#71609))
GLOBAL_UNIT_ASSIGNED_CONTEXT((#71629,#71631,#71632))
REPRESENTATION_CONTEXT('','3D')
);
#71625=(
GEOMETRIC_REPRESENTATION_CONTEXT(3)
GLOBAL_UNCERTAINTY_ASSIGNED_CONTEXT((#71610))
GLOBAL_UNIT_ASSIGNED_CONTEXT((#71629,#71631,#71632))
REPRESENTATION_CONTEXT('','3D')
);
#71626=(
GEOMETRIC_REPRESENTATION_CONTEXT(3)
GLOBAL_UNCERTAINTY_ASSIGNED_CONTEXT((#71611))
GLOBAL_UNIT_ASSIGNED_CONTEXT((#71629,#71631,#71632))
REPRESENTATION_CONTEXT('','3D')
);
#71627=(
GEOMETRIC_REPRESENTATION_CONTEXT(3)
GLOBAL_UNCERTAINTY_ASSIGNED_CONTEXT((#71612))
GLOBAL_UNIT_ASSIGNED_CONTEXT((#71629,#71631,#71632))
REPRESENTATION_CONTEXT('','3D')
);
#71628=(
GEOMETRIC_REPRESENTATION_CONTEXT(3)
GLOBAL_UNCERTAINTY_ASSIGNED_CONTEXT((#71613))
GLOBAL_UNIT_ASSIGNED_CONTEXT((#71629,#71631,#71632))
REPRESENTATION_CONTEXT('','3D')
);
#71629=(
LENGTH_UNIT()
NAMED_UNIT(*)
SI_UNIT(.MILLI.,.METRE.)
);
#71630=(
LENGTH_UNIT()
NAMED_UNIT(*)
SI_UNIT($,.METRE.)
);
#71631=(
NAMED_UNIT(*)
PLANE_ANGLE_UNIT()
SI_UNIT($,.RADIAN.)
);
#71632=(
NAMED_UNIT(*)
SI_UNIT($,.STERADIAN.)
SOLID_ANGLE_UNIT()
);
#71633=SHAPE_DEFINITION_REPRESENTATION(#71647,#71682);
#71634=SHAPE_DEFINITION_REPRESENTATION(#71648,#71683);
#71635=SHAPE_DEFINITION_REPRESENTATION(#71649,#71684);
#71636=SHAPE_DEFINITION_REPRESENTATION(#71650,#71685);
#71637=SHAPE_DEFINITION_REPRESENTATION(#71651,#71686);
#71638=SHAPE_DEFINITION_REPRESENTATION(#71652,#71687);
#71639=SHAPE_DEFINITION_REPRESENTATION(#71653,#71688);
#71640=SHAPE_DEFINITION_REPRESENTATION(#71654,#71689);
#71641=SHAPE_DEFINITION_REPRESENTATION(#71655,#71690);
#71642=SHAPE_DEFINITION_REPRESENTATION(#71656,#71691);
#71643=SHAPE_DEFINITION_REPRESENTATION(#71657,#71692);
#71644=SHAPE_DEFINITION_REPRESENTATION(#71658,#71693);
#71645=SHAPE_DEFINITION_REPRESENTATION(#71659,#71694);
#71646=SHAPE_DEFINITION_REPRESENTATION(#71660,#71695);
#71647=PRODUCT_DEFINITION_SHAPE('',$,#71697);
#71648=PRODUCT_DEFINITION_SHAPE('',$,#71698);
#71649=PRODUCT_DEFINITION_SHAPE('',$,#71699);
#71650=PRODUCT_DEFINITION_SHAPE('',$,#71700);
#71651=PRODUCT_DEFINITION_SHAPE('',$,#71701);
#71652=PRODUCT_DEFINITION_SHAPE('',$,#71702);
#71653=PRODUCT_DEFINITION_SHAPE('',$,#71703);
#71654=PRODUCT_DEFINITION_SHAPE('',$,#71704);
#71655=PRODUCT_DEFINITION_SHAPE('',$,#71705);
#71656=PRODUCT_DEFINITION_SHAPE('',$,#71706);
#71657=PRODUCT_DEFINITION_SHAPE('',$,#71707);
#71658=PRODUCT_DEFINITION_SHAPE('',$,#71708);
#71659=PRODUCT_DEFINITION_SHAPE('',$,#71709);
#71660=PRODUCT_DEFINITION_SHAPE('',$,#71710);
#71661=PRODUCT_DEFINITION_SHAPE($,$,#74);
#71662=PRODUCT_DEFINITION_SHAPE($,$,#75);
#71663=PRODUCT_DEFINITION_SHAPE($,$,#76);
#71664=PRODUCT_DEFINITION_SHAPE($,$,#77);
#71665=PRODUCT_DEFINITION_SHAPE($,$,#78);
#71666=PRODUCT_DEFINITION_SHAPE($,$,#79);
#71667=PRODUCT_DEFINITION_SHAPE($,$,#80);
#71668=PRODUCT_DEFINITION_SHAPE($,$,#81);
#71669=PRODUCT_DEFINITION_SHAPE($,$,#82);
#71670=PRODUCT_DEFINITION_SHAPE($,$,#83);
#71671=PRODUCT_DEFINITION_SHAPE($,$,#84);
#71672=PRODUCT_DEFINITION_SHAPE($,$,#85);
#71673=PRODUCT_DEFINITION_SHAPE($,$,#86);
#71674=PRODUCT_DEFINITION_SHAPE($,$,#87);
#71675=PRODUCT_DEFINITION_SHAPE($,$,#88);
#71676=PRODUCT_DEFINITION_SHAPE($,$,#89);
#71677=PRODUCT_DEFINITION_SHAPE($,$,#90);
#71678=PRODUCT_DEFINITION_SHAPE($,$,#91);
#71679=PRODUCT_DEFINITION_SHAPE($,$,#92);
#71680=PRODUCT_DEFINITION_SHAPE($,$,#93);
#71681=PRODUCT_DEFINITION_SHAPE($,$,#94);
#71682=SHAPE_REPRESENTATION('',(#34365,#37640,#37641,#37642,#37643,#37644,
#37645,#37646,#37647,#37648,#37649,#37650,#37651,#37652,#37653,#37654,#37655,
#37656,#37657,#37658,#37659,#37660),#71614);
#71683=SHAPE_REPRESENTATION('',(#34366),#71615);
#71684=SHAPE_REPRESENTATION('',(#36166),#71616);
#71685=SHAPE_REPRESENTATION('',(#36341),#71617);
#71686=SHAPE_REPRESENTATION('',(#36377),#71618);
#71687=SHAPE_REPRESENTATION('',(#36394),#71619);
#71688=SHAPE_REPRESENTATION('',(#36711),#71620);
#71689=SHAPE_REPRESENTATION('',(#36728),#71621);
#71690=SHAPE_REPRESENTATION('',(#37019),#71622);
#71691=SHAPE_REPRESENTATION('',(#37037),#71623);
#71692=SHAPE_REPRESENTATION('',(#37185),#71624);
#71693=SHAPE_REPRESENTATION('',(#37215),#71625);
#71694=SHAPE_REPRESENTATION('',(#37269),#71626);
#71695=SHAPE_REPRESENTATION('',(#37583),#71627);
#71696=PRODUCT_DEFINITION_CONTEXT('part definition',#71740,'design');
#71697=PRODUCT_DEFINITION('2026-10-25-00-23-46-966','MAS-498',#71711,#71696);
#71698=PRODUCT_DEFINITION('2026-10-25-00-23-47-869',
'01_Hub_Drum_10x2.25_5on4.5_3500lb',#71712,#71696);
#71699=PRODUCT_DEFINITION('2026-10-25-00-23-52-849',
'10_Spindle_84_3500lb',#71713,#71696);
#71700=PRODUCT_DEFINITION('2026-10-25-00-23-52-198',
'08_Grease_Seal_1.719x2.565_Dexter_10-36',#71714,#71696);
#71701=PRODUCT_DEFINITION('2026-10-25-00-23-51-247',
'05_Inner_Bearing_Cup_L68111',#71715,#71696);
#71702=PRODUCT_DEFINITION('2026-10-25-00-23-50-612',
'04_Inner_Bearing_Cone_L68149',#71716,#71696);
#71703=PRODUCT_DEFINITION('2026-10-25-00-23-52-009',
'07_Outer_Bearing_Cup_L44610',#71717,#71696);
#71704=PRODUCT_DEFINITION('2026-10-25-00-23-51-414',
'06_Outer_Bearing_Cone_L44649',#71718,#71696);
#71705=PRODUCT_DEFINITION('2026-10-25-00-23-54-288',
'11_Spindle_Tang_Washer_1in',#71719,#71696);
#71706=PRODUCT_DEFINITION('2026-10-25-00-23-54-695',
'12_Spindle_Nut_1-14_Slotted',#71720,#71696);
#71707=PRODUCT_DEFINITION('2026-10-25-00-23-55-849',
'13_Cotter_Pin_5-32x1-1-4',#71721,#71696);
#71708=PRODUCT_DEFINITION('2026-10-25-00-23-52-521','09_Dust_Cap_1.98',
#71722,#71696);
#71709=PRODUCT_DEFINITION('2026-10-25-00-23-49-479',
'02_Wheel_Stud_1-2-20_UNF_Knurled',#71723,#71696);
#71710=PRODUCT_DEFINITION('2026-10-25-00-23-50-203',
'03_Lug_Nut_1-2-20_60deg_Cone',#71724,#71696);
#71711=PRODUCT_DEFINITION_FORMATION('',$,#71742);
#71712=PRODUCT_DEFINITION_FORMATION('',$,#71743);
#71713=PRODUCT_DEFINITION_FORMATION('',$,#71744);
#71714=PRODUCT_DEFINITION_FORMATION('',$,#71745);
#71715=PRODUCT_DEFINITION_FORMATION('',$,#71746);
#71716=PRODUCT_DEFINITION_FORMATION('',$,#71747);
#71717=PRODUCT_DEFINITION_FORMATION('',$,#71748);
#71718=PRODUCT_DEFINITION_FORMATION('',$,#71749);
#71719=PRODUCT_DEFINITION_FORMATION('',$,#71750);
#71720=PRODUCT_DEFINITION_FORMATION('',$,#71751);
#71721=PRODUCT_DEFINITION_FORMATION('',$,#71752);
#71722=PRODUCT_DEFINITION_FORMATION('',$,#71753);
#71723=PRODUCT_DEFINITION_FORMATION('',$,#71754);
#71724=PRODUCT_DEFINITION_FORMATION('',$,#71755);
#71725=PRODUCT_RELATED_PRODUCT_CATEGORY('MAS-498','MAS-498',(#71742));
#71726=PRODUCT_RELATED_PRODUCT_CATEGORY(
'01_Hub_Drum_10x2.25_5on4.5_3500lb','01_Hub_Drum_10x2.25_5on4.5_3500lb',
(#71743));
#71727=PRODUCT_RELATED_PRODUCT_CATEGORY('10_Spindle_84_3500lb',
'10_Spindle_84_3500lb',(#71744));
#71728=PRODUCT_RELATED_PRODUCT_CATEGORY(
'08_Grease_Seal_1.719x2.565_Dexter_10-36',
'08_Grease_Seal_1.719x2.565_Dexter_10-36',(#71745));
#71729=PRODUCT_RELATED_PRODUCT_CATEGORY('05_Inner_Bearing_Cup_L68111',
'05_Inner_Bearing_Cup_L68111',(#71746));
#71730=PRODUCT_RELATED_PRODUCT_CATEGORY('04_Inner_Bearing_Cone_L68149',
'04_Inner_Bearing_Cone_L68149',(#71747));
#71731=PRODUCT_RELATED_PRODUCT_CATEGORY('07_Outer_Bearing_Cup_L44610',
'07_Outer_Bearing_Cup_L44610',(#71748));
#71732=PRODUCT_RELATED_PRODUCT_CATEGORY('06_Outer_Bearing_Cone_L44649',
'06_Outer_Bearing_Cone_L44649',(#71749));
#71733=PRODUCT_RELATED_PRODUCT_CATEGORY('11_Spindle_Tang_Washer_1in',
'11_Spindle_Tang_Washer_1in',(#71750));
#71734=PRODUCT_RELATED_PRODUCT_CATEGORY('12_Spindle_Nut_1-14_Slotted',
'12_Spindle_Nut_1-14_Slotted',(#71751));
#71735=PRODUCT_RELATED_PRODUCT_CATEGORY('13_Cotter_Pin_5-32x1-1-4',
'13_Cotter_Pin_5-32x1-1-4',(#71752));
#71736=PRODUCT_RELATED_PRODUCT_CATEGORY('09_Dust_Cap_1.98',
'09_Dust_Cap_1.98',(#71753));
#71737=PRODUCT_RELATED_PRODUCT_CATEGORY(
'02_Wheel_Stud_1-2-20_UNF_Knurled','02_Wheel_Stud_1-2-20_UNF_Knurled',(#71754));
#71738=PRODUCT_RELATED_PRODUCT_CATEGORY('03_Lug_Nut_1-2-20_60deg_Cone',
'03_Lug_Nut_1-2-20_60deg_Cone',(#71755));
#71739=APPLICATION_PROTOCOL_DEFINITION('international standard',
'automotive_design',2009,#71740);
#71740=APPLICATION_CONTEXT(
'Core Data for Automotive Mechanical Design Process');
#71741=PRODUCT_CONTEXT('part definition',#71740,'mechanical');
#71742=PRODUCT('2026-10-25-00-23-46-966','MAS-498',$,(#71741));
#71743=PRODUCT('2026-10-25-00-23-47-869',
'01_Hub_Drum_10x2.25_5on4.5_3500lb',$,(#71741));
#71744=PRODUCT('2026-10-25-00-23-52-849','10_Spindle_84_3500lb',$,(#71741));
#71745=PRODUCT('2026-10-25-00-23-52-198',
'08_Grease_Seal_1.719x2.565_Dexter_10-36',$,(#71741));
#71746=PRODUCT('2026-10-25-00-23-51-247','05_Inner_Bearing_Cup_L68111',
$,(#71741));
#71747=PRODUCT('2026-10-25-00-23-50-612','04_Inner_Bearing_Cone_L68149',
$,(#71741));
#71748=PRODUCT('2026-10-25-00-23-52-009','07_Outer_Bearing_Cup_L44610',
$,(#71741));
#71749=PRODUCT('2026-10-25-00-23-51-414','06_Outer_Bearing_Cone_L44649',
$,(#71741));
#71750=PRODUCT('2026-10-25-00-23-54-288','11_Spindle_Tang_Washer_1in',$,
(#71741));
#71751=PRODUCT('2026-10-25-00-23-54-695','12_Spindle_Nut_1-14_Slotted',
$,(#71741));
#71752=PRODUCT('2026-10-25-00-23-55-849','13_Cotter_Pin_5-32x1-1-4',$,(#71741));
#71753=PRODUCT('2026-10-25-00-23-52-521','09_Dust_Cap_1.98',$,(#71741));
#71754=PRODUCT('2026-10-25-00-23-49-479',
'02_Wheel_Stud_1-2-20_UNF_Knurled',$,(#71741));
#71755=PRODUCT('2026-10-25-00-23-50-203','03_Lug_Nut_1-2-20_60deg_Cone',
$,(#71741));
#71756=PRESENTATION_STYLE_ASSIGNMENT((#71761));
#71757=PRESENTATION_STYLE_ASSIGNMENT((#71762));
#71758=PRESENTATION_STYLE_ASSIGNMENT((#71763));
#71759=PRESENTATION_STYLE_ASSIGNMENT((#71764));
#71760=PRESENTATION_STYLE_ASSIGNMENT((#71765));
#71761=SURFACE_STYLE_USAGE(.BOTH.,#71766);
#71762=SURFACE_STYLE_USAGE(.BOTH.,#71767);
#71763=SURFACE_STYLE_USAGE(.BOTH.,#71768);
#71764=SURFACE_STYLE_USAGE(.BOTH.,#71769);
#71765=SURFACE_STYLE_USAGE(.BOTH.,#71770);
#71766=SURFACE_SIDE_STYLE('',(#71771));
#71767=SURFACE_SIDE_STYLE('',(#71772));
#71768=SURFACE_SIDE_STYLE('',(#71773));
#71769=SURFACE_SIDE_STYLE('',(#71774));
#71770=SURFACE_SIDE_STYLE('',(#71775));
#71771=SURFACE_STYLE_FILL_AREA(#71776);
#71772=SURFACE_STYLE_FILL_AREA(#71777);
#71773=SURFACE_STYLE_FILL_AREA(#71778);
#71774=SURFACE_STYLE_FILL_AREA(#71779);
#71775=SURFACE_STYLE_FILL_AREA(#71780);
#71776=FILL_AREA_STYLE('Steel - Satin',(#71781));
#71777=FILL_AREA_STYLE('MAS496_gun',(#71782));
#71778=FILL_AREA_STYLE('MAS496_ti',(#71783));
#71779=FILL_AREA_STYLE('MAS496_ss',(#71784));
#71780=FILL_AREA_STYLE('MAS496_al',(#71785));
#71781=FILL_AREA_STYLE_COLOUR('Steel - Satin',#71786);
#71782=FILL_AREA_STYLE_COLOUR('MAS496_gun',#71787);
#71783=FILL_AREA_STYLE_COLOUR('MAS496_ti',#71788);
#71784=FILL_AREA_STYLE_COLOUR('MAS496_ss',#71789);
#71785=FILL_AREA_STYLE_COLOUR('MAS496_al',#71790);
#71786=COLOUR_RGB('Steel - Satin',0.627450980392157,0.627450980392157,0.627450980392157);
#71787=COLOUR_RGB('MAS496_gun',0.313725490196078,0.337254901960784,0.364705882352941);
#71788=COLOUR_RGB('MAS496_ti',0.549019607843137,0.572549019607843,0.596078431372549);
#71789=COLOUR_RGB('MAS496_ss',0.83921568627451,0.850980392156863,0.862745098039216);
#71790=COLOUR_RGB('MAS496_al',0.67843137254902,0.705882352941177,0.729411764705882);
#71791=COLOUR_RGB('Dark Blue',0.08,0.2,0.34);
#71792=FILL_AREA_STYLE_COLOUR('',#71791);
#71793=FILL_AREA_STYLE('',(#71792));
#71794=SURFACE_STYLE_FILL_AREA(#71793);
#71795=SURFACE_SIDE_STYLE('',(#71794));
#71796=SURFACE_STYLE_USAGE(.BOTH.,#71795);
#71797=PRESENTATION_STYLE_ASSIGNMENT((#71796));
#71798=COLOUR_RGB('Light Blue',0.38,0.62,0.78);
#71799=FILL_AREA_STYLE_COLOUR('',#71798);
#71800=FILL_AREA_STYLE('',(#71799));
#71801=SURFACE_STYLE_FILL_AREA(#71800);
#71802=SURFACE_SIDE_STYLE('',(#71801));
#71803=SURFACE_STYLE_USAGE(.BOTH.,#71802);
#71804=PRESENTATION_STYLE_ASSIGNMENT((#71803));
#71805=COLOUR_RGB('Sky Blue',0.24,0.69,0.87);
#71806=FILL_AREA_STYLE_COLOUR('',#71805);
#71807=FILL_AREA_STYLE('',(#71806));
#71808=SURFACE_STYLE_FILL_AREA(#71807);
#71809=SURFACE_SIDE_STYLE('',(#71808));
#71810=SURFACE_STYLE_USAGE(.BOTH.,#71809);
#71811=PRESENTATION_STYLE_ASSIGNMENT((#71810));
#71812=COLOUR_RGB('Grey',0.48,0.52,0.57);
#71813=FILL_AREA_STYLE_COLOUR('',#71812);
#71814=FILL_AREA_STYLE('',(#71813));
#71815=SURFACE_STYLE_FILL_AREA(#71814);
#71816=SURFACE_SIDE_STYLE('',(#71815));
#71817=SURFACE_STYLE_USAGE(.BOTH.,#71816);
#71818=PRESENTATION_STYLE_ASSIGNMENT((#71817));
#71819=COLOUR_RGB('Black',0.12,0.14,0.17);
#71820=FILL_AREA_STYLE_COLOUR('',#71819);
#71821=FILL_AREA_STYLE('',(#71820));
#71822=SURFACE_STYLE_FILL_AREA(#71821);
#71823=SURFACE_SIDE_STYLE('',(#71822));
#71824=SURFACE_STYLE_USAGE(.BOTH.,#71823);
#71825=PRESENTATION_STYLE_ASSIGNMENT((#71824));
#71826=COLOUR_RGB('Off White',0.89,0.88,0.83);
#71827=FILL_AREA_STYLE_COLOUR('',#71826);
#71828=FILL_AREA_STYLE('',(#71827));
#71829=SURFACE_STYLE_FILL_AREA(#71828);
#71830=SURFACE_SIDE_STYLE('',(#71829));
#71831=SURFACE_STYLE_USAGE(.BOTH.,#71830);
#71832=PRESENTATION_STYLE_ASSIGNMENT((#71831));
ENDSEC;
END-ISO-10303-21;
